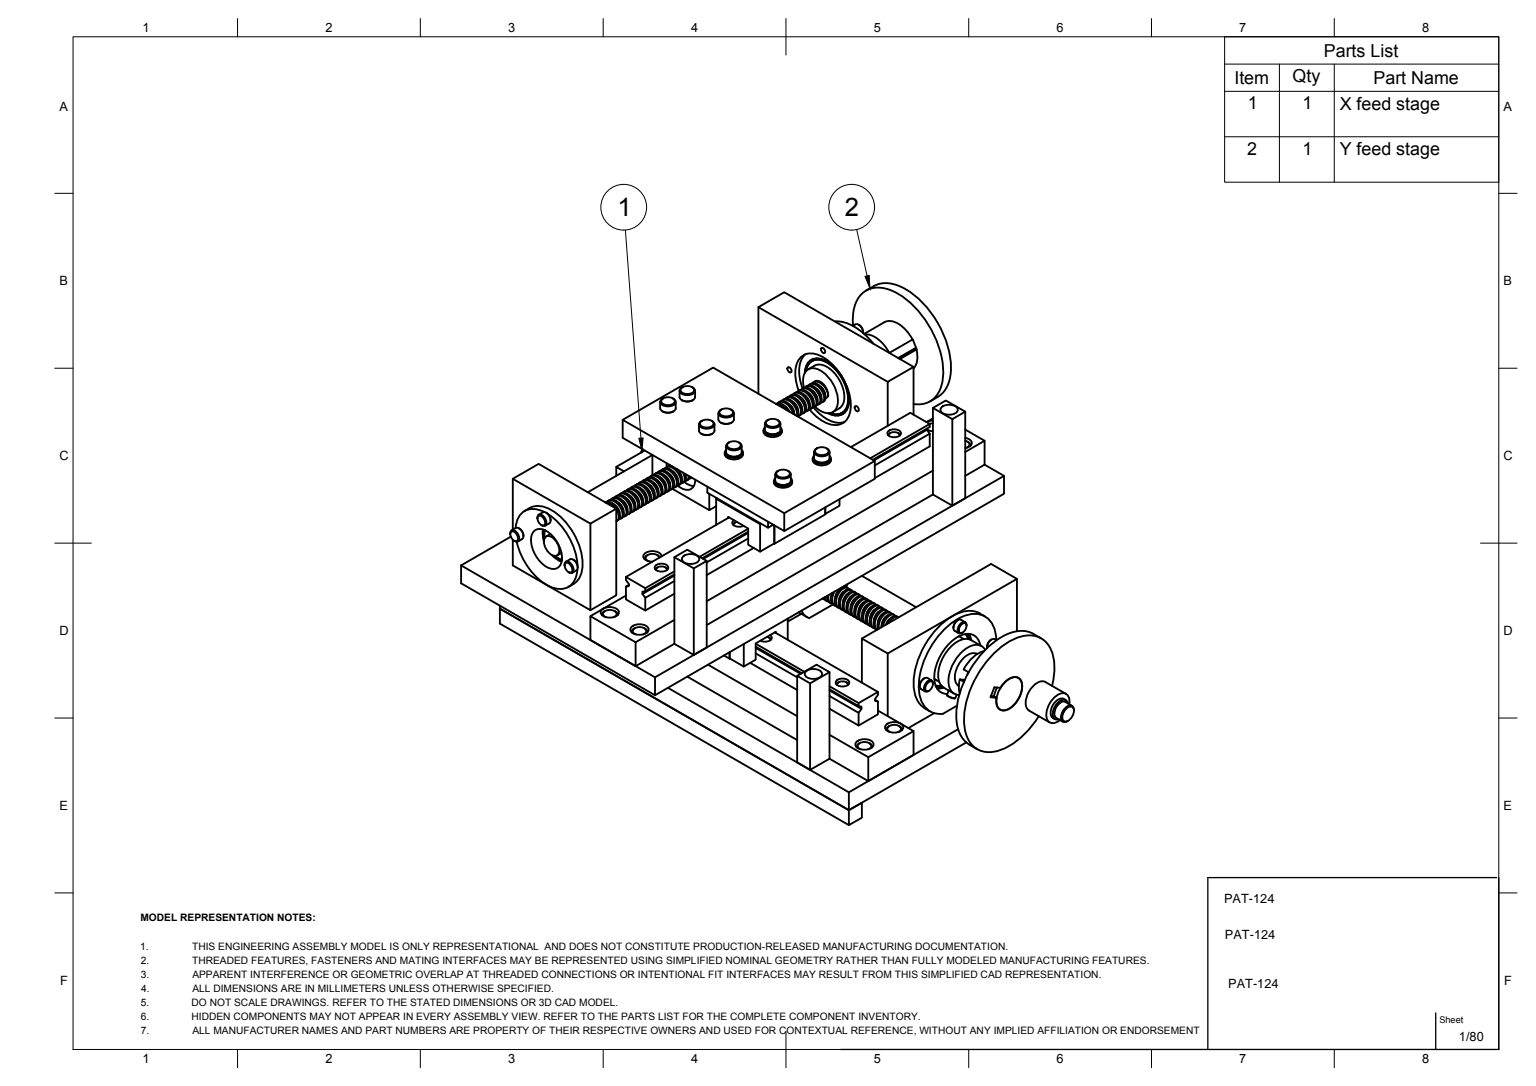
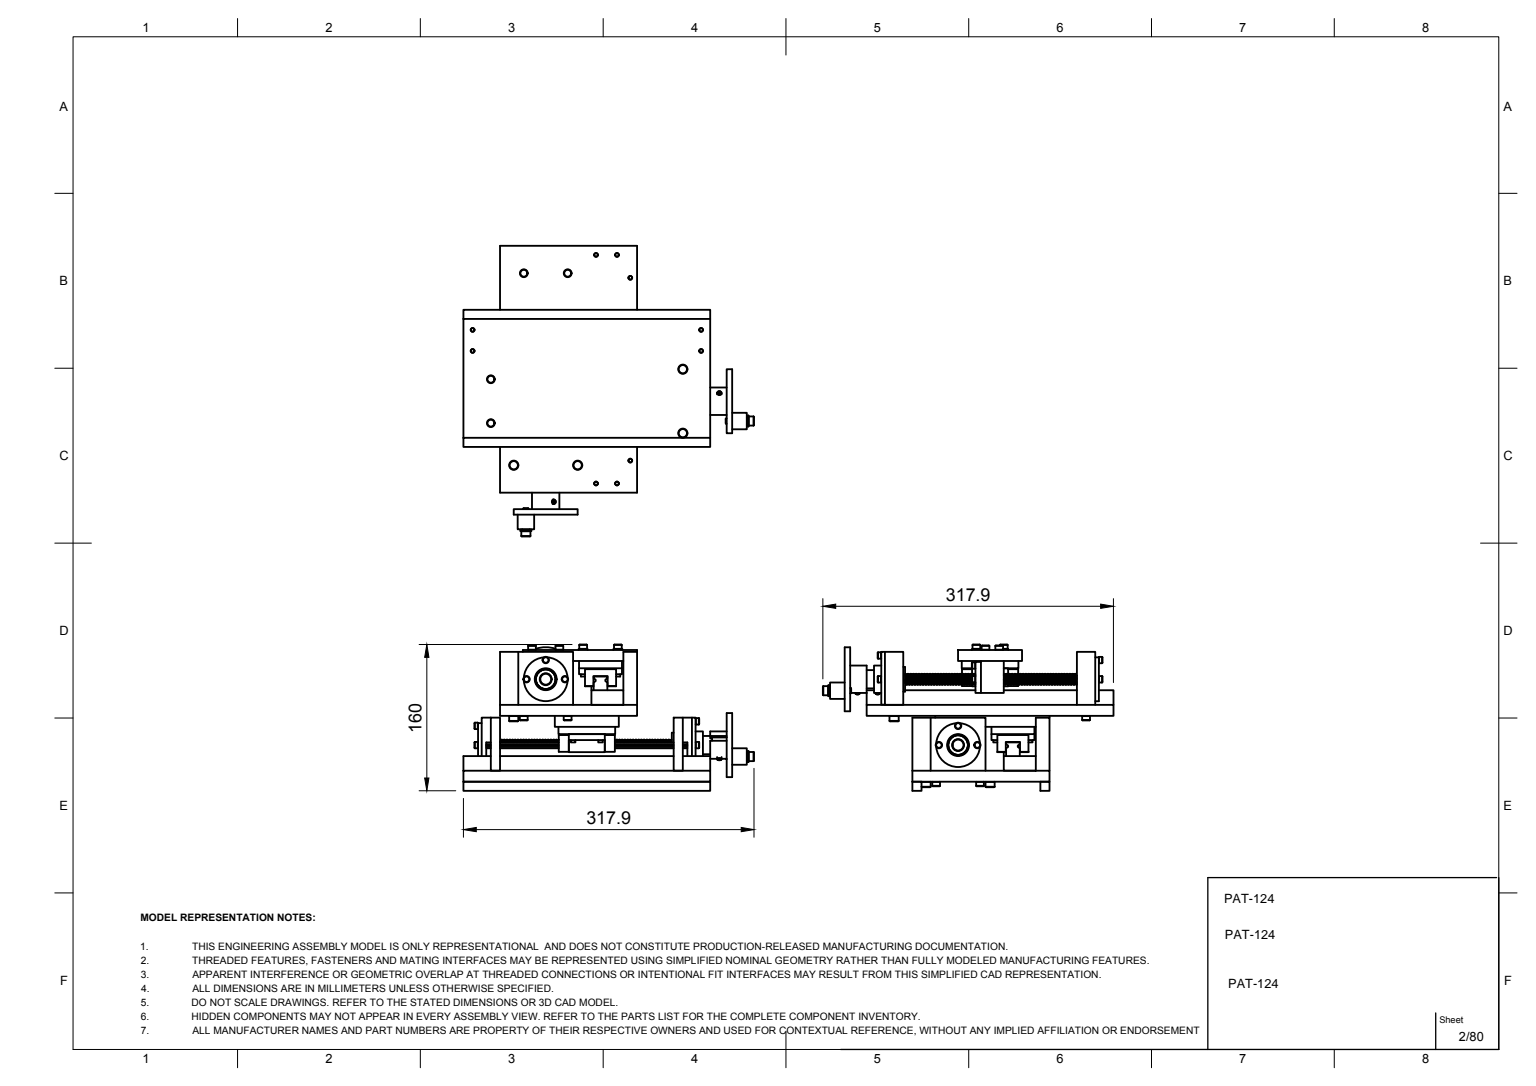
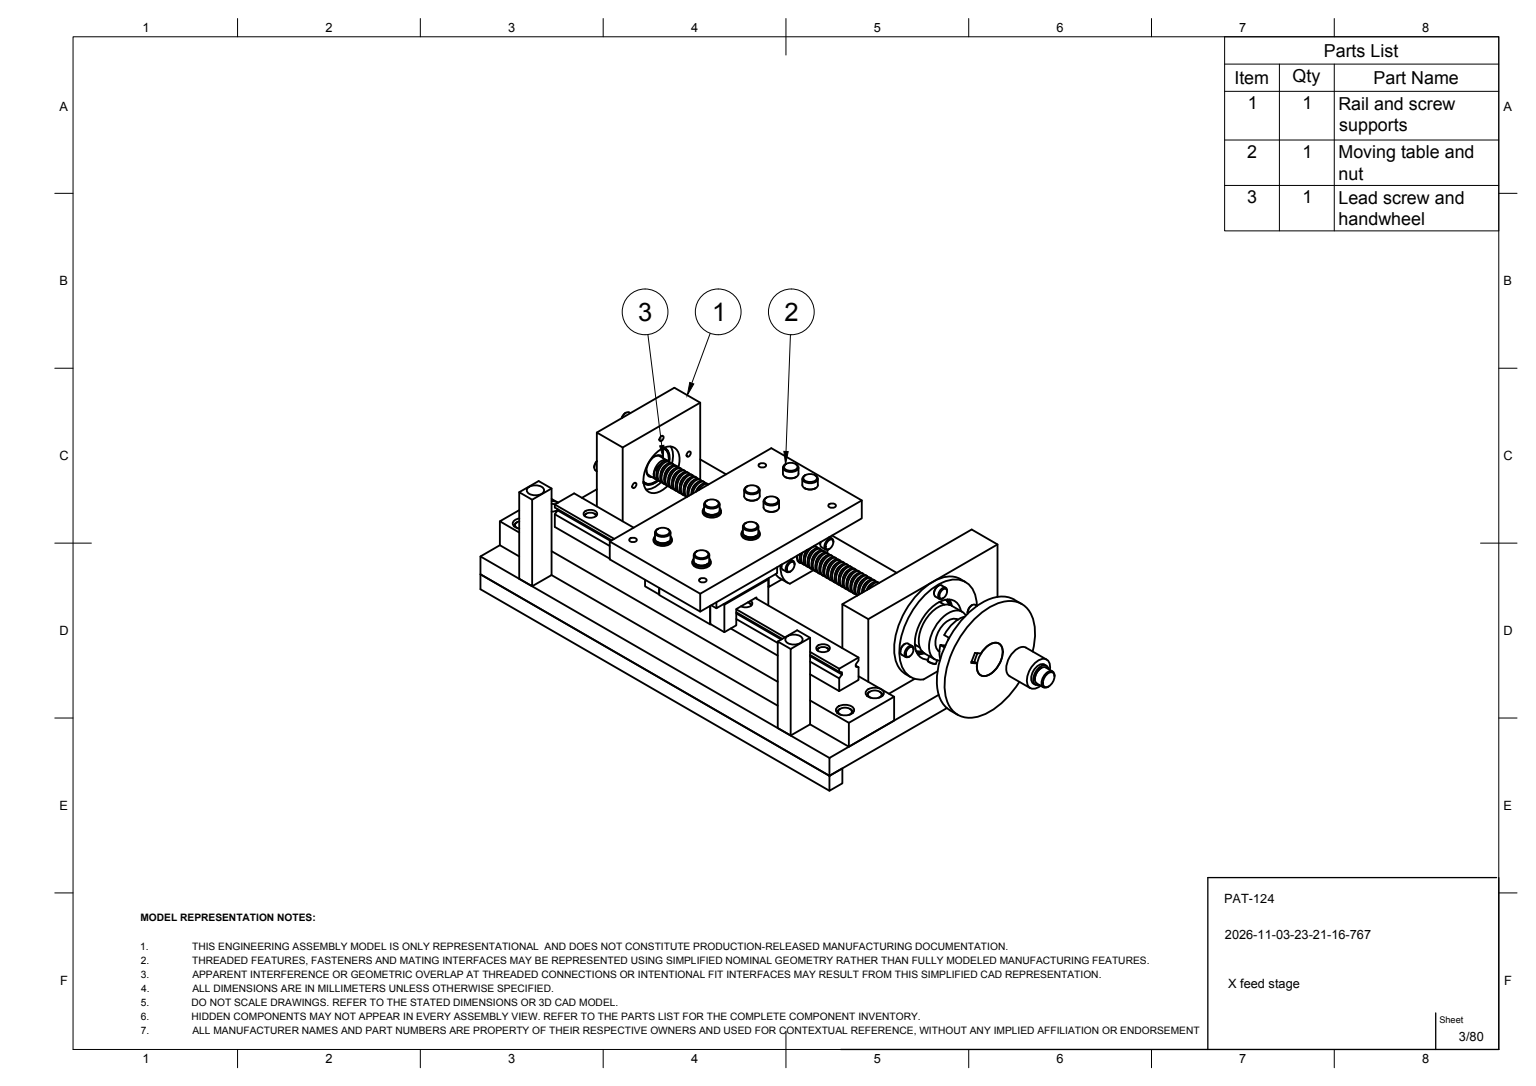
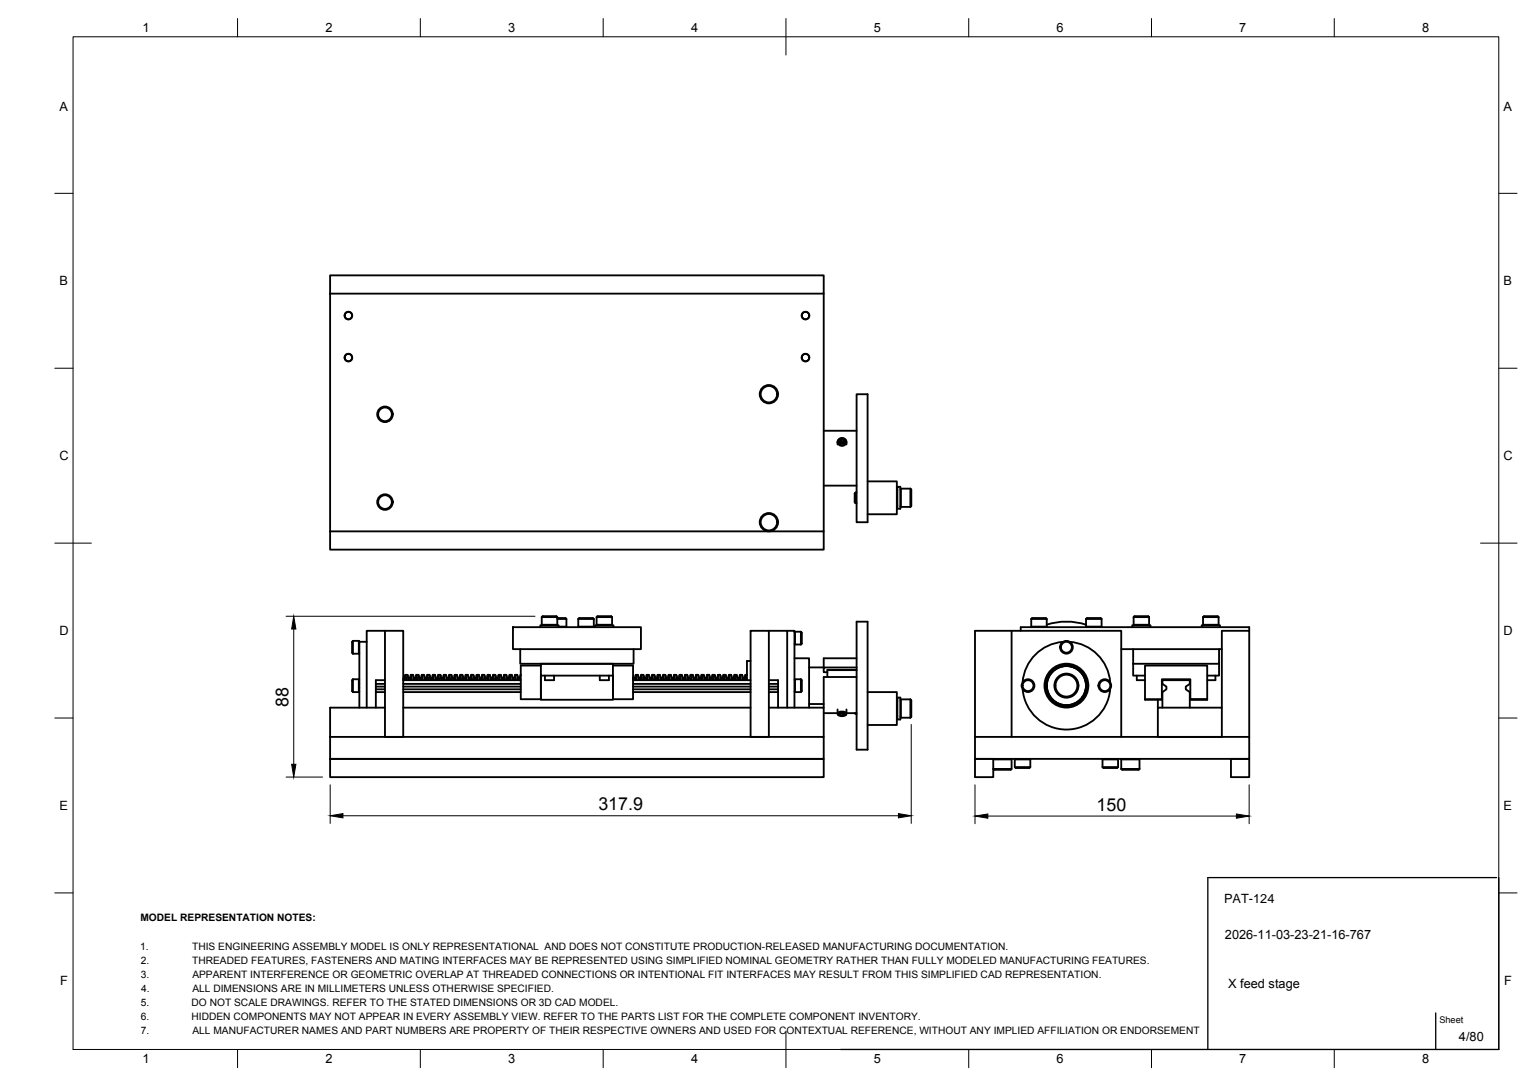
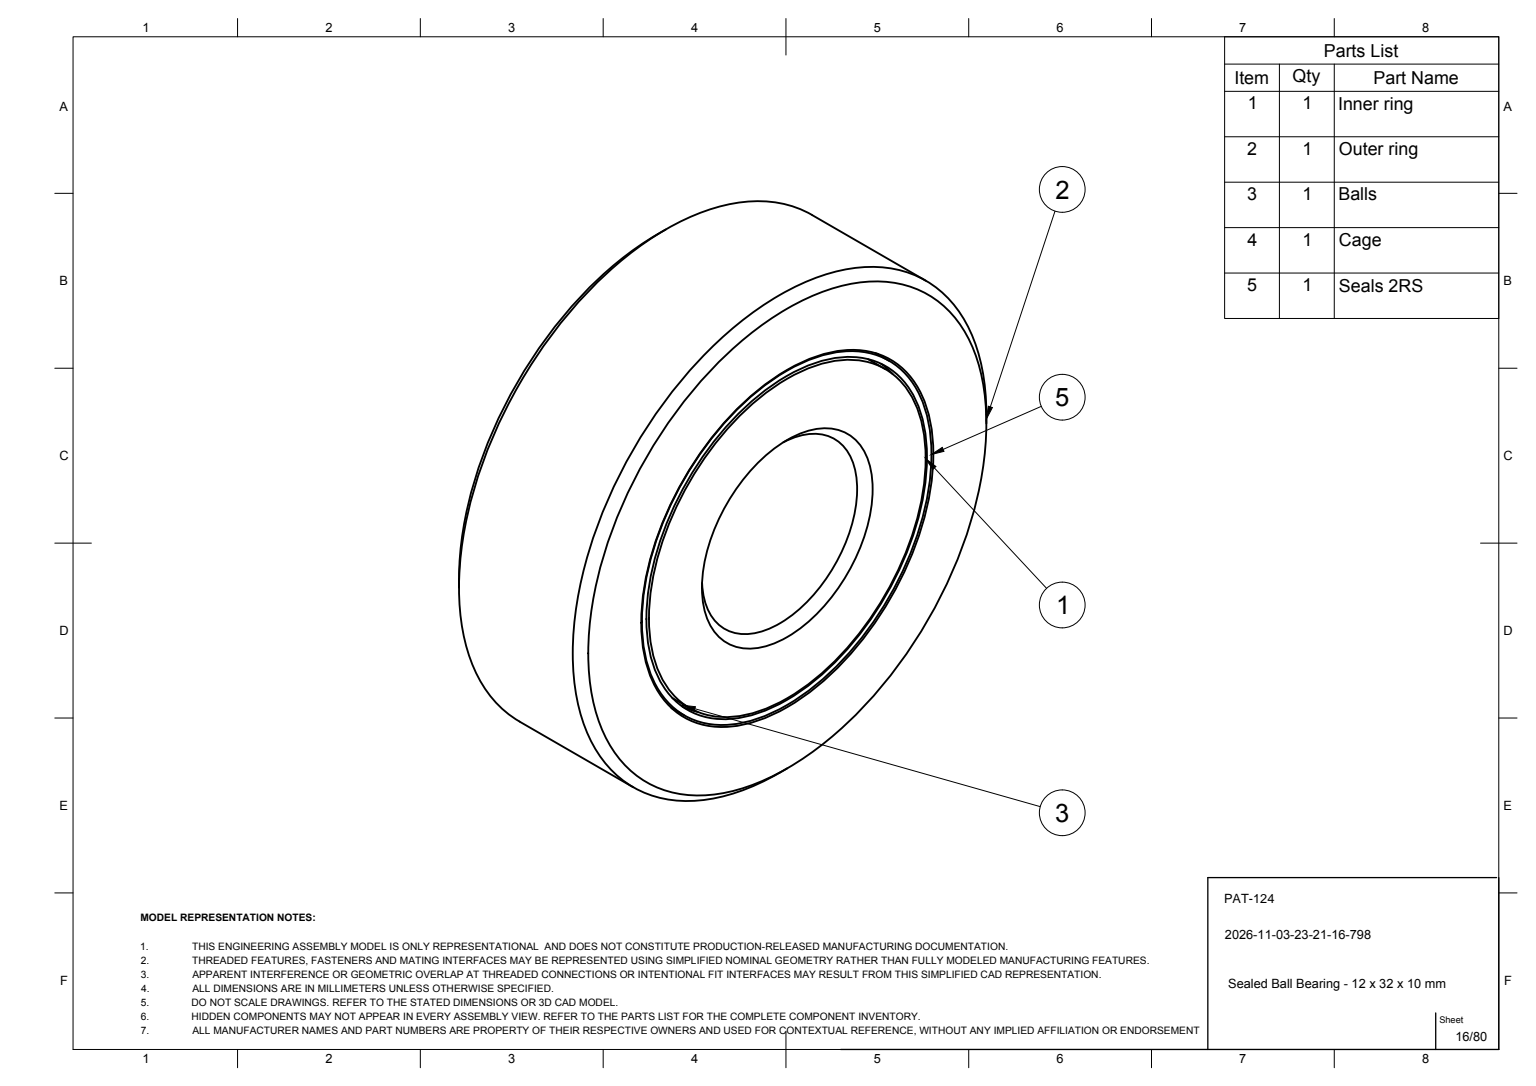
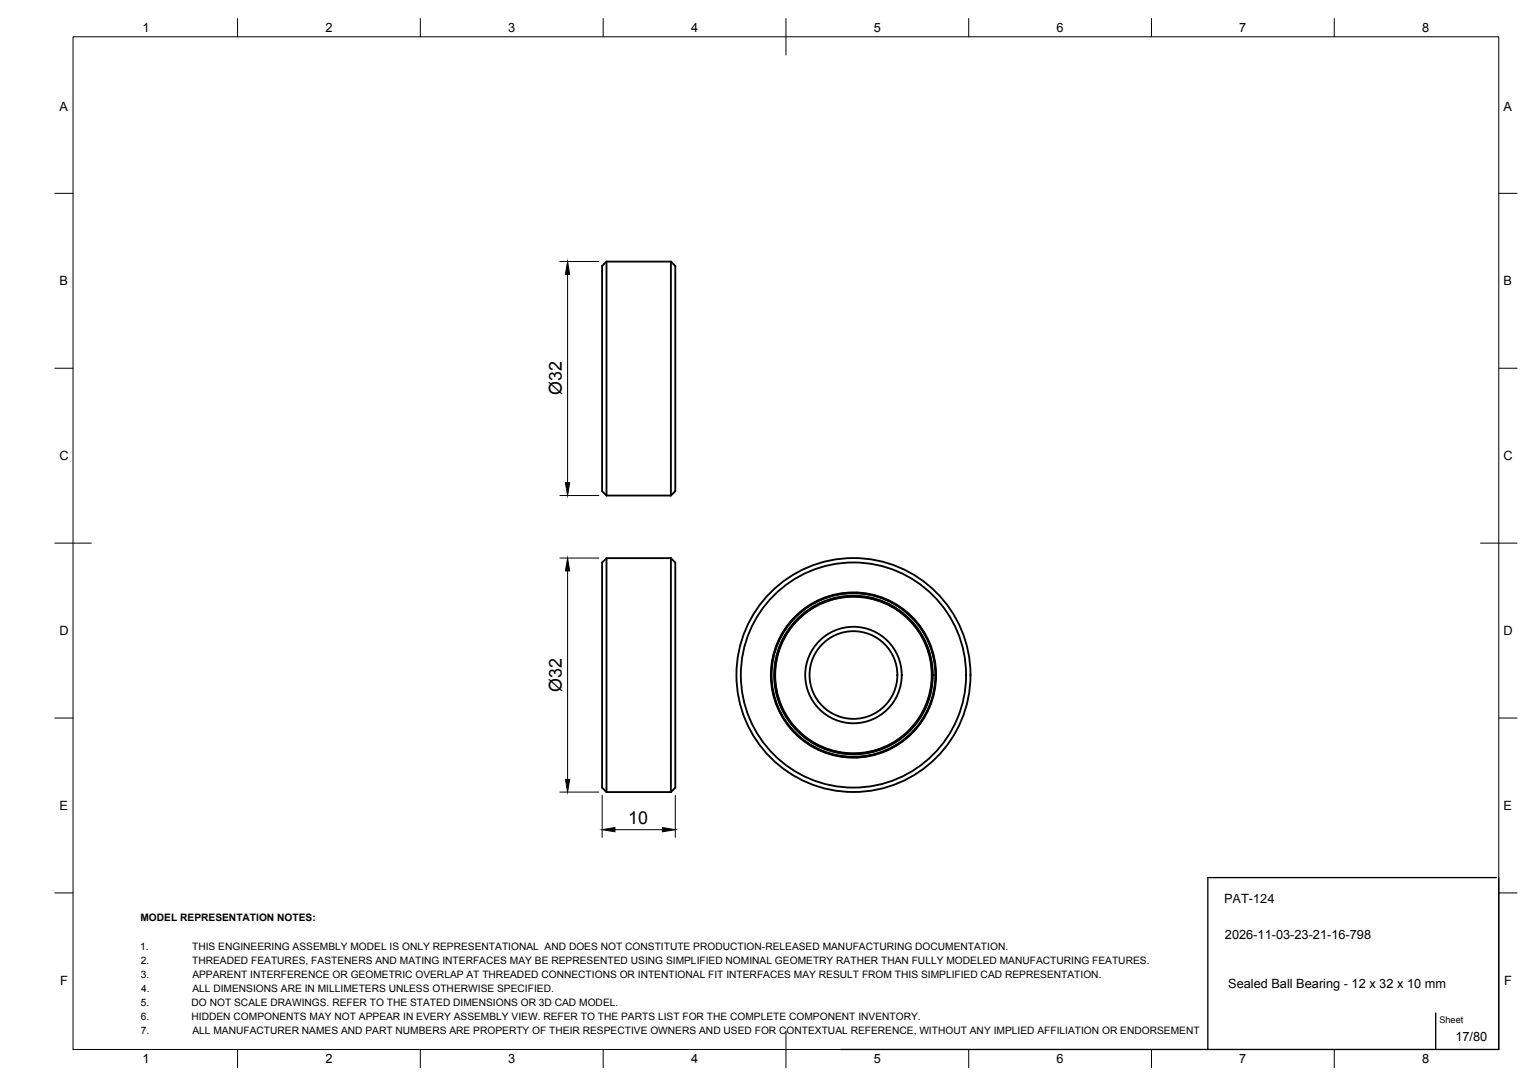
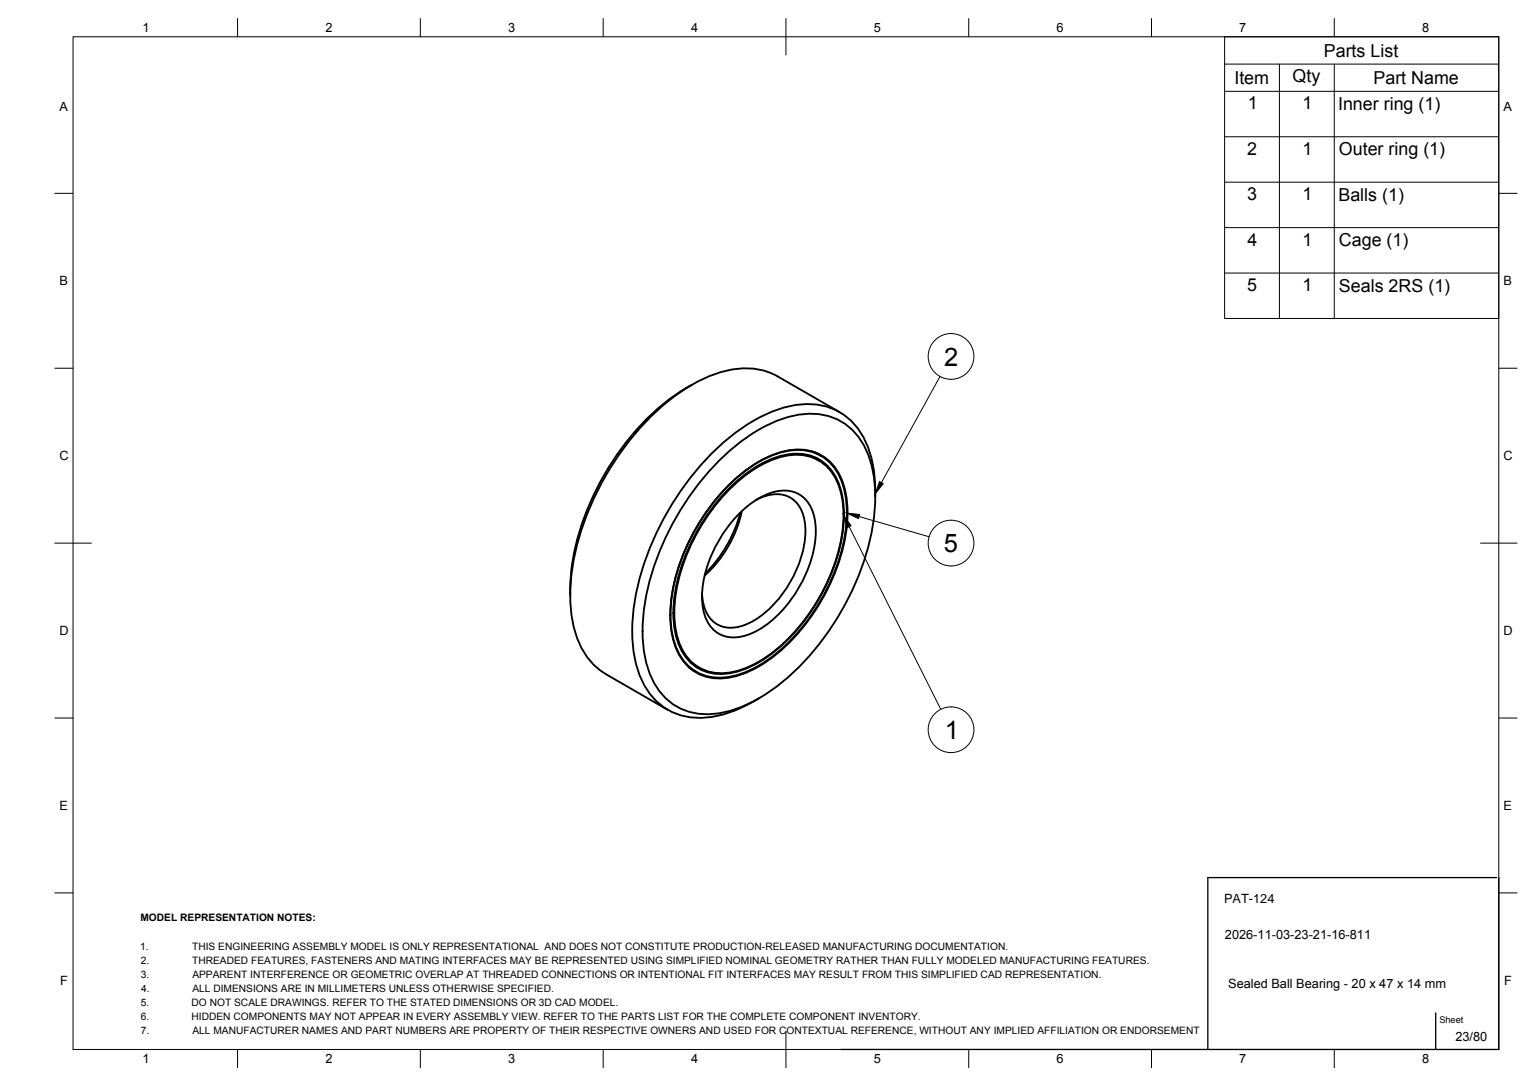
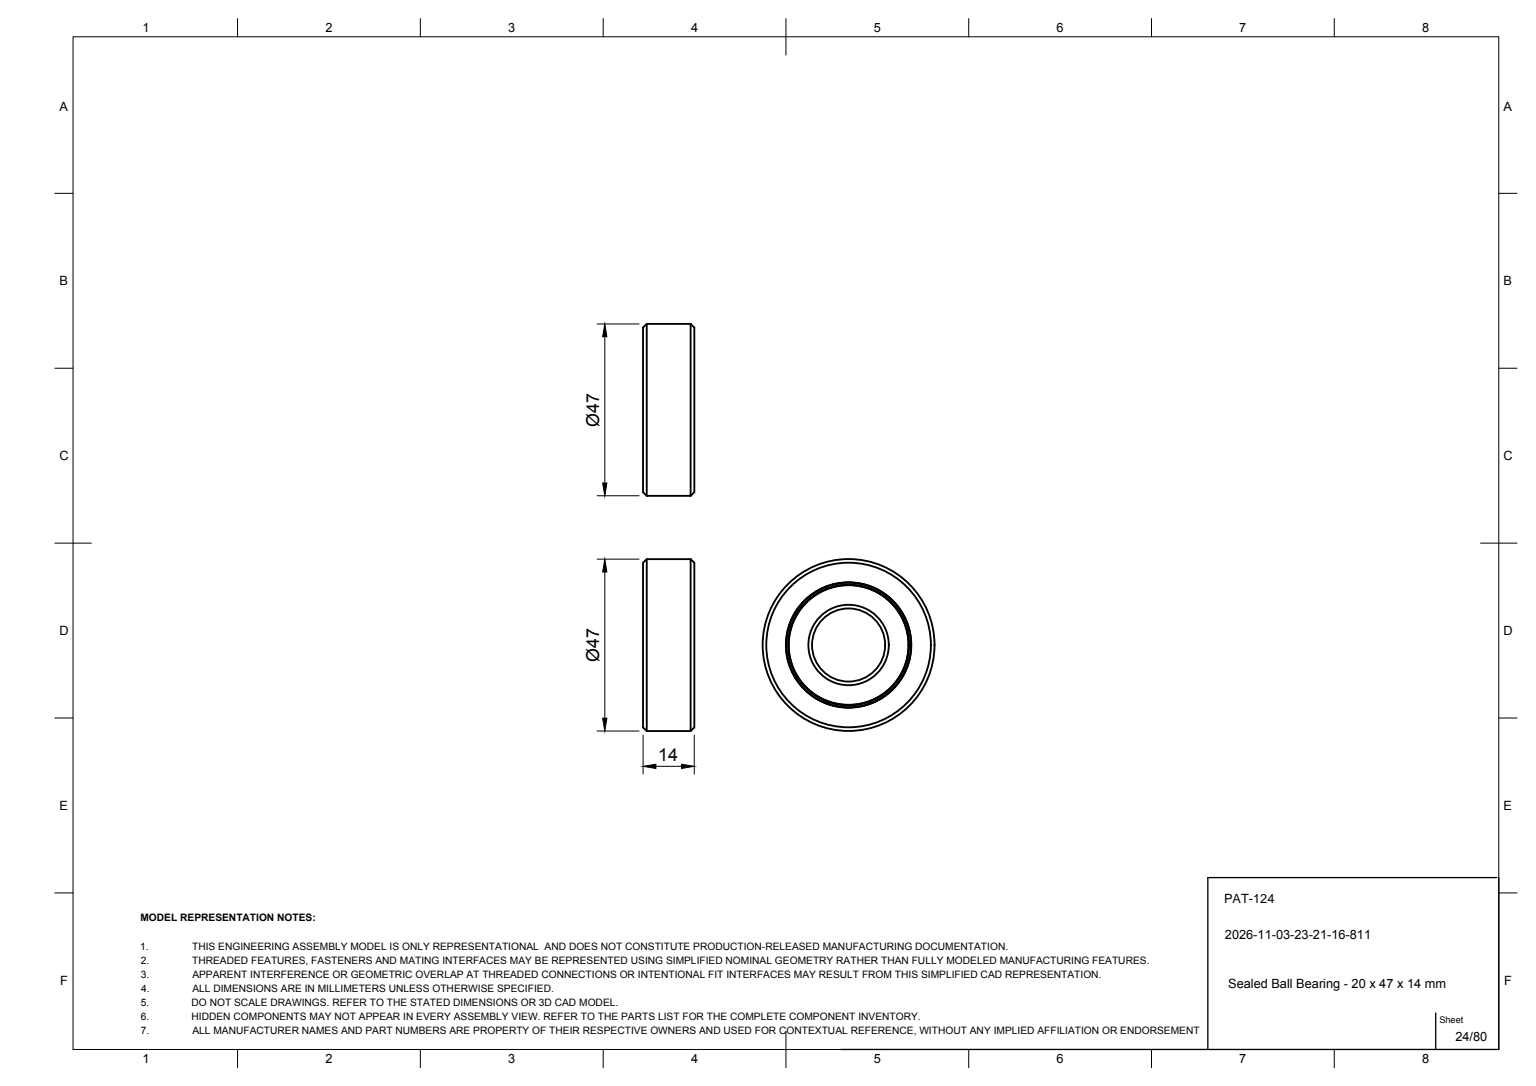
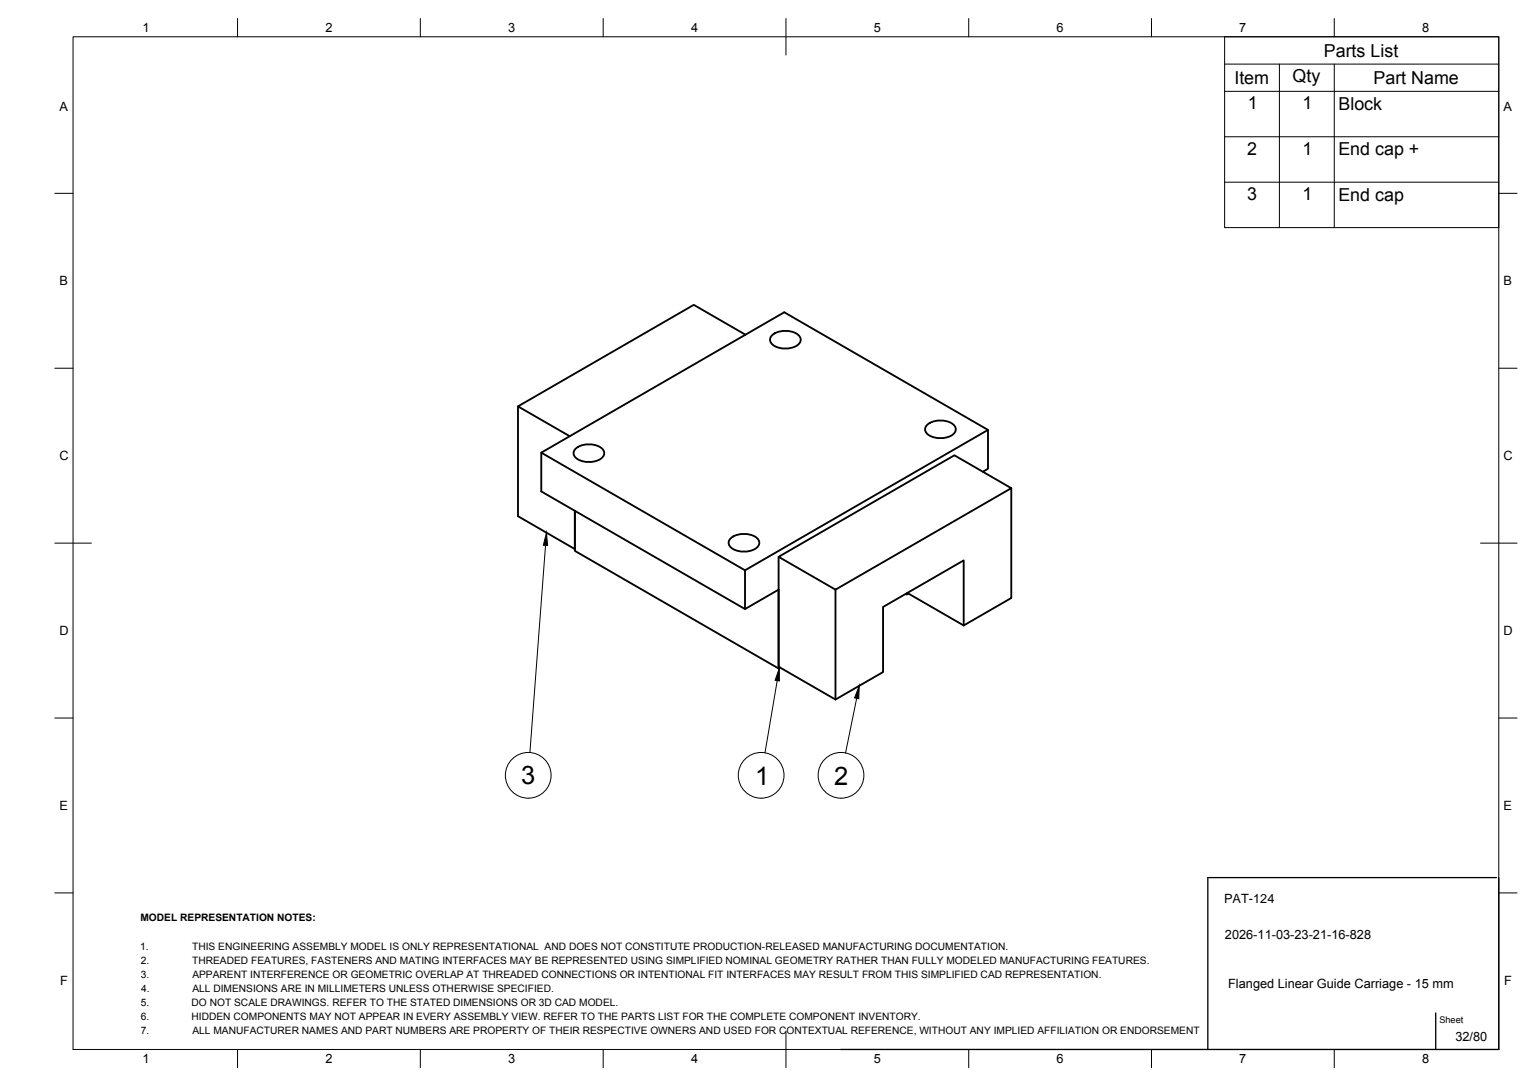
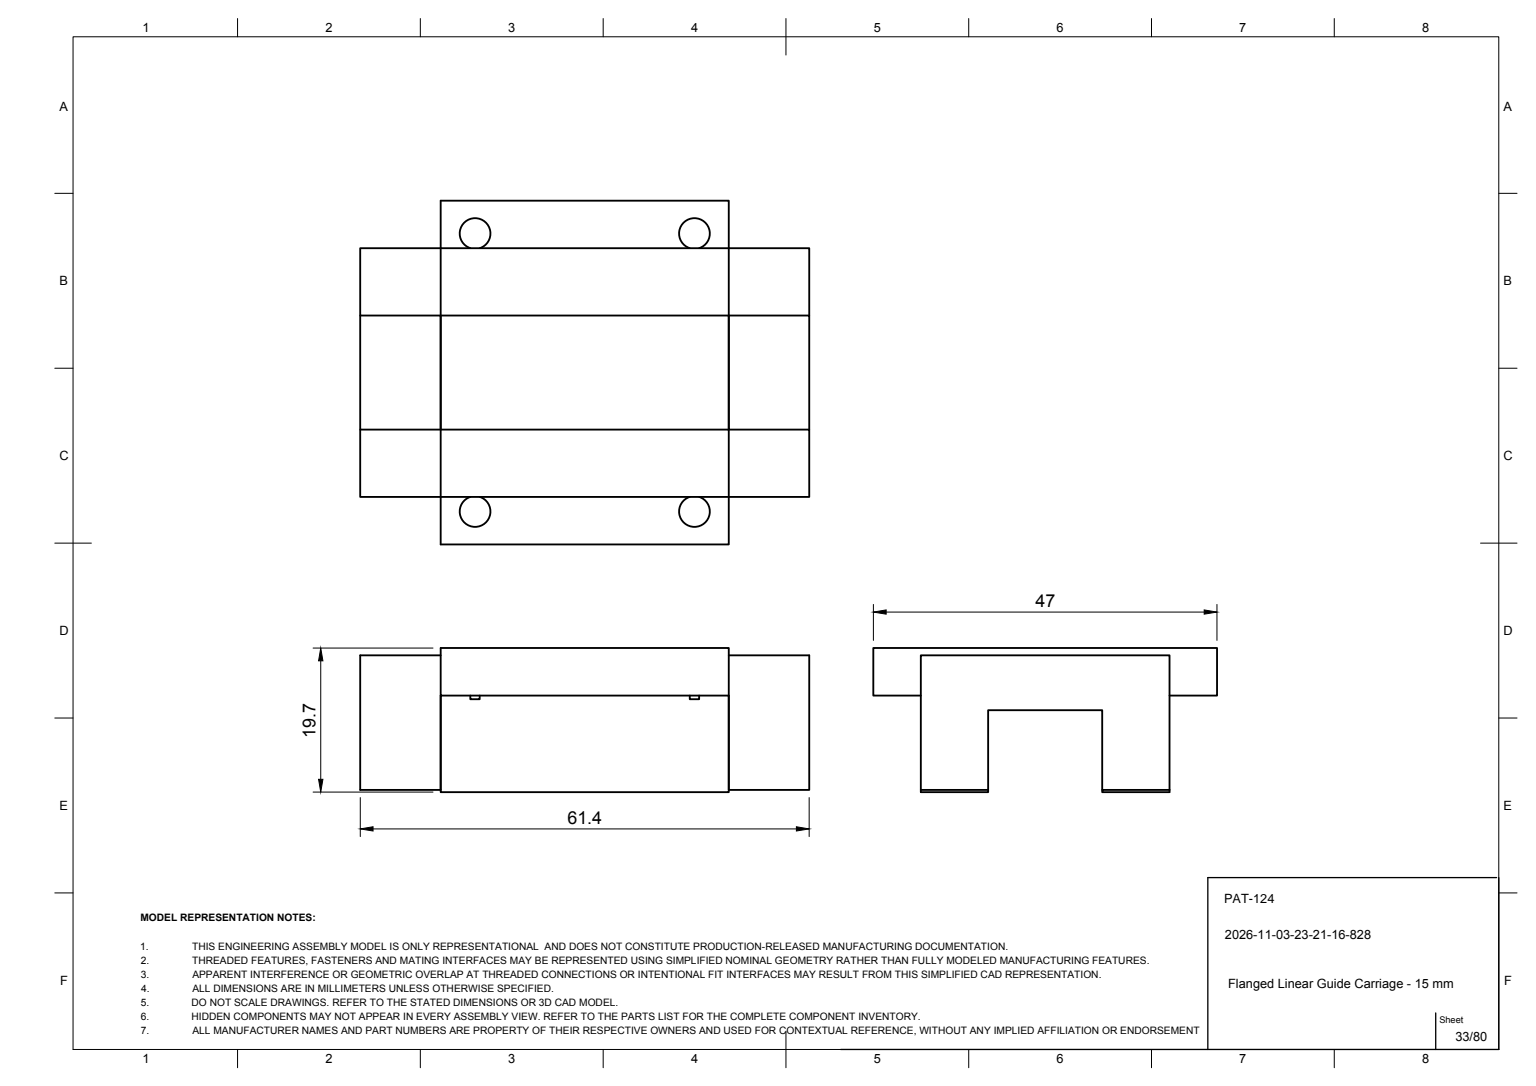
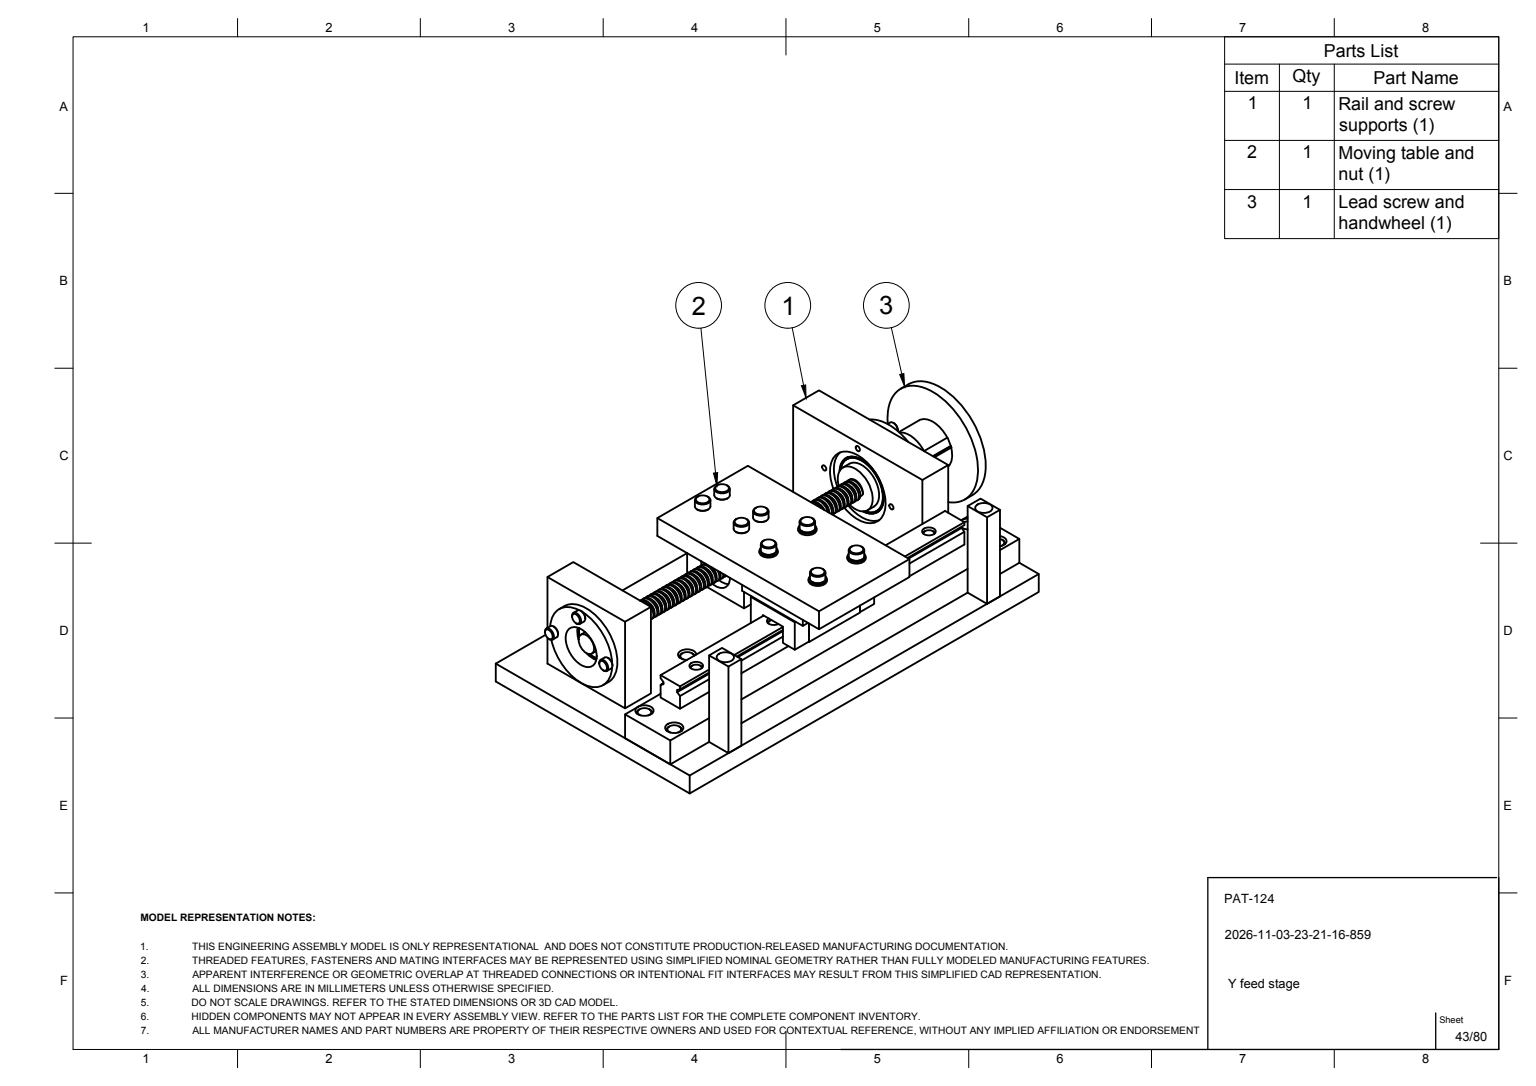
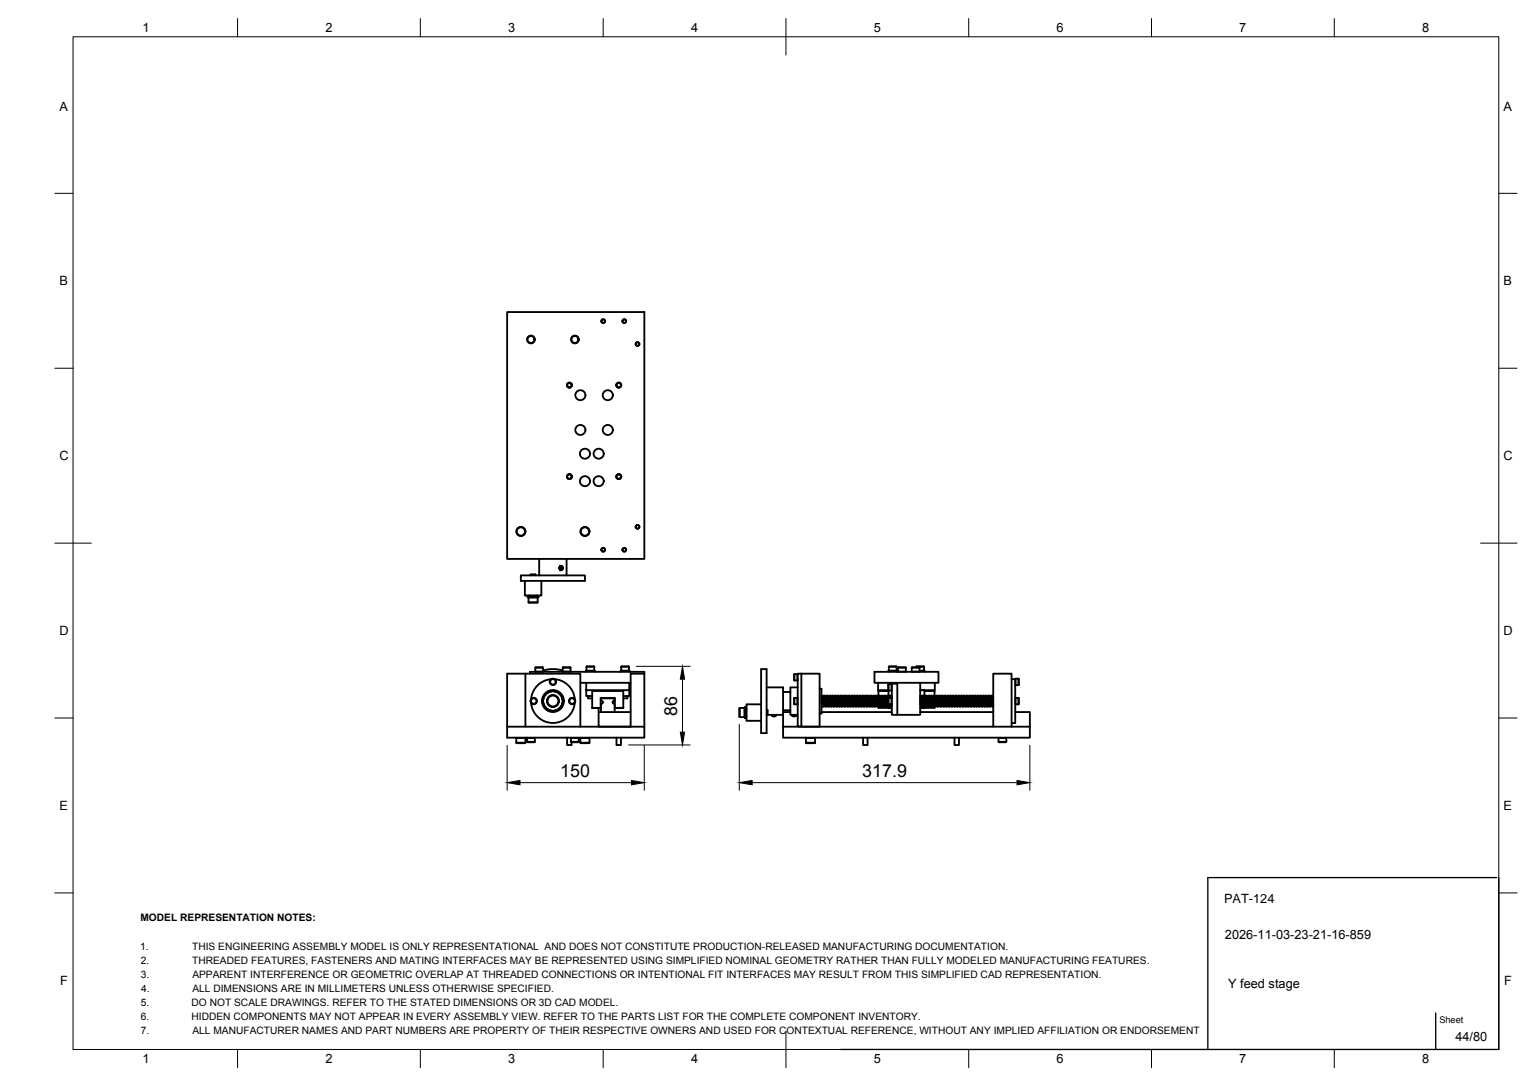
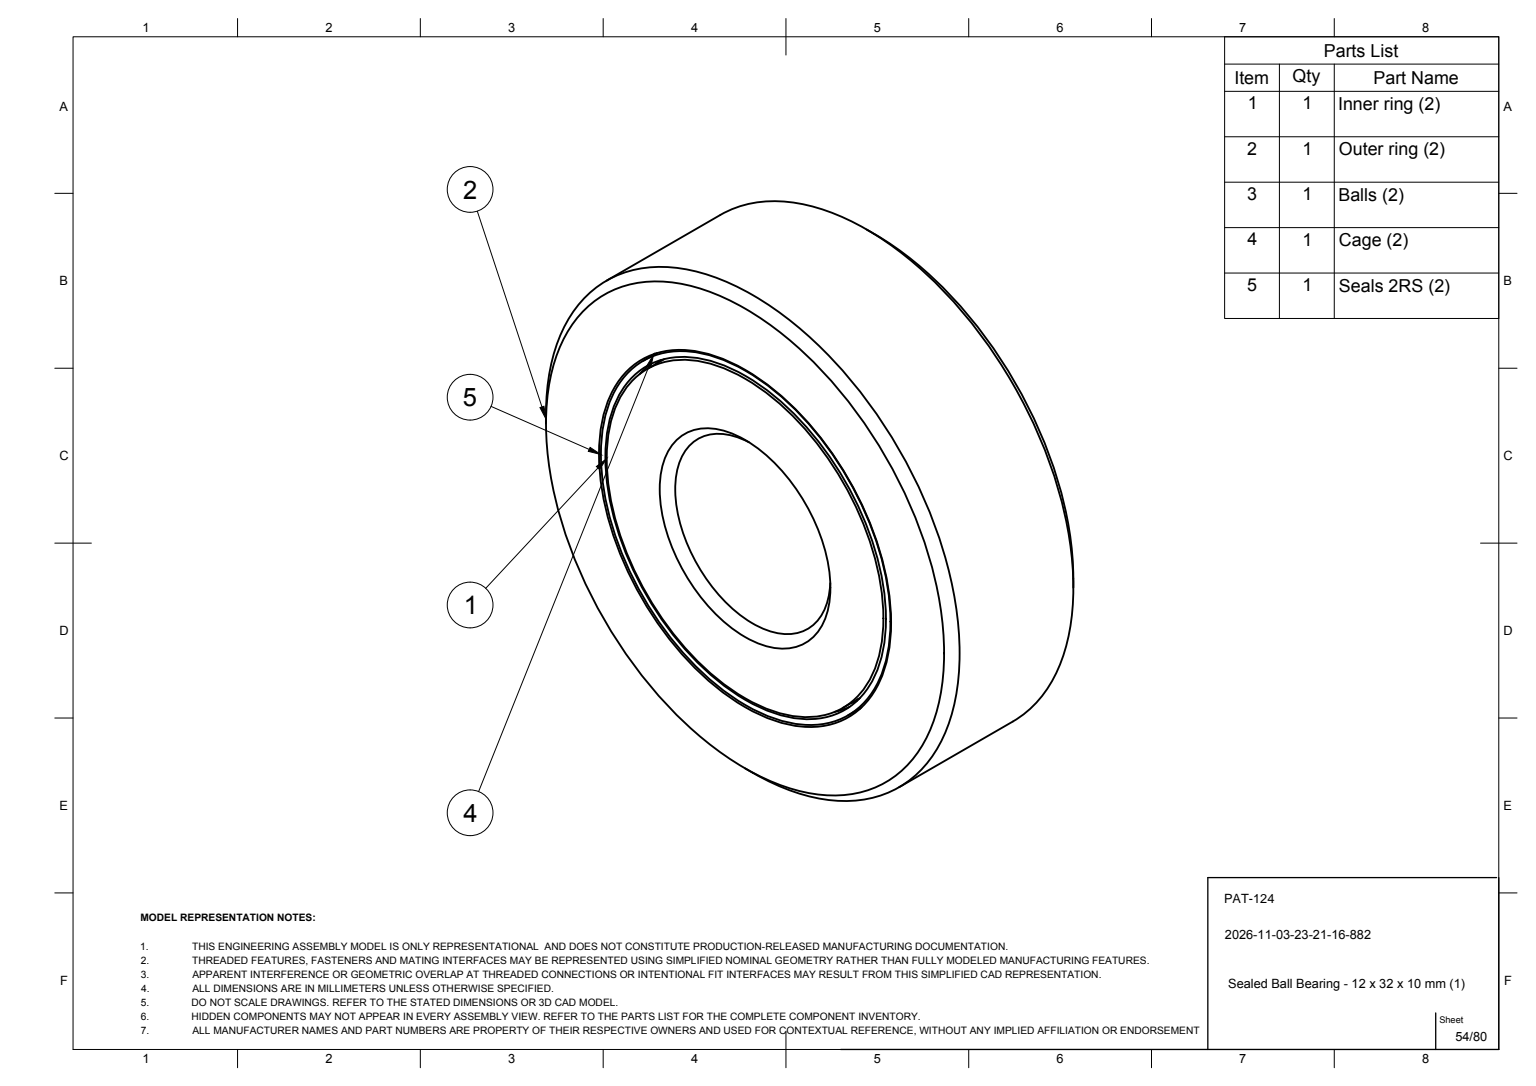
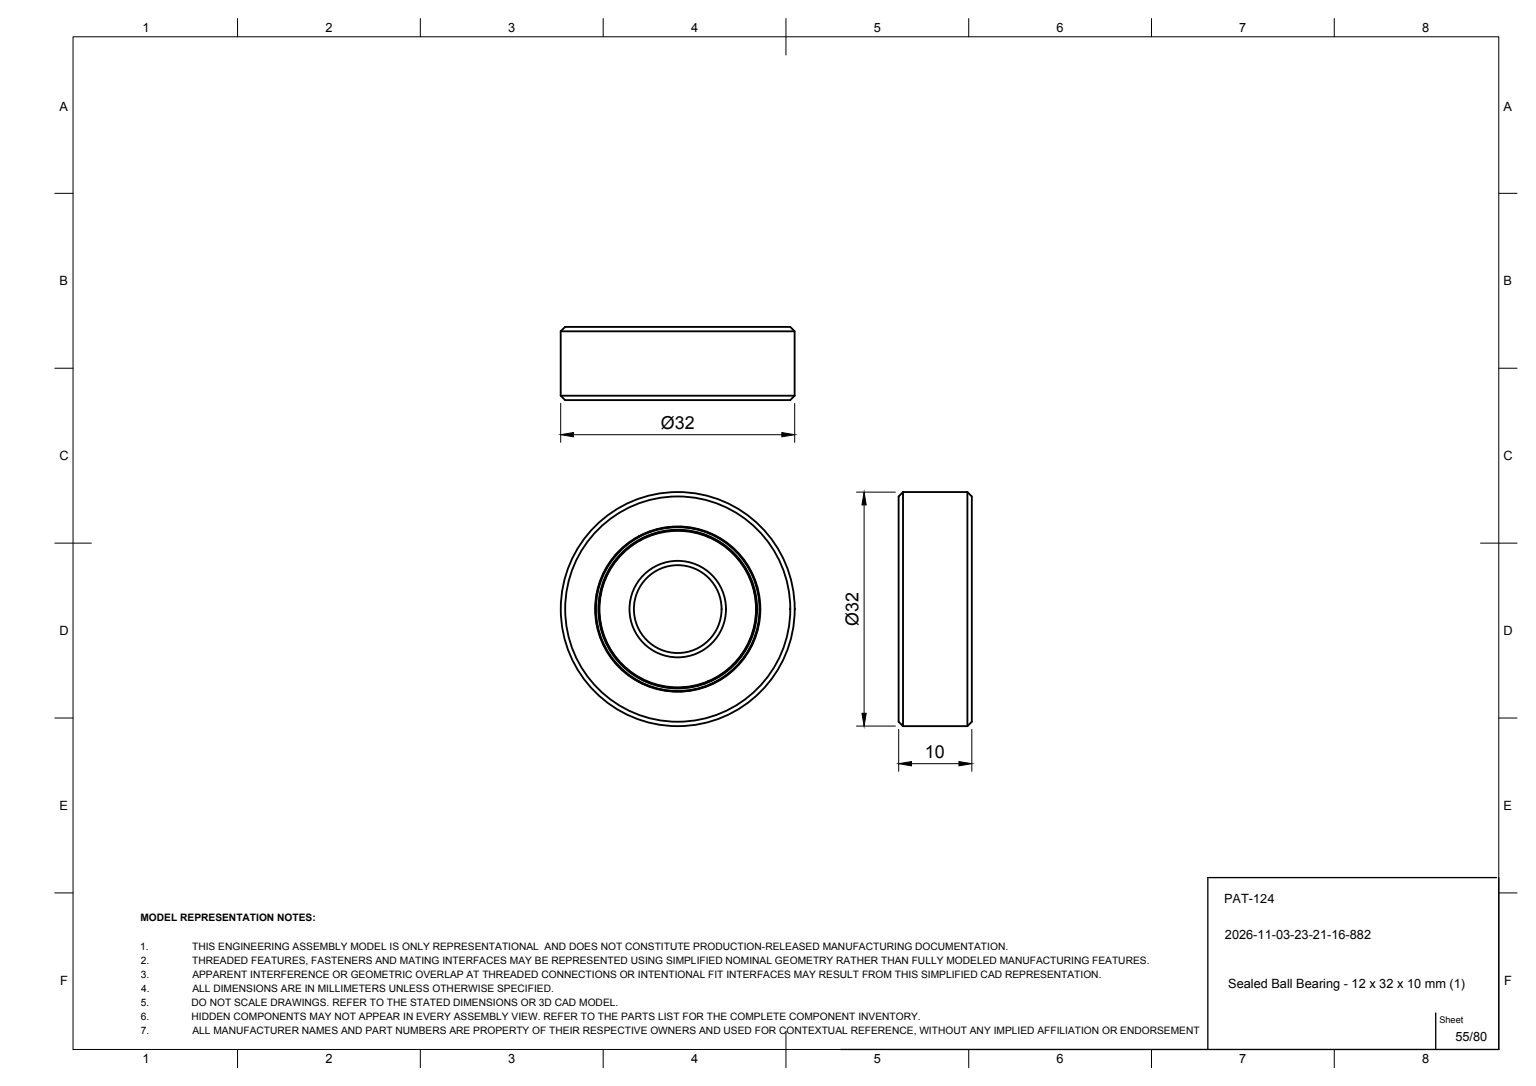
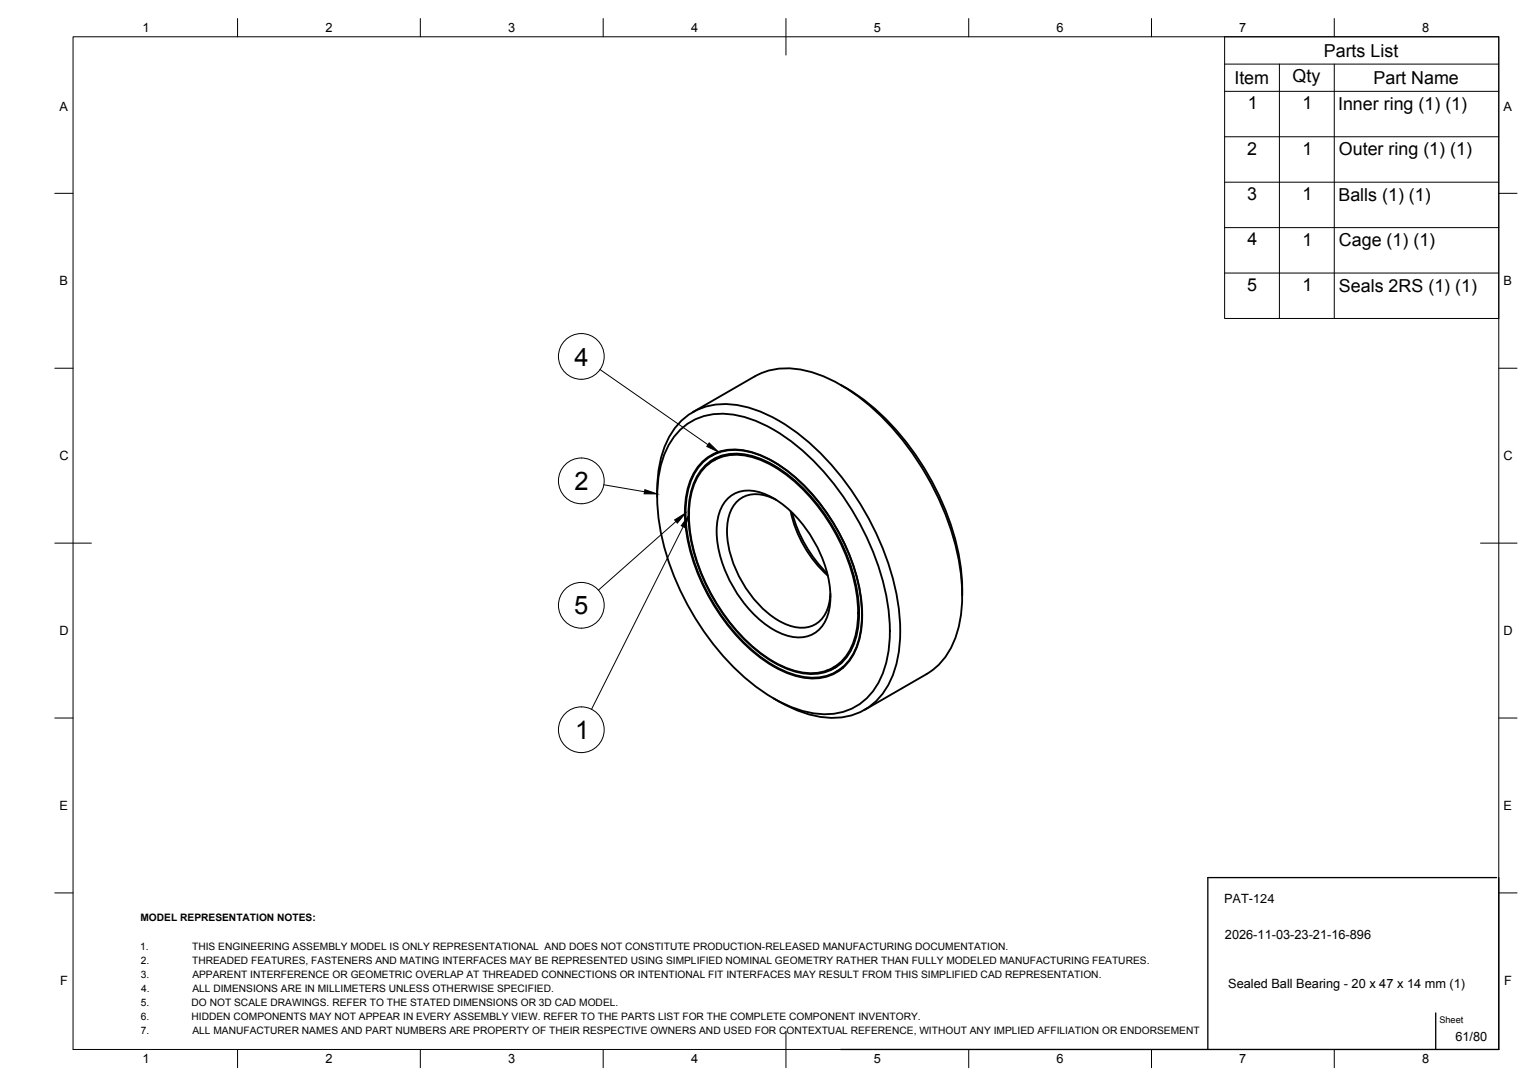
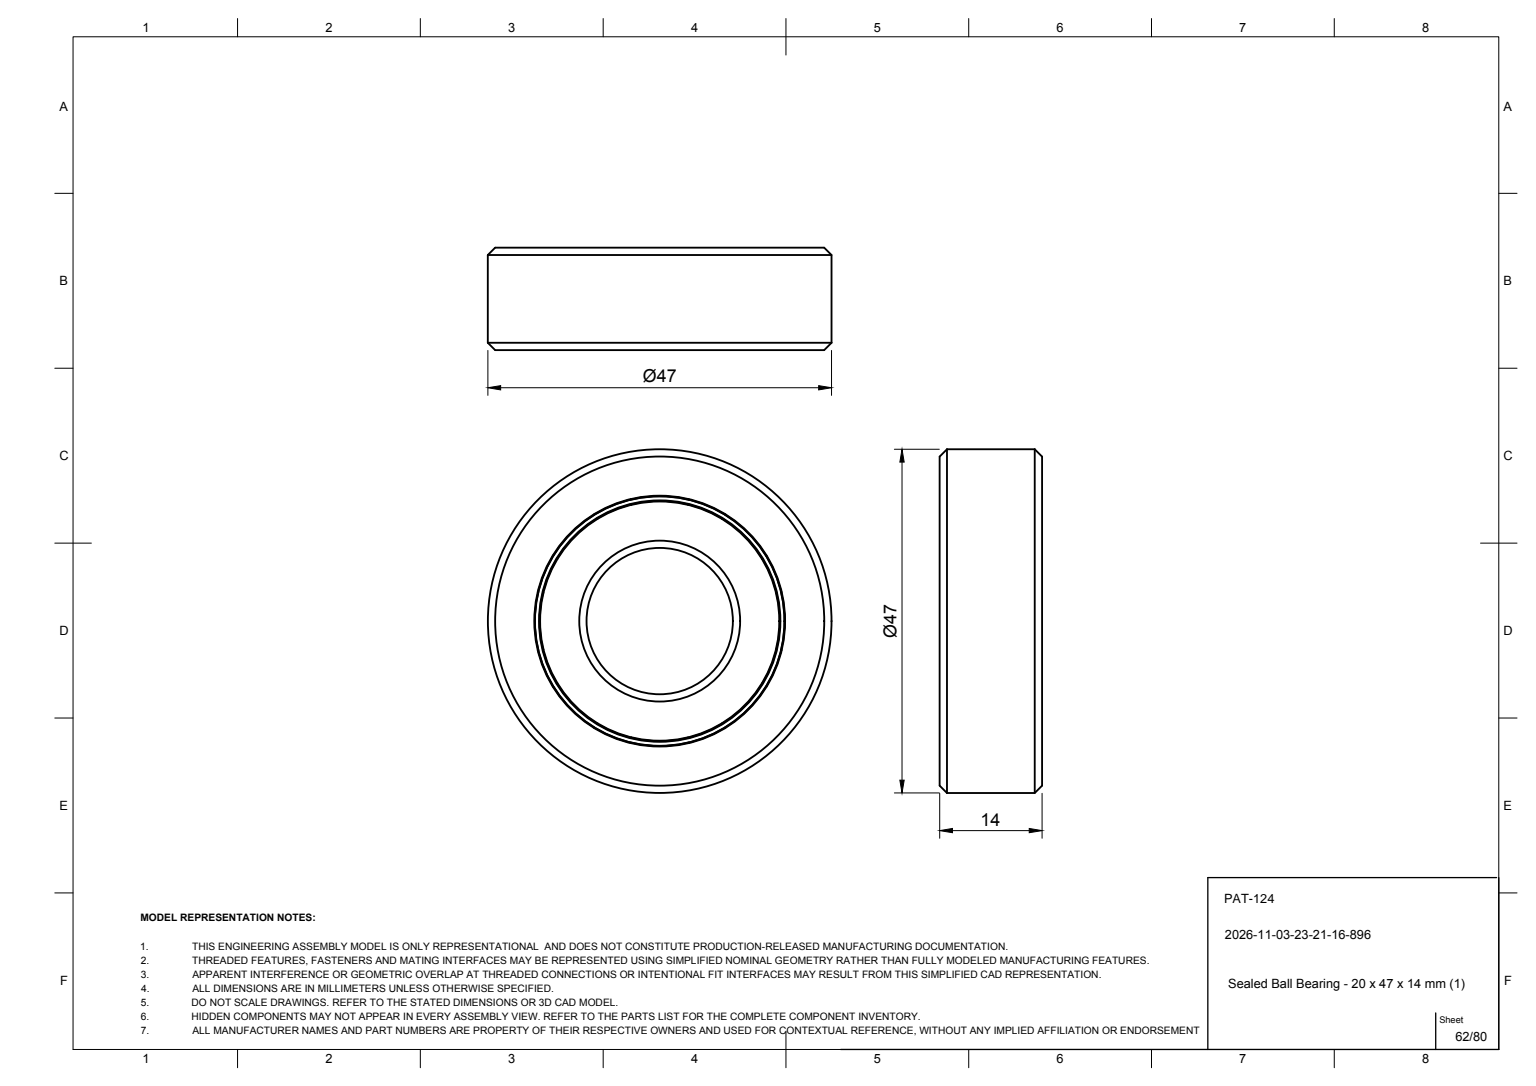
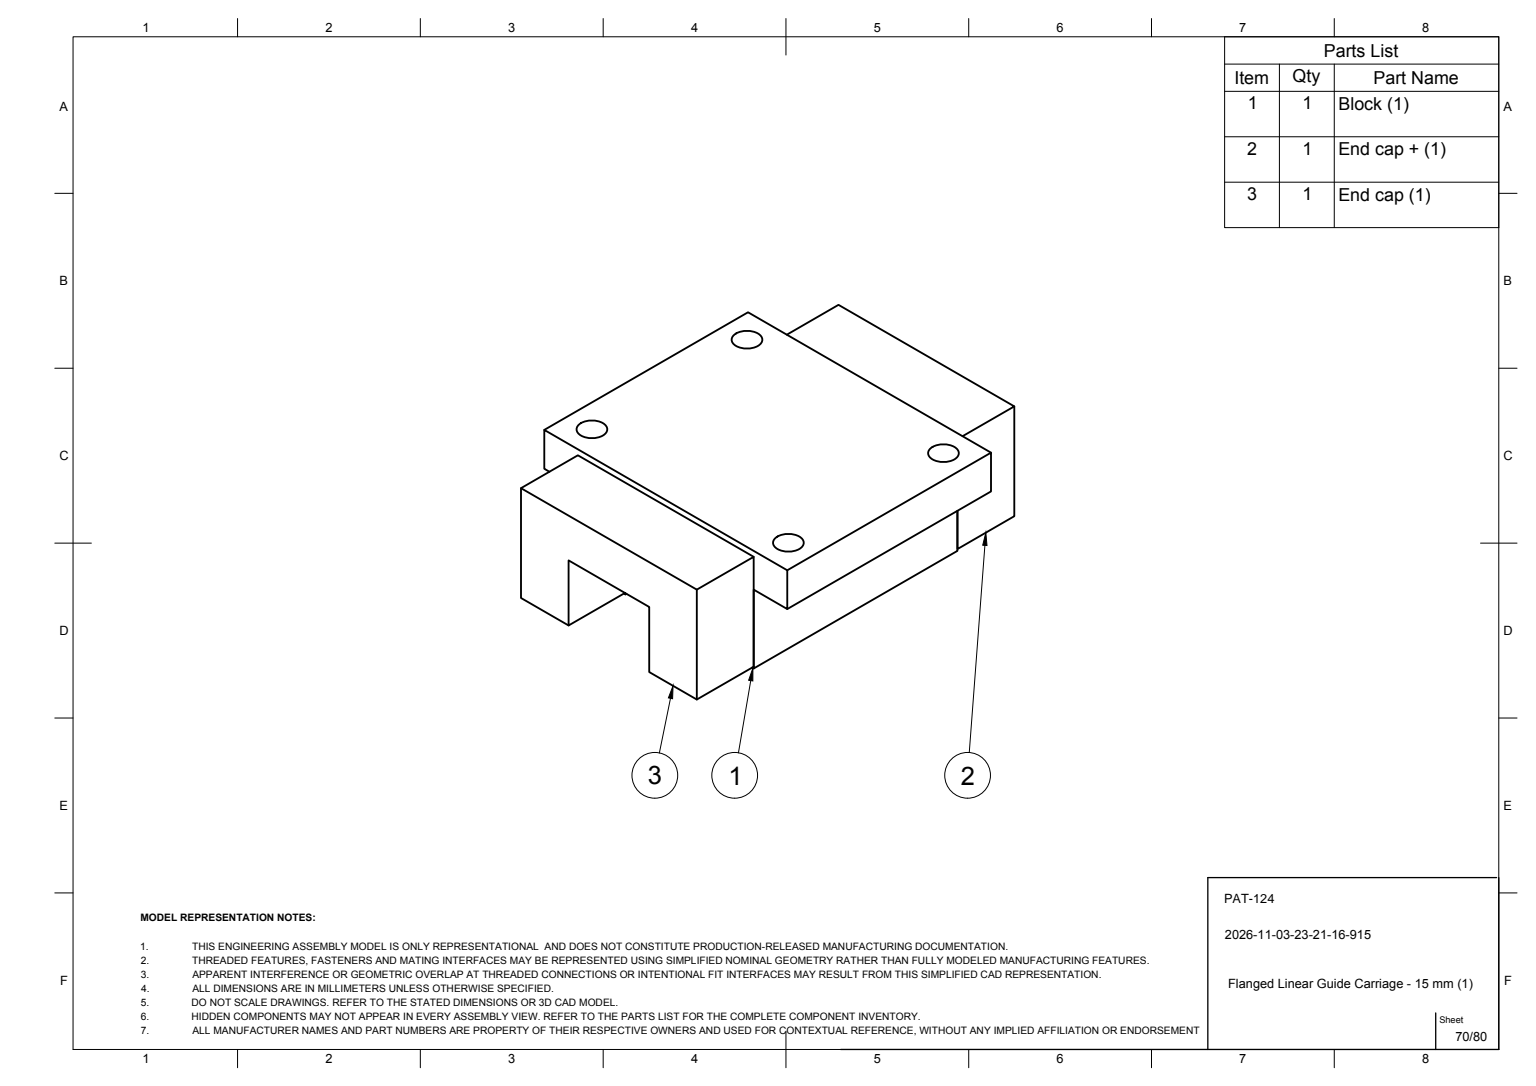
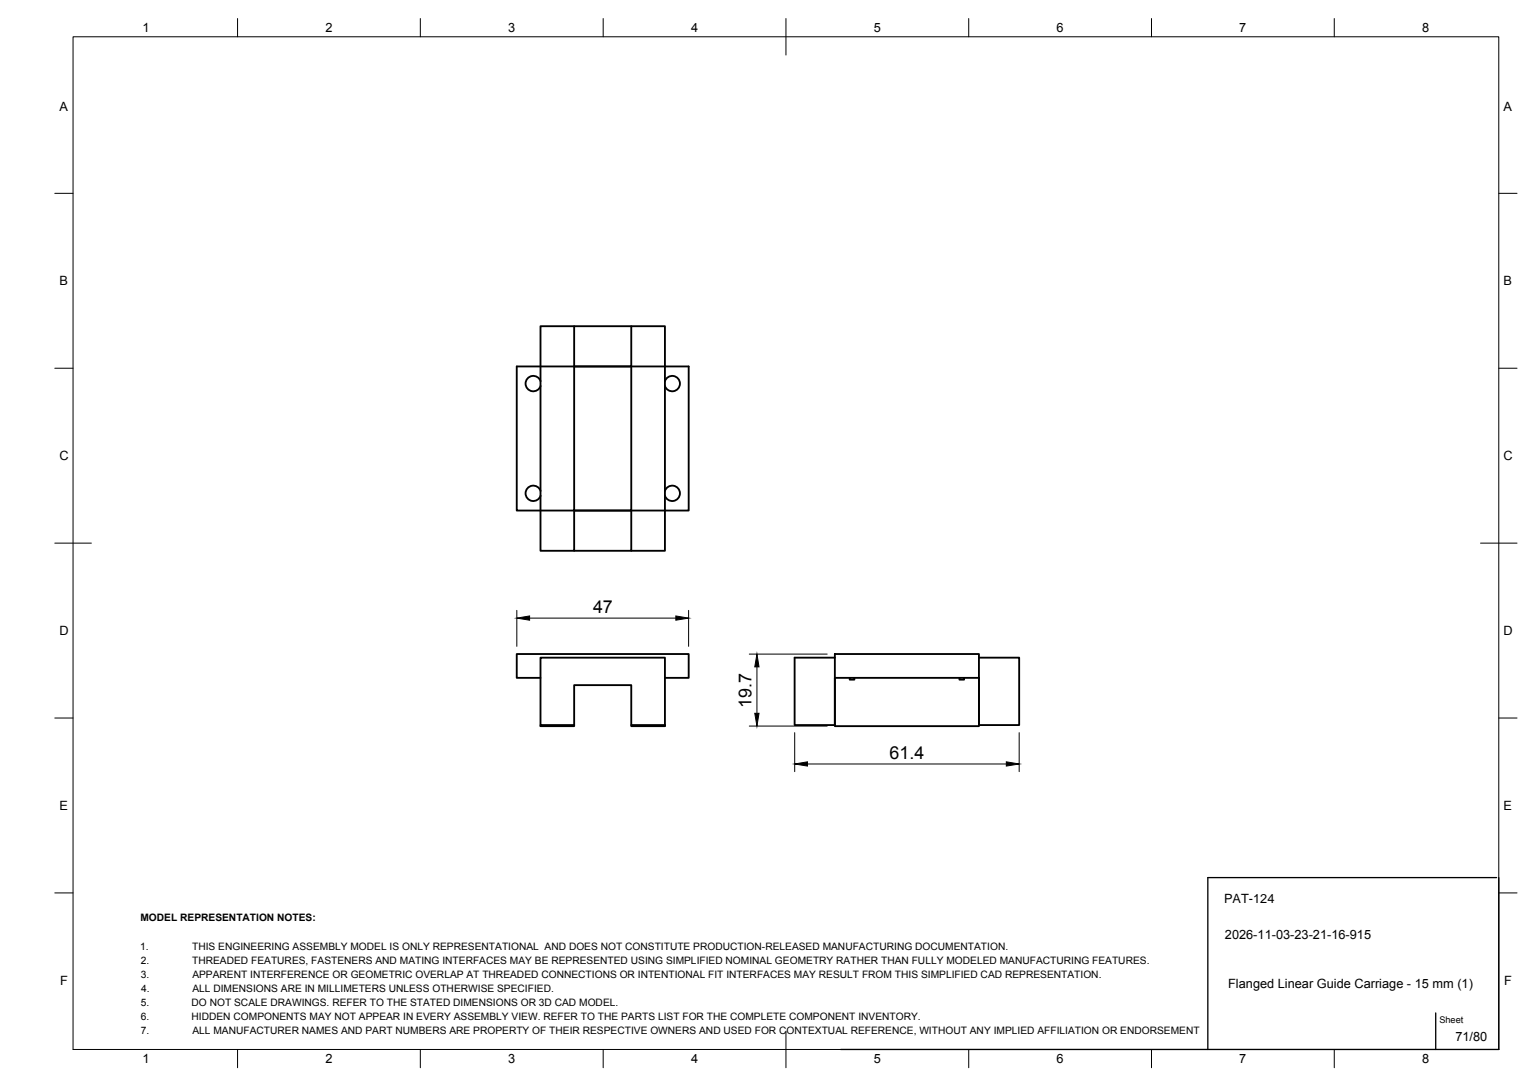
ISO-10303-21;
HEADER;
/* Generated by software containing ST-Developer
 * from STEP Tools, Inc. (www.steptools.com) 
 */

FILE_DESCRIPTION(
/* description */ ('XY cross-slide table'),
/* implementation_level */ '2;1');

FILE_NAME(
/* name */ 'PAT-124',
/* time_stamp */ '2026-10-28T03:22:46-07:00',
/* author */ (''),
/* organization */ (''),
/* preprocessor_version */ 'ST-DEVELOPER v20.2',
/* originating_system */ 'Autodesk Translation Framework v15.17.0.0',
/* authorisation */ '');

FILE_SCHEMA (('AUTOMOTIVE_DESIGN { 1 0 10303 214 3 1 1 }'));
ENDSEC;

DATA;
#10=MECHANICAL_DESIGN_GEOMETRIC_PRESENTATION_REPRESENTATION('',(#1670,#1671,
#1672,#1673,#1674,#1675,#1676,#1677,#1678,#1679,#1680,#1681,#1682,#1683,
#1684,#1685,#1686,#1687,#1688,#1689,#1690,#1691,#1692,#1693,#1694,#1695,
#1696,#1697,#1698,#1699,#1700,#1701,#1702,#1703,#1704,#1705,#1706,#1707,
#1708,#1709,#1710,#1711,#1712,#1713,#1714,#1715,#1716,#1717,#1718,#1719,
#1720,#1721,#1722,#1723,#1724,#1725,#1726,#1727,#1728,#1729,#1730,#1731,
#1732,#1733,#1734,#1735,#1736,#1737,#1738,#1739,#1740,#1741,#1742,#1743,
#1744,#1745,#1746,#1747,#1748,#1749,#1750,#1751,#1752,#1753,#1754,#1755,
#1756,#1757,#1758,#1759,#1760,#1761,#1762,#1763,#1764,#1765,#1766,#1767,
#1768,#1769,#1770,#1771,#1772,#1773,#1774,#1775,#1776,#1777,#1778,#1779,
#1780,#1781,#1782),#62984);
#11=B_SPLINE_SURFACE_WITH_KNOTS('',3,3,((#36306,#36307,#36308,#36309,#36310,
#36311,#36312,#36313,#36314,#36315,#36316,#36317,#36318,#36319,#36320,#36321,
#36322,#36323,#36324,#36325,#36326,#36327,#36328,#36329,#36330,#36331,#36332,
#36333,#36334,#36335,#36336,#36337,#36338,#36339,#36340,#36341,#36342,#36343,
#36344,#36345,#36346,#36347,#36348,#36349,#36350,#36351,#36352,#36353,#36354,
#36355,#36356,#36357,#36358,#36359,#36360,#36361,#36362,#36363,#36364,#36365,
#36366,#36367,#36368,#36369,#36370,#36371,#36372,#36373,#36374,#36375,#36376,
#36377,#36378,#36379,#36380,#36381,#36382,#36383,#36384,#36385,#36386,#36387,
#36388,#36389,#36390,#36391,#36392,#36393,#36394,#36395,#36396,#36397,#36398,
#36399,#36400,#36401,#36402,#36403,#36404,#36405,#36406,#36407,#36408,#36409,
#36410,#36411,#36412,#36413,#36414,#36415,#36416,#36417,#36418,#36419,#36420),
(#36421,#36422,#36423,#36424,#36425,#36426,#36427,#36428,#36429,#36430,
#36431,#36432,#36433,#36434,#36435,#36436,#36437,#36438,#36439,#36440,#36441,
#36442,#36443,#36444,#36445,#36446,#36447,#36448,#36449,#36450,#36451,#36452,
#36453,#36454,#36455,#36456,#36457,#36458,#36459,#36460,#36461,#36462,#36463,
#36464,#36465,#36466,#36467,#36468,#36469,#36470,#36471,#36472,#36473,#36474,
#36475,#36476,#36477,#36478,#36479,#36480,#36481,#36482,#36483,#36484,#36485,
#36486,#36487,#36488,#36489,#36490,#36491,#36492,#36493,#36494,#36495,#36496,
#36497,#36498,#36499,#36500,#36501,#36502,#36503,#36504,#36505,#36506,#36507,
#36508,#36509,#36510,#36511,#36512,#36513,#36514,#36515,#36516,#36517,#36518,
#36519,#36520,#36521,#36522,#36523,#36524,#36525,#36526,#36527,#36528,#36529,
#36530,#36531,#36532,#36533,#36534,#36535),(#36536,#36537,#36538,#36539,
#36540,#36541,#36542,#36543,#36544,#36545,#36546,#36547,#36548,#36549,#36550,
#36551,#36552,#36553,#36554,#36555,#36556,#36557,#36558,#36559,#36560,#36561,
#36562,#36563,#36564,#36565,#36566,#36567,#36568,#36569,#36570,#36571,#36572,
#36573,#36574,#36575,#36576,#36577,#36578,#36579,#36580,#36581,#36582,#36583,
#36584,#36585,#36586,#36587,#36588,#36589,#36590,#36591,#36592,#36593,#36594,
#36595,#36596,#36597,#36598,#36599,#36600,#36601,#36602,#36603,#36604,#36605,
#36606,#36607,#36608,#36609,#36610,#36611,#36612,#36613,#36614,#36615,#36616,
#36617,#36618,#36619,#36620,#36621,#36622,#36623,#36624,#36625,#36626,#36627,
#36628,#36629,#36630,#36631,#36632,#36633,#36634,#36635,#36636,#36637,#36638,
#36639,#36640,#36641,#36642,#36643,#36644,#36645,#36646,#36647,#36648,#36649,
#36650),(#36651,#36652,#36653,#36654,#36655,#36656,#36657,#36658,#36659,
#36660,#36661,#36662,#36663,#36664,#36665,#36666,#36667,#36668,#36669,#36670,
#36671,#36672,#36673,#36674,#36675,#36676,#36677,#36678,#36679,#36680,#36681,
#36682,#36683,#36684,#36685,#36686,#36687,#36688,#36689,#36690,#36691,#36692,
#36693,#36694,#36695,#36696,#36697,#36698,#36699,#36700,#36701,#36702,#36703,
#36704,#36705,#36706,#36707,#36708,#36709,#36710,#36711,#36712,#36713,#36714,
#36715,#36716,#36717,#36718,#36719,#36720,#36721,#36722,#36723,#36724,#36725,
#36726,#36727,#36728,#36729,#36730,#36731,#36732,#36733,#36734,#36735,#36736,
#36737,#36738,#36739,#36740,#36741,#36742,#36743,#36744,#36745,#36746,#36747,
#36748,#36749,#36750,#36751,#36752,#36753,#36754,#36755,#36756,#36757,#36758,
#36759,#36760,#36761,#36762,#36763,#36764,#36765)),.UNSPECIFIED.,.F.,.F.,
 .F.,(4,4),(4,1,1,1,1,1,1,1,1,1,1,1,1,1,1,1,1,1,1,1,1,1,1,1,1,1,1,1,1,1,
1,1,1,1,1,1,1,1,1,1,1,1,1,1,1,1,1,1,1,1,1,1,1,1,1,1,1,1,1,1,1,1,1,1,1,1,
1,1,1,1,1,1,1,1,1,1,1,1,1,1,1,1,1,1,1,1,1,1,1,1,1,1,1,1,1,1,1,1,1,1,1,1,
1,1,1,1,1,1,1,1,1,1,4),(0.,0.173020531651036),(12.1475814751569,12.6421543672732,
13.1367272593894,13.6313001515056,14.1258730436219,14.6204459357381,15.1150188278544,
15.6095917199706,16.1041646120869,16.5987375042031,17.0933103963194,17.5878832884356,
18.0824561805519,18.5770290726681,19.0716019647843,19.5661748569006,20.0607477490168,
20.5553206411331,21.0498935332493,21.5444664253656,22.0390393174818,22.5336122095981,
23.0281851017143,23.5227579938306,24.0173308859468,24.511903778063,25.0064766701793,
25.5010495622955,25.9956224544118,26.490195346528,26.9847682386443,27.4793411307605,
27.9739140228768,28.468486914993,28.9630598071093,29.4576326992255,29.9522055913417,
30.446778483458,30.9413513755742,31.4359242676905,31.9304971598067,32.425070051923,
32.9196429440392,33.4142158361555,33.9087887282717,34.403361620388,34.8979345125042,
35.3925074046204,35.8870802967367,36.3816531888529,36.8762260809692,37.3707989730854,
37.8653718652017,38.3599447573179,38.8545176494342,39.3490905415504,39.8436634336667,
40.3382363257829,40.8328092178991,41.3273821100154,41.8219550021316,42.3165278942479,
42.8111007863641,43.3056736784804,43.8002465705966,44.2948194627129,44.7893923548291,
45.2839652469454,45.7785381390616,46.2731110311778,46.7676839232941,47.2622568154103,
47.7568297075266,48.2514025996428,48.7459754917591,49.2405483838753,49.7351212759916,
50.2296941681078,50.7242670602241,51.2188399523403,51.7134128444565,52.2079857365728,
52.702558628689,53.1971315208053,53.6917044129215,54.1862773050378,54.680850197154,
55.1754230892703,55.6699959813865,56.1645688735028,56.659141765619,57.1537146577353,
57.6482875498515,58.1428604419677,58.637433334084,59.1320062262002,59.6265791183165,
60.1211520104327,60.615724902549,61.1102977946652,61.6048706867815,62.0994435788977,
62.5940164710139,63.0885893631302,63.5831622552464,64.0777351473627,64.5723080394789,
65.0668809315952,65.5614538237114,66.0560267158277,66.5505996079439,67.0451725000601,
67.5397453921764),.UNSPECIFIED.);
#12=B_SPLINE_SURFACE_WITH_KNOTS('',3,3,((#36865,#36866,#36867,#36868,#36869,
#36870,#36871,#36872,#36873,#36874,#36875,#36876,#36877,#36878,#36879,#36880,
#36881,#36882,#36883,#36884,#36885,#36886,#36887,#36888,#36889,#36890,#36891,
#36892,#36893,#36894,#36895,#36896,#36897,#36898,#36899,#36900,#36901,#36902,
#36903,#36904,#36905,#36906,#36907,#36908,#36909,#36910,#36911,#36912,#36913,
#36914,#36915,#36916,#36917,#36918,#36919,#36920,#36921,#36922,#36923,#36924,
#36925,#36926,#36927,#36928,#36929,#36930,#36931,#36932,#36933,#36934,#36935,
#36936,#36937,#36938,#36939,#36940,#36941,#36942,#36943,#36944,#36945,#36946,
#36947,#36948,#36949,#36950,#36951,#36952,#36953,#36954,#36955,#36956,#36957,
#36958,#36959,#36960,#36961,#36962,#36963,#36964,#36965,#36966,#36967,#36968,
#36969,#36970,#36971,#36972,#36973,#36974,#36975,#36976,#36977,#36978,#36979),
(#36980,#36981,#36982,#36983,#36984,#36985,#36986,#36987,#36988,#36989,
#36990,#36991,#36992,#36993,#36994,#36995,#36996,#36997,#36998,#36999,#37000,
#37001,#37002,#37003,#37004,#37005,#37006,#37007,#37008,#37009,#37010,#37011,
#37012,#37013,#37014,#37015,#37016,#37017,#37018,#37019,#37020,#37021,#37022,
#37023,#37024,#37025,#37026,#37027,#37028,#37029,#37030,#37031,#37032,#37033,
#37034,#37035,#37036,#37037,#37038,#37039,#37040,#37041,#37042,#37043,#37044,
#37045,#37046,#37047,#37048,#37049,#37050,#37051,#37052,#37053,#37054,#37055,
#37056,#37057,#37058,#37059,#37060,#37061,#37062,#37063,#37064,#37065,#37066,
#37067,#37068,#37069,#37070,#37071,#37072,#37073,#37074,#37075,#37076,#37077,
#37078,#37079,#37080,#37081,#37082,#37083,#37084,#37085,#37086,#37087,#37088,
#37089,#37090,#37091,#37092,#37093,#37094),(#37095,#37096,#37097,#37098,
#37099,#37100,#37101,#37102,#37103,#37104,#37105,#37106,#37107,#37108,#37109,
#37110,#37111,#37112,#37113,#37114,#37115,#37116,#37117,#37118,#37119,#37120,
#37121,#37122,#37123,#37124,#37125,#37126,#37127,#37128,#37129,#37130,#37131,
#37132,#37133,#37134,#37135,#37136,#37137,#37138,#37139,#37140,#37141,#37142,
#37143,#37144,#37145,#37146,#37147,#37148,#37149,#37150,#37151,#37152,#37153,
#37154,#37155,#37156,#37157,#37158,#37159,#37160,#37161,#37162,#37163,#37164,
#37165,#37166,#37167,#37168,#37169,#37170,#37171,#37172,#37173,#37174,#37175,
#37176,#37177,#37178,#37179,#37180,#37181,#37182,#37183,#37184,#37185,#37186,
#37187,#37188,#37189,#37190,#37191,#37192,#37193,#37194,#37195,#37196,#37197,
#37198,#37199,#37200,#37201,#37202,#37203,#37204,#37205,#37206,#37207,#37208,
#37209),(#37210,#37211,#37212,#37213,#37214,#37215,#37216,#37217,#37218,
#37219,#37220,#37221,#37222,#37223,#37224,#37225,#37226,#37227,#37228,#37229,
#37230,#37231,#37232,#37233,#37234,#37235,#37236,#37237,#37238,#37239,#37240,
#37241,#37242,#37243,#37244,#37245,#37246,#37247,#37248,#37249,#37250,#37251,
#37252,#37253,#37254,#37255,#37256,#37257,#37258,#37259,#37260,#37261,#37262,
#37263,#37264,#37265,#37266,#37267,#37268,#37269,#37270,#37271,#37272,#37273,
#37274,#37275,#37276,#37277,#37278,#37279,#37280,#37281,#37282,#37283,#37284,
#37285,#37286,#37287,#37288,#37289,#37290,#37291,#37292,#37293,#37294,#37295,
#37296,#37297,#37298,#37299,#37300,#37301,#37302,#37303,#37304,#37305,#37306,
#37307,#37308,#37309,#37310,#37311,#37312,#37313,#37314,#37315,#37316,#37317,
#37318,#37319,#37320,#37321,#37322,#37323,#37324)),.UNSPECIFIED.,.F.,.F.,
 .F.,(4,4),(4,1,1,1,1,1,1,1,1,1,1,1,1,1,1,1,1,1,1,1,1,1,1,1,1,1,1,1,1,1,
1,1,1,1,1,1,1,1,1,1,1,1,1,1,1,1,1,1,1,1,1,1,1,1,1,1,1,1,1,1,1,1,1,1,1,1,
1,1,1,1,1,1,1,1,1,1,1,1,1,1,1,1,1,1,1,1,1,1,1,1,1,1,1,1,1,1,1,1,1,1,1,1,
1,1,1,1,1,1,1,1,1,1,4),(0.,0.173020531651036),(15.1888611523549,15.6834340444711,
16.1780069365874,16.6725798287036,17.1671527208199,17.6617256129361,18.1562985050523,
18.6508713971686,19.1454442892848,19.6400171814011,20.1345900735173,20.6291629656336,
21.1237358577498,21.6183087498661,22.1128816419823,22.6074545340986,23.1020274262148,
23.596600318331,24.0911732104473,24.5857461025635,25.0803189946798,25.574891886796,
26.0694647789123,26.5640376710285,27.0586105631448,27.553183455261,28.0477563473773,
28.5423292394935,29.0369021316097,29.531475023726,30.0260479158422,30.5206208079585,
31.0151937000747,31.509766592191,32.0043394843072,32.4989123764235,32.9934852685397,
33.488058160656,33.9826310527722,34.4772039448884,34.9717768370047,35.4663497291209,
35.9609226212372,36.4554955133534,36.9500684054697,37.4446412975859,37.9392141897022,
38.4337870818184,38.9283599739347,39.4229328660509,39.9175057581671,40.4120786502834,
40.9066515423996,41.4012244345159,41.8957973266321,42.3903702187484,42.8849431108646,
43.3795160029809,43.8740888950971,44.3686617872134,44.8632346793296,45.3578075714458,
45.8523804635621,46.3469533556783,46.8415262477946,47.3360991399108,47.8306720320271,
48.3252449241433,48.8198178162596,49.3143907083758,49.8089636004921,50.3035364926083,
50.7981093847245,51.2926822768408,51.787255168957,52.2818280610733,52.7764009531895,
53.2709738453058,53.765546737422,54.2601196295383,54.7546925216545,55.2492654137708,
55.743838305887,56.2384111980032,56.7329840901195,57.2275569822357,57.722129874352,
58.2167027664682,58.7112756585845,59.2058485507007,59.700421442817,60.1949943349332,
60.6895672270495,61.1841401191657,61.6787130112819,62.1732859033982,62.6678587955144,
63.1624316876307,63.6570045797469,64.1515774718632,64.6461503639794,65.1407232560957,
65.6352961482119,66.1298690403281,66.6244419324444,67.1190148245607,67.6135877166769,
68.1081606087931,68.6027335009094,69.0973063930256,69.5918792851419,70.0864521772581,
70.5810250693744),.UNSPECIFIED.);
#13=B_SPLINE_SURFACE_WITH_KNOTS('',3,3,((#43107,#43108,#43109,#43110,#43111,
#43112,#43113,#43114,#43115,#43116,#43117,#43118,#43119,#43120,#43121,#43122,
#43123,#43124,#43125,#43126,#43127,#43128,#43129,#43130,#43131,#43132,#43133,
#43134,#43135,#43136,#43137,#43138,#43139,#43140,#43141,#43142,#43143,#43144,
#43145,#43146,#43147,#43148,#43149,#43150,#43151,#43152,#43153,#43154,#43155,
#43156,#43157,#43158,#43159,#43160,#43161,#43162,#43163,#43164,#43165,#43166,
#43167,#43168,#43169,#43170,#43171,#43172,#43173,#43174,#43175,#43176,#43177,
#43178,#43179,#43180,#43181,#43182,#43183,#43184,#43185,#43186,#43187,#43188,
#43189,#43190,#43191,#43192,#43193,#43194,#43195,#43196,#43197,#43198,#43199,
#43200,#43201,#43202,#43203,#43204,#43205,#43206,#43207,#43208,#43209,#43210,
#43211,#43212,#43213,#43214,#43215,#43216,#43217,#43218,#43219,#43220,#43221,
#43222,#43223,#43224,#43225,#43226,#43227,#43228,#43229,#43230,#43231,#43232,
#43233,#43234,#43235,#43236,#43237,#43238,#43239,#43240,#43241,#43242,#43243,
#43244,#43245,#43246,#43247,#43248,#43249,#43250,#43251,#43252,#43253,#43254,
#43255,#43256,#43257,#43258,#43259,#43260,#43261,#43262,#43263,#43264,#43265,
#43266,#43267,#43268,#43269,#43270,#43271,#43272,#43273,#43274,#43275,#43276,
#43277,#43278,#43279,#43280,#43281,#43282,#43283,#43284,#43285,#43286,#43287,
#43288,#43289,#43290,#43291,#43292,#43293,#43294,#43295,#43296,#43297,#43298,
#43299,#43300,#43301,#43302,#43303,#43304,#43305,#43306,#43307,#43308,#43309,
#43310,#43311,#43312,#43313,#43314,#43315,#43316,#43317,#43318,#43319,#43320,
#43321,#43322,#43323,#43324,#43325,#43326,#43327,#43328,#43329,#43330,#43331,
#43332,#43333,#43334,#43335,#43336,#43337,#43338,#43339,#43340,#43341,#43342,
#43343,#43344,#43345,#43346,#43347,#43348,#43349,#43350,#43351,#43352,#43353,
#43354,#43355,#43356,#43357,#43358,#43359,#43360,#43361,#43362,#43363,#43364,
#43365,#43366,#43367,#43368,#43369,#43370,#43371,#43372,#43373,#43374,#43375,
#43376,#43377,#43378,#43379,#43380,#43381,#43382,#43383,#43384,#43385,#43386,
#43387,#43388,#43389,#43390,#43391,#43392,#43393,#43394,#43395,#43396,#43397,
#43398,#43399,#43400,#43401,#43402,#43403,#43404,#43405,#43406,#43407,#43408,
#43409,#43410,#43411,#43412,#43413,#43414,#43415,#43416,#43417,#43418,#43419,
#43420,#43421,#43422,#43423,#43424,#43425,#43426,#43427,#43428,#43429,#43430,
#43431,#43432,#43433,#43434,#43435,#43436,#43437,#43438,#43439,#43440,#43441,
#43442,#43443,#43444,#43445,#43446,#43447,#43448,#43449,#43450,#43451,#43452,
#43453,#43454,#43455,#43456,#43457,#43458,#43459,#43460,#43461,#43462,#43463,
#43464,#43465,#43466,#43467,#43468,#43469,#43470,#43471,#43472,#43473,#43474,
#43475,#43476,#43477,#43478,#43479,#43480,#43481,#43482,#43483,#43484,#43485,
#43486,#43487,#43488,#43489,#43490,#43491,#43492,#43493,#43494,#43495,#43496,
#43497,#43498,#43499,#43500,#43501,#43502,#43503,#43504,#43505,#43506,#43507,
#43508,#43509,#43510,#43511,#43512,#43513,#43514,#43515,#43516,#43517,#43518,
#43519,#43520,#43521,#43522,#43523,#43524,#43525,#43526,#43527,#43528,#43529,
#43530,#43531,#43532,#43533,#43534,#43535,#43536,#43537,#43538,#43539,#43540,
#43541,#43542,#43543,#43544,#43545,#43546,#43547,#43548,#43549,#43550,#43551,
#43552,#43553,#43554,#43555,#43556,#43557,#43558,#43559,#43560,#43561,#43562,
#43563,#43564,#43565,#43566,#43567,#43568,#43569,#43570,#43571,#43572,#43573,
#43574,#43575,#43576,#43577,#43578,#43579,#43580,#43581,#43582,#43583,#43584,
#43585,#43586,#43587,#43588,#43589,#43590,#43591,#43592,#43593,#43594,#43595,
#43596,#43597,#43598,#43599,#43600,#43601,#43602,#43603,#43604),(#43605,
#43606,#43607,#43608,#43609,#43610,#43611,#43612,#43613,#43614,#43615,#43616,
#43617,#43618,#43619,#43620,#43621,#43622,#43623,#43624,#43625,#43626,#43627,
#43628,#43629,#43630,#43631,#43632,#43633,#43634,#43635,#43636,#43637,#43638,
#43639,#43640,#43641,#43642,#43643,#43644,#43645,#43646,#43647,#43648,#43649,
#43650,#43651,#43652,#43653,#43654,#43655,#43656,#43657,#43658,#43659,#43660,
#43661,#43662,#43663,#43664,#43665,#43666,#43667,#43668,#43669,#43670,#43671,
#43672,#43673,#43674,#43675,#43676,#43677,#43678,#43679,#43680,#43681,#43682,
#43683,#43684,#43685,#43686,#43687,#43688,#43689,#43690,#43691,#43692,#43693,
#43694,#43695,#43696,#43697,#43698,#43699,#43700,#43701,#43702,#43703,#43704,
#43705,#43706,#43707,#43708,#43709,#43710,#43711,#43712,#43713,#43714,#43715,
#43716,#43717,#43718,#43719,#43720,#43721,#43722,#43723,#43724,#43725,#43726,
#43727,#43728,#43729,#43730,#43731,#43732,#43733,#43734,#43735,#43736,#43737,
#43738,#43739,#43740,#43741,#43742,#43743,#43744,#43745,#43746,#43747,#43748,
#43749,#43750,#43751,#43752,#43753,#43754,#43755,#43756,#43757,#43758,#43759,
#43760,#43761,#43762,#43763,#43764,#43765,#43766,#43767,#43768,#43769,#43770,
#43771,#43772,#43773,#43774,#43775,#43776,#43777,#43778,#43779,#43780,#43781,
#43782,#43783,#43784,#43785,#43786,#43787,#43788,#43789,#43790,#43791,#43792,
#43793,#43794,#43795,#43796,#43797,#43798,#43799,#43800,#43801,#43802,#43803,
#43804,#43805,#43806,#43807,#43808,#43809,#43810,#43811,#43812,#43813,#43814,
#43815,#43816,#43817,#43818,#43819,#43820,#43821,#43822,#43823,#43824,#43825,
#43826,#43827,#43828,#43829,#43830,#43831,#43832,#43833,#43834,#43835,#43836,
#43837,#43838,#43839,#43840,#43841,#43842,#43843,#43844,#43845,#43846,#43847,
#43848,#43849,#43850,#43851,#43852,#43853,#43854,#43855,#43856,#43857,#43858,
#43859,#43860,#43861,#43862,#43863,#43864,#43865,#43866,#43867,#43868,#43869,
#43870,#43871,#43872,#43873,#43874,#43875,#43876,#43877,#43878,#43879,#43880,
#43881,#43882,#43883,#43884,#43885,#43886,#43887,#43888,#43889,#43890,#43891,
#43892,#43893,#43894,#43895,#43896,#43897,#43898,#43899,#43900,#43901,#43902,
#43903,#43904,#43905,#43906,#43907,#43908,#43909,#43910,#43911,#43912,#43913,
#43914,#43915,#43916,#43917,#43918,#43919,#43920,#43921,#43922,#43923,#43924,
#43925,#43926,#43927,#43928,#43929,#43930,#43931,#43932,#43933,#43934,#43935,
#43936,#43937,#43938,#43939,#43940,#43941,#43942,#43943,#43944,#43945,#43946,
#43947,#43948,#43949,#43950,#43951,#43952,#43953,#43954,#43955,#43956,#43957,
#43958,#43959,#43960,#43961,#43962,#43963,#43964,#43965,#43966,#43967,#43968,
#43969,#43970,#43971,#43972,#43973,#43974,#43975,#43976,#43977,#43978,#43979,
#43980,#43981,#43982,#43983,#43984,#43985,#43986,#43987,#43988,#43989,#43990,
#43991,#43992,#43993,#43994,#43995,#43996,#43997,#43998,#43999,#44000,#44001,
#44002,#44003,#44004,#44005,#44006,#44007,#44008,#44009,#44010,#44011,#44012,
#44013,#44014,#44015,#44016,#44017,#44018,#44019,#44020,#44021,#44022,#44023,
#44024,#44025,#44026,#44027,#44028,#44029,#44030,#44031,#44032,#44033,#44034,
#44035,#44036,#44037,#44038,#44039,#44040,#44041,#44042,#44043,#44044,#44045,
#44046,#44047,#44048,#44049,#44050,#44051,#44052,#44053,#44054,#44055,#44056,
#44057,#44058,#44059,#44060,#44061,#44062,#44063,#44064,#44065,#44066,#44067,
#44068,#44069,#44070,#44071,#44072,#44073,#44074,#44075,#44076,#44077,#44078,
#44079,#44080,#44081,#44082,#44083,#44084,#44085,#44086,#44087,#44088,#44089,
#44090,#44091,#44092,#44093,#44094,#44095,#44096,#44097,#44098,#44099,#44100,
#44101,#44102),(#44103,#44104,#44105,#44106,#44107,#44108,#44109,#44110,
#44111,#44112,#44113,#44114,#44115,#44116,#44117,#44118,#44119,#44120,#44121,
#44122,#44123,#44124,#44125,#44126,#44127,#44128,#44129,#44130,#44131,#44132,
#44133,#44134,#44135,#44136,#44137,#44138,#44139,#44140,#44141,#44142,#44143,
#44144,#44145,#44146,#44147,#44148,#44149,#44150,#44151,#44152,#44153,#44154,
#44155,#44156,#44157,#44158,#44159,#44160,#44161,#44162,#44163,#44164,#44165,
#44166,#44167,#44168,#44169,#44170,#44171,#44172,#44173,#44174,#44175,#44176,
#44177,#44178,#44179,#44180,#44181,#44182,#44183,#44184,#44185,#44186,#44187,
#44188,#44189,#44190,#44191,#44192,#44193,#44194,#44195,#44196,#44197,#44198,
#44199,#44200,#44201,#44202,#44203,#44204,#44205,#44206,#44207,#44208,#44209,
#44210,#44211,#44212,#44213,#44214,#44215,#44216,#44217,#44218,#44219,#44220,
#44221,#44222,#44223,#44224,#44225,#44226,#44227,#44228,#44229,#44230,#44231,
#44232,#44233,#44234,#44235,#44236,#44237,#44238,#44239,#44240,#44241,#44242,
#44243,#44244,#44245,#44246,#44247,#44248,#44249,#44250,#44251,#44252,#44253,
#44254,#44255,#44256,#44257,#44258,#44259,#44260,#44261,#44262,#44263,#44264,
#44265,#44266,#44267,#44268,#44269,#44270,#44271,#44272,#44273,#44274,#44275,
#44276,#44277,#44278,#44279,#44280,#44281,#44282,#44283,#44284,#44285,#44286,
#44287,#44288,#44289,#44290,#44291,#44292,#44293,#44294,#44295,#44296,#44297,
#44298,#44299,#44300,#44301,#44302,#44303,#44304,#44305,#44306,#44307,#44308,
#44309,#44310,#44311,#44312,#44313,#44314,#44315,#44316,#44317,#44318,#44319,
#44320,#44321,#44322,#44323,#44324,#44325,#44326,#44327,#44328,#44329,#44330,
#44331,#44332,#44333,#44334,#44335,#44336,#44337,#44338,#44339,#44340,#44341,
#44342,#44343,#44344,#44345,#44346,#44347,#44348,#44349,#44350,#44351,#44352,
#44353,#44354,#44355,#44356,#44357,#44358,#44359,#44360,#44361,#44362,#44363,
#44364,#44365,#44366,#44367,#44368,#44369,#44370,#44371,#44372,#44373,#44374,
#44375,#44376,#44377,#44378,#44379,#44380,#44381,#44382,#44383,#44384,#44385,
#44386,#44387,#44388,#44389,#44390,#44391,#44392,#44393,#44394,#44395,#44396,
#44397,#44398,#44399,#44400,#44401,#44402,#44403,#44404,#44405,#44406,#44407,
#44408,#44409,#44410,#44411,#44412,#44413,#44414,#44415,#44416,#44417,#44418,
#44419,#44420,#44421,#44422,#44423,#44424,#44425,#44426,#44427,#44428,#44429,
#44430,#44431,#44432,#44433,#44434,#44435,#44436,#44437,#44438,#44439,#44440,
#44441,#44442,#44443,#44444,#44445,#44446,#44447,#44448,#44449,#44450,#44451,
#44452,#44453,#44454,#44455,#44456,#44457,#44458,#44459,#44460,#44461,#44462,
#44463,#44464,#44465,#44466,#44467,#44468,#44469,#44470,#44471,#44472,#44473,
#44474,#44475,#44476,#44477,#44478,#44479,#44480,#44481,#44482,#44483,#44484,
#44485,#44486,#44487,#44488,#44489,#44490,#44491,#44492,#44493,#44494,#44495,
#44496,#44497,#44498,#44499,#44500,#44501,#44502,#44503,#44504,#44505,#44506,
#44507,#44508,#44509,#44510,#44511,#44512,#44513,#44514,#44515,#44516,#44517,
#44518,#44519,#44520,#44521,#44522,#44523,#44524,#44525,#44526,#44527,#44528,
#44529,#44530,#44531,#44532,#44533,#44534,#44535,#44536,#44537,#44538,#44539,
#44540,#44541,#44542,#44543,#44544,#44545,#44546,#44547,#44548,#44549,#44550,
#44551,#44552,#44553,#44554,#44555,#44556,#44557,#44558,#44559,#44560,#44561,
#44562,#44563,#44564,#44565,#44566,#44567,#44568,#44569,#44570,#44571,#44572,
#44573,#44574,#44575,#44576,#44577,#44578,#44579,#44580,#44581,#44582,#44583,
#44584,#44585,#44586,#44587,#44588,#44589,#44590,#44591,#44592,#44593,#44594,
#44595,#44596,#44597,#44598,#44599,#44600),(#44601,#44602,#44603,#44604,
#44605,#44606,#44607,#44608,#44609,#44610,#44611,#44612,#44613,#44614,#44615,
#44616,#44617,#44618,#44619,#44620,#44621,#44622,#44623,#44624,#44625,#44626,
#44627,#44628,#44629,#44630,#44631,#44632,#44633,#44634,#44635,#44636,#44637,
#44638,#44639,#44640,#44641,#44642,#44643,#44644,#44645,#44646,#44647,#44648,
#44649,#44650,#44651,#44652,#44653,#44654,#44655,#44656,#44657,#44658,#44659,
#44660,#44661,#44662,#44663,#44664,#44665,#44666,#44667,#44668,#44669,#44670,
#44671,#44672,#44673,#44674,#44675,#44676,#44677,#44678,#44679,#44680,#44681,
#44682,#44683,#44684,#44685,#44686,#44687,#44688,#44689,#44690,#44691,#44692,
#44693,#44694,#44695,#44696,#44697,#44698,#44699,#44700,#44701,#44702,#44703,
#44704,#44705,#44706,#44707,#44708,#44709,#44710,#44711,#44712,#44713,#44714,
#44715,#44716,#44717,#44718,#44719,#44720,#44721,#44722,#44723,#44724,#44725,
#44726,#44727,#44728,#44729,#44730,#44731,#44732,#44733,#44734,#44735,#44736,
#44737,#44738,#44739,#44740,#44741,#44742,#44743,#44744,#44745,#44746,#44747,
#44748,#44749,#44750,#44751,#44752,#44753,#44754,#44755,#44756,#44757,#44758,
#44759,#44760,#44761,#44762,#44763,#44764,#44765,#44766,#44767,#44768,#44769,
#44770,#44771,#44772,#44773,#44774,#44775,#44776,#44777,#44778,#44779,#44780,
#44781,#44782,#44783,#44784,#44785,#44786,#44787,#44788,#44789,#44790,#44791,
#44792,#44793,#44794,#44795,#44796,#44797,#44798,#44799,#44800,#44801,#44802,
#44803,#44804,#44805,#44806,#44807,#44808,#44809,#44810,#44811,#44812,#44813,
#44814,#44815,#44816,#44817,#44818,#44819,#44820,#44821,#44822,#44823,#44824,
#44825,#44826,#44827,#44828,#44829,#44830,#44831,#44832,#44833,#44834,#44835,
#44836,#44837,#44838,#44839,#44840,#44841,#44842,#44843,#44844,#44845,#44846,
#44847,#44848,#44849,#44850,#44851,#44852,#44853,#44854,#44855,#44856,#44857,
#44858,#44859,#44860,#44861,#44862,#44863,#44864,#44865,#44866,#44867,#44868,
#44869,#44870,#44871,#44872,#44873,#44874,#44875,#44876,#44877,#44878,#44879,
#44880,#44881,#44882,#44883,#44884,#44885,#44886,#44887,#44888,#44889,#44890,
#44891,#44892,#44893,#44894,#44895,#44896,#44897,#44898,#44899,#44900,#44901,
#44902,#44903,#44904,#44905,#44906,#44907,#44908,#44909,#44910,#44911,#44912,
#44913,#44914,#44915,#44916,#44917,#44918,#44919,#44920,#44921,#44922,#44923,
#44924,#44925,#44926,#44927,#44928,#44929,#44930,#44931,#44932,#44933,#44934,
#44935,#44936,#44937,#44938,#44939,#44940,#44941,#44942,#44943,#44944,#44945,
#44946,#44947,#44948,#44949,#44950,#44951,#44952,#44953,#44954,#44955,#44956,
#44957,#44958,#44959,#44960,#44961,#44962,#44963,#44964,#44965,#44966,#44967,
#44968,#44969,#44970,#44971,#44972,#44973,#44974,#44975,#44976,#44977,#44978,
#44979,#44980,#44981,#44982,#44983,#44984,#44985,#44986,#44987,#44988,#44989,
#44990,#44991,#44992,#44993,#44994,#44995,#44996,#44997,#44998,#44999,#45000,
#45001,#45002,#45003,#45004,#45005,#45006,#45007,#45008,#45009,#45010,#45011,
#45012,#45013,#45014,#45015,#45016,#45017,#45018,#45019,#45020,#45021,#45022,
#45023,#45024,#45025,#45026,#45027,#45028,#45029,#45030,#45031,#45032,#45033,
#45034,#45035,#45036,#45037,#45038,#45039,#45040,#45041,#45042,#45043,#45044,
#45045,#45046,#45047,#45048,#45049,#45050,#45051,#45052,#45053,#45054,#45055,
#45056,#45057,#45058,#45059,#45060,#45061,#45062,#45063,#45064,#45065,#45066,
#45067,#45068,#45069,#45070,#45071,#45072,#45073,#45074,#45075,#45076,#45077,
#45078,#45079,#45080,#45081,#45082,#45083,#45084,#45085,#45086,#45087,#45088,
#45089,#45090,#45091,#45092,#45093,#45094,#45095,#45096,#45097,#45098)),
 .UNSPECIFIED.,.F.,.F.,.F.,(4,4),(4,1,1,1,1,1,1,1,1,1,1,1,1,1,1,1,1,1,1,
1,1,1,1,1,1,1,1,1,1,1,1,1,1,1,1,1,1,1,1,1,1,1,1,1,1,1,1,1,1,1,1,1,1,1,1,
1,1,1,1,1,1,1,1,1,1,1,1,1,1,1,1,1,1,1,1,1,1,1,1,1,1,1,1,1,1,1,1,1,1,1,1,
1,1,1,1,1,1,1,1,1,1,1,1,1,1,1,1,1,1,1,1,1,1,1,1,1,1,1,1,1,1,1,1,1,1,1,1,
1,1,1,1,1,1,1,1,1,1,1,1,1,1,1,1,1,1,1,1,1,1,1,1,1,1,1,1,1,1,1,1,1,1,1,1,
1,1,1,1,1,1,1,1,1,1,1,1,1,1,1,1,1,1,1,1,1,1,1,1,1,1,1,1,1,1,1,1,1,1,1,1,
1,1,1,1,1,1,1,1,1,1,1,1,1,1,1,1,1,1,1,1,1,1,1,1,1,1,1,1,1,1,1,1,1,1,1,1,
1,1,1,1,1,1,1,1,1,1,1,1,1,1,1,1,1,1,1,1,1,1,1,1,1,1,1,1,1,1,1,1,1,1,1,1,
1,1,1,1,1,1,1,1,1,1,1,1,1,1,1,1,1,1,1,1,1,1,1,1,1,1,1,1,1,1,1,1,1,1,1,1,
1,1,1,1,1,1,1,1,1,1,1,1,1,1,1,1,1,1,1,1,1,1,1,1,1,1,1,1,1,1,1,1,1,1,1,1,
1,1,1,1,1,1,1,1,1,1,1,1,1,1,1,1,1,1,1,1,1,1,1,1,1,1,1,1,1,1,1,1,1,1,1,1,
1,1,1,1,1,1,1,1,1,1,1,1,1,1,1,1,1,1,1,1,1,1,1,1,1,1,1,1,1,1,1,1,1,1,1,1,
1,1,1,1,1,1,1,1,1,1,1,1,1,1,1,1,1,1,1,1,1,1,1,1,1,1,1,1,1,1,1,1,1,1,1,1,
1,1,1,1,1,1,1,1,1,1,1,1,1,1,1,1,1,1,1,1,1,1,1,1,1,1,1,1,1,1,1,1,1,1,1,1,
1,1,1,1,1,1,1,1,4),(0.,0.184512097253587),(8.98171729021681,9.48139635699984,
9.98107542378286,10.4807544905659,10.9804335573489,11.4801126241319,11.979791690915,
12.479470757698,12.979149824481,13.478828891264,13.9785079580471,14.4781870248301,
14.9778660916131,15.4775451583961,15.9772242251791,16.4769032919622,16.9765823587452,
17.4762614255282,17.9759404923112,18.4756195590943,18.9752986258773,19.4749776926603,
19.9746567594433,20.4743358262264,20.9740148930094,21.4736939597924,21.9733730265754,
22.4730520933585,22.9727311601415,23.4724102269245,23.9720892937075,24.4717683604905,
24.9714474272736,25.4711264940566,25.9708055608396,26.4704846276226,26.9701636944057,
27.4698427611887,27.9695218279717,28.4692008947547,28.9688799615378,29.4685590283208,
29.9682380951038,30.4679171618868,30.9675962286699,31.4672752954529,31.9669543622359,
32.4666334290189,32.966312495802,33.465991562585,33.965670629368,34.465349696151,
34.965028762934,35.4647078297171,35.9643868965001,36.4640659632831,36.9637450300661,
37.4634240968492,37.9631031636322,38.4627822304152,38.9624612971982,39.4621403639813,
39.9618194307643,40.4614984975473,40.9611775643303,41.4608566311134,41.9605356978964,
42.4602147646794,42.9598938314624,43.4595728982454,43.9592519650285,44.4589310318115,
44.9586100985945,45.4582891653775,45.9579682321606,46.4576472989436,46.9573263657266,
47.4570054325096,47.9566844992927,48.4563635660757,48.9560426328587,49.4557216996417,
49.9554007664248,50.4550798332078,50.9547588999908,51.4544379667738,51.9541170335568,
52.4537961003399,52.9534751671229,53.4531542339059,53.9528333006889,54.452512367472,
54.952191434255,55.451870501038,55.951549567821,56.4512286346041,56.9509077013871,
57.4505867681701,57.9502658349531,58.4499449017362,58.9496239685192,59.9489821020852,
60.9483402356513,61.9476983692173,62.9470565027834,63.9464146363494,64.9457727699155,
65.9451309034815,66.9444890370476,67.9438471706136,68.9432053041797,69.9425634377457,
70.9419215713118,71.9412797048778,72.9406378384438,73.9399959720099,74.9393541055759,
75.938712239142,76.938070372708,77.9374285062741,78.9367866398401,79.9361447734062,
80.9355029069722,81.9348610405383,82.9342191741043,83.9335773076704,84.9329354412364,
85.9322935748025,86.9316517083685,87.9310098419346,88.9303679755006,89.9297261090666,
90.9290842426327,91.9284423761987,92.9278005097648,93.9271586433308,94.9265167768969,
95.9258749104629,96.925233044029,97.924591177595,98.9239493111611,99.9233074447271,
100.922665578293,101.922023711859,102.921381845425,103.920739978991,104.920098112557,
105.919456246123,106.918814379689,107.918172513255,108.917530646822,109.916888780388,
110.916246913954,111.91560504752,112.914963181086,113.914321314652,114.913679448218,
115.913037581784,116.91239571535,117.911753848916,118.911111982482,119.910470116048,
120.909828249614,121.90918638318,122.908544516746,123.907902650312,124.907260783878,
125.906618917444,126.90597705101,127.905335184576,128.904693318142,129.904051451709,
130.903409585275,131.902767718841,132.902125852407,133.901483985973,134.900842119539,
135.900200253105,136.899558386671,137.898916520237,138.898274653803,139.897632787369,
140.896990920935,141.896349054501,142.895707188067,143.895065321633,144.894423455199,
145.893781588765,146.893139722331,147.892497855897,148.891855989463,149.891214123029,
150.890572256596,151.889930390162,152.889288523728,153.888646657294,154.88800479086,
155.887362924426,156.886721057992,157.886079191558,158.885437325124,159.88479545869,
160.884153592256,161.883511725822,162.882869859388,163.882227992954,164.88158612652,
165.880944260086,166.880302393652,167.879660527218,168.879018660784,169.87837679435,
170.877734927916,171.877093061483,172.876451195049,173.875809328615,174.875167462181,
175.874525595747,176.873883729313,177.873241862879,178.872599996445,179.871958130011,
180.871316263577,181.870674397143,182.870032530709,183.869390664275,184.868748797841,
185.868106931407,186.867465064973,187.866823198539,188.866181332105,189.865539465671,
190.864897599237,191.864255732803,192.86361386637,193.862971999936,194.862330133502,
195.861688267068,196.861046400634,197.8604045342,198.859762667766,199.859120801332,
200.858478934898,201.857837068464,202.85719520203,203.856553335596,204.855911469162,
205.855269602728,206.854627736294,207.85398586986,208.853344003426,209.852702136992,
210.852060270558,211.851418404124,212.85077653769,213.850134671257,214.849492804823,
215.848850938389,216.848209071955,217.847567205521,218.846925339087,219.846283472653,
220.845641606219,221.844999739785,222.844357873351,223.843716006917,224.843074140483,
225.842432274049,226.841790407615,227.841148541181,228.840506674747,229.839864808313,
230.839222941879,231.838581075445,232.837939209011,233.837297342577,234.836655476144,
235.83601360971,236.835371743276,237.834729876842,238.834088010408,239.833446143974,
240.83280427754,241.832162411106,242.831520544672,243.830878678238,244.830236811804,
245.82959494537,246.828953078936,247.828311212502,248.827669346068,249.827027479634,
250.8263856132,251.825743746766,252.825101880332,253.824460013898,254.823818147464,
255.82317628103,256.822534414597,257.821892548163,258.821250681729,259.820608815295,
260.819966948861,261.819325082427,262.818683215993,263.818041349559,264.817399483125,
265.816757616691,266.816115750257,267.815473883823,268.814832017389,269.814190150955,
270.813548284521,271.812906418087,272.812264551653,273.811622685219,274.810980818785,
275.810338952351,276.809697085917,277.809055219484,278.80841335305,279.807771486616,
280.807129620182,281.806487753748,282.805845887314,283.80520402088,284.804562154446,
285.803920288012,286.803278421578,287.802636555144,288.80199468871,289.801352822276,
290.800710955842,291.800069089408,292.799427222974,293.79878535654,294.798143490106,
295.797501623672,296.796859757238,297.796217890804,298.795576024371,299.794934157937,
300.794292291503,301.793650425069,302.793008558635,303.792366692201,304.791724825767,
305.791082959333,306.790441092899,307.789799226465,308.789157360031,309.788515493597,
310.787873627163,311.787231760729,312.786589894295,313.785948027861,314.785306161427,
315.784664294993,316.784022428559,317.783380562125,318.782738695691,319.782096829258,
320.781454962824,321.78081309639,322.780171229956,323.779529363522,324.778887497088,
325.778245630654,326.77760376422,327.776961897786,328.776320031352,329.775678164918,
330.775036298484,331.77439443205,332.773752565616,333.773110699182,334.772468832748,
335.771826966314,336.77118509988,337.770543233446,338.769901367012,339.769259500578,
340.768617634145,341.767975767711,342.767333901277,343.766692034843,344.766050168409,
345.765408301975,346.764766435541,347.764124569107,348.763482702673,349.762840836239,
350.762198969805,351.761557103371,352.760915236937,353.760273370503,354.259952437286,
354.759631504069,355.259310570852,355.758989637635,356.258668704418,356.758347771201,
357.258026837984,357.757705904767,358.25738497155,358.757064038333,359.256743105116,
359.756422171899,360.256101238682,360.755780305465,361.255459372248,361.755138439031,
362.254817505815,362.754496572598,363.254175639381,363.753854706164,364.253533772947,
364.75321283973,365.252891906513,365.752570973296,366.252250040079,366.751929106862,
367.251608173645,367.751287240428,368.250966307211,368.750645373994,369.250324440777,
369.75000350756,370.249682574343,370.749361641126,371.249040707909,371.748719774692,
372.248398841475,372.748077908258,373.247756975041,373.747436041824,374.247115108607,
374.74679417539,375.246473242173,375.746152308956,376.245831375739,376.745510442522,
377.245189509305,377.744868576088,378.244547642871,378.744226709654,379.243905776437,
379.74358484322,380.243263910003,380.742942976786,381.242622043569,381.742301110352,
382.241980177135,382.741659243918,383.241338310702,383.741017377485,384.240696444268,
384.740375511051,385.240054577834,385.739733644617,386.2394127114,386.739091778183,
387.238770844966,387.738449911749,388.238128978532,388.737808045315,389.237487112098,
389.737166178881,390.236845245664,390.736524312447,391.23620337923,391.735882446013,
392.235561512796,392.735240579579,393.234919646362,393.734598713145,394.234277779928,
394.733956846711,395.233635913494,395.733314980277,396.23299404706,396.732673113843,
397.232352180626,397.732031247409,398.231710314192,398.731389380975,399.231068447758,
399.730747514541,400.230426581324,400.730105648107,401.22978471489,401.729463781673,
402.229142848456,402.728821915239,403.228500982022,403.728180048805),
 .UNSPECIFIED.);
#14=B_SPLINE_SURFACE_WITH_KNOTS('',3,3,((#45192,#45193,#45194,#45195,#45196,
#45197,#45198,#45199,#45200,#45201,#45202,#45203,#45204,#45205,#45206,#45207,
#45208,#45209,#45210,#45211,#45212,#45213,#45214,#45215,#45216,#45217,#45218,
#45219,#45220,#45221,#45222,#45223,#45224,#45225,#45226,#45227,#45228,#45229,
#45230,#45231,#45232,#45233,#45234,#45235,#45236,#45237,#45238,#45239,#45240,
#45241,#45242,#45243,#45244,#45245,#45246,#45247,#45248,#45249,#45250,#45251,
#45252,#45253,#45254,#45255,#45256,#45257,#45258,#45259,#45260,#45261,#45262,
#45263,#45264,#45265,#45266,#45267,#45268,#45269,#45270,#45271,#45272,#45273,
#45274,#45275,#45276,#45277,#45278,#45279,#45280,#45281,#45282,#45283,#45284,
#45285,#45286,#45287,#45288,#45289,#45290,#45291,#45292,#45293,#45294,#45295,
#45296,#45297,#45298,#45299,#45300,#45301,#45302,#45303,#45304,#45305,#45306,
#45307,#45308,#45309,#45310,#45311,#45312,#45313,#45314,#45315,#45316,#45317,
#45318,#45319,#45320,#45321,#45322,#45323,#45324,#45325,#45326,#45327,#45328,
#45329,#45330,#45331,#45332,#45333,#45334,#45335,#45336,#45337,#45338,#45339,
#45340,#45341,#45342,#45343,#45344,#45345,#45346,#45347,#45348,#45349,#45350,
#45351,#45352,#45353,#45354,#45355,#45356,#45357,#45358,#45359,#45360,#45361,
#45362,#45363,#45364,#45365,#45366,#45367,#45368,#45369,#45370,#45371,#45372,
#45373,#45374,#45375,#45376,#45377,#45378,#45379,#45380,#45381,#45382,#45383,
#45384,#45385,#45386,#45387,#45388,#45389,#45390,#45391,#45392,#45393,#45394,
#45395,#45396,#45397,#45398,#45399,#45400,#45401,#45402,#45403,#45404,#45405,
#45406,#45407,#45408,#45409,#45410,#45411,#45412,#45413,#45414,#45415,#45416,
#45417,#45418,#45419,#45420,#45421,#45422,#45423,#45424,#45425,#45426,#45427,
#45428,#45429,#45430,#45431,#45432,#45433,#45434,#45435,#45436,#45437,#45438,
#45439,#45440,#45441,#45442,#45443,#45444,#45445,#45446,#45447,#45448,#45449,
#45450,#45451,#45452,#45453,#45454,#45455,#45456,#45457,#45458,#45459,#45460,
#45461,#45462,#45463,#45464,#45465,#45466,#45467,#45468,#45469,#45470,#45471,
#45472,#45473,#45474,#45475,#45476,#45477,#45478,#45479,#45480,#45481,#45482,
#45483,#45484,#45485,#45486,#45487,#45488,#45489,#45490,#45491,#45492,#45493,
#45494,#45495,#45496,#45497,#45498,#45499,#45500,#45501,#45502,#45503,#45504,
#45505,#45506,#45507,#45508,#45509,#45510,#45511,#45512,#45513,#45514,#45515,
#45516,#45517,#45518,#45519,#45520,#45521,#45522,#45523,#45524,#45525,#45526,
#45527,#45528,#45529,#45530,#45531,#45532,#45533,#45534,#45535,#45536,#45537,
#45538,#45539,#45540,#45541,#45542,#45543,#45544,#45545,#45546,#45547,#45548,
#45549,#45550,#45551,#45552,#45553,#45554,#45555,#45556,#45557,#45558,#45559,
#45560,#45561,#45562,#45563,#45564,#45565,#45566,#45567,#45568,#45569,#45570,
#45571,#45572,#45573,#45574,#45575,#45576,#45577,#45578,#45579,#45580,#45581,
#45582,#45583,#45584,#45585,#45586,#45587,#45588,#45589,#45590,#45591,#45592,
#45593,#45594,#45595,#45596,#45597,#45598,#45599,#45600,#45601,#45602,#45603,
#45604,#45605,#45606,#45607,#45608,#45609,#45610,#45611,#45612,#45613,#45614,
#45615,#45616,#45617,#45618,#45619,#45620,#45621,#45622,#45623,#45624,#45625,
#45626,#45627,#45628,#45629,#45630,#45631,#45632,#45633,#45634,#45635,#45636,
#45637,#45638,#45639,#45640,#45641,#45642,#45643,#45644,#45645,#45646,#45647,
#45648,#45649,#45650,#45651,#45652,#45653,#45654,#45655,#45656,#45657,#45658,
#45659,#45660,#45661,#45662,#45663,#45664,#45665,#45666,#45667,#45668,#45669,
#45670,#45671,#45672,#45673,#45674,#45675,#45676,#45677,#45678,#45679,#45680,
#45681,#45682,#45683,#45684,#45685,#45686,#45687,#45688,#45689),(#45690,
#45691,#45692,#45693,#45694,#45695,#45696,#45697,#45698,#45699,#45700,#45701,
#45702,#45703,#45704,#45705,#45706,#45707,#45708,#45709,#45710,#45711,#45712,
#45713,#45714,#45715,#45716,#45717,#45718,#45719,#45720,#45721,#45722,#45723,
#45724,#45725,#45726,#45727,#45728,#45729,#45730,#45731,#45732,#45733,#45734,
#45735,#45736,#45737,#45738,#45739,#45740,#45741,#45742,#45743,#45744,#45745,
#45746,#45747,#45748,#45749,#45750,#45751,#45752,#45753,#45754,#45755,#45756,
#45757,#45758,#45759,#45760,#45761,#45762,#45763,#45764,#45765,#45766,#45767,
#45768,#45769,#45770,#45771,#45772,#45773,#45774,#45775,#45776,#45777,#45778,
#45779,#45780,#45781,#45782,#45783,#45784,#45785,#45786,#45787,#45788,#45789,
#45790,#45791,#45792,#45793,#45794,#45795,#45796,#45797,#45798,#45799,#45800,
#45801,#45802,#45803,#45804,#45805,#45806,#45807,#45808,#45809,#45810,#45811,
#45812,#45813,#45814,#45815,#45816,#45817,#45818,#45819,#45820,#45821,#45822,
#45823,#45824,#45825,#45826,#45827,#45828,#45829,#45830,#45831,#45832,#45833,
#45834,#45835,#45836,#45837,#45838,#45839,#45840,#45841,#45842,#45843,#45844,
#45845,#45846,#45847,#45848,#45849,#45850,#45851,#45852,#45853,#45854,#45855,
#45856,#45857,#45858,#45859,#45860,#45861,#45862,#45863,#45864,#45865,#45866,
#45867,#45868,#45869,#45870,#45871,#45872,#45873,#45874,#45875,#45876,#45877,
#45878,#45879,#45880,#45881,#45882,#45883,#45884,#45885,#45886,#45887,#45888,
#45889,#45890,#45891,#45892,#45893,#45894,#45895,#45896,#45897,#45898,#45899,
#45900,#45901,#45902,#45903,#45904,#45905,#45906,#45907,#45908,#45909,#45910,
#45911,#45912,#45913,#45914,#45915,#45916,#45917,#45918,#45919,#45920,#45921,
#45922,#45923,#45924,#45925,#45926,#45927,#45928,#45929,#45930,#45931,#45932,
#45933,#45934,#45935,#45936,#45937,#45938,#45939,#45940,#45941,#45942,#45943,
#45944,#45945,#45946,#45947,#45948,#45949,#45950,#45951,#45952,#45953,#45954,
#45955,#45956,#45957,#45958,#45959,#45960,#45961,#45962,#45963,#45964,#45965,
#45966,#45967,#45968,#45969,#45970,#45971,#45972,#45973,#45974,#45975,#45976,
#45977,#45978,#45979,#45980,#45981,#45982,#45983,#45984,#45985,#45986,#45987,
#45988,#45989,#45990,#45991,#45992,#45993,#45994,#45995,#45996,#45997,#45998,
#45999,#46000,#46001,#46002,#46003,#46004,#46005,#46006,#46007,#46008,#46009,
#46010,#46011,#46012,#46013,#46014,#46015,#46016,#46017,#46018,#46019,#46020,
#46021,#46022,#46023,#46024,#46025,#46026,#46027,#46028,#46029,#46030,#46031,
#46032,#46033,#46034,#46035,#46036,#46037,#46038,#46039,#46040,#46041,#46042,
#46043,#46044,#46045,#46046,#46047,#46048,#46049,#46050,#46051,#46052,#46053,
#46054,#46055,#46056,#46057,#46058,#46059,#46060,#46061,#46062,#46063,#46064,
#46065,#46066,#46067,#46068,#46069,#46070,#46071,#46072,#46073,#46074,#46075,
#46076,#46077,#46078,#46079,#46080,#46081,#46082,#46083,#46084,#46085,#46086,
#46087,#46088,#46089,#46090,#46091,#46092,#46093,#46094,#46095,#46096,#46097,
#46098,#46099,#46100,#46101,#46102,#46103,#46104,#46105,#46106,#46107,#46108,
#46109,#46110,#46111,#46112,#46113,#46114,#46115,#46116,#46117,#46118,#46119,
#46120,#46121,#46122,#46123,#46124,#46125,#46126,#46127,#46128,#46129,#46130,
#46131,#46132,#46133,#46134,#46135,#46136,#46137,#46138,#46139,#46140,#46141,
#46142,#46143,#46144,#46145,#46146,#46147,#46148,#46149,#46150,#46151,#46152,
#46153,#46154,#46155,#46156,#46157,#46158,#46159,#46160,#46161,#46162,#46163,
#46164,#46165,#46166,#46167,#46168,#46169,#46170,#46171,#46172,#46173,#46174,
#46175,#46176,#46177,#46178,#46179,#46180,#46181,#46182,#46183,#46184,#46185,
#46186,#46187),(#46188,#46189,#46190,#46191,#46192,#46193,#46194,#46195,
#46196,#46197,#46198,#46199,#46200,#46201,#46202,#46203,#46204,#46205,#46206,
#46207,#46208,#46209,#46210,#46211,#46212,#46213,#46214,#46215,#46216,#46217,
#46218,#46219,#46220,#46221,#46222,#46223,#46224,#46225,#46226,#46227,#46228,
#46229,#46230,#46231,#46232,#46233,#46234,#46235,#46236,#46237,#46238,#46239,
#46240,#46241,#46242,#46243,#46244,#46245,#46246,#46247,#46248,#46249,#46250,
#46251,#46252,#46253,#46254,#46255,#46256,#46257,#46258,#46259,#46260,#46261,
#46262,#46263,#46264,#46265,#46266,#46267,#46268,#46269,#46270,#46271,#46272,
#46273,#46274,#46275,#46276,#46277,#46278,#46279,#46280,#46281,#46282,#46283,
#46284,#46285,#46286,#46287,#46288,#46289,#46290,#46291,#46292,#46293,#46294,
#46295,#46296,#46297,#46298,#46299,#46300,#46301,#46302,#46303,#46304,#46305,
#46306,#46307,#46308,#46309,#46310,#46311,#46312,#46313,#46314,#46315,#46316,
#46317,#46318,#46319,#46320,#46321,#46322,#46323,#46324,#46325,#46326,#46327,
#46328,#46329,#46330,#46331,#46332,#46333,#46334,#46335,#46336,#46337,#46338,
#46339,#46340,#46341,#46342,#46343,#46344,#46345,#46346,#46347,#46348,#46349,
#46350,#46351,#46352,#46353,#46354,#46355,#46356,#46357,#46358,#46359,#46360,
#46361,#46362,#46363,#46364,#46365,#46366,#46367,#46368,#46369,#46370,#46371,
#46372,#46373,#46374,#46375,#46376,#46377,#46378,#46379,#46380,#46381,#46382,
#46383,#46384,#46385,#46386,#46387,#46388,#46389,#46390,#46391,#46392,#46393,
#46394,#46395,#46396,#46397,#46398,#46399,#46400,#46401,#46402,#46403,#46404,
#46405,#46406,#46407,#46408,#46409,#46410,#46411,#46412,#46413,#46414,#46415,
#46416,#46417,#46418,#46419,#46420,#46421,#46422,#46423,#46424,#46425,#46426,
#46427,#46428,#46429,#46430,#46431,#46432,#46433,#46434,#46435,#46436,#46437,
#46438,#46439,#46440,#46441,#46442,#46443,#46444,#46445,#46446,#46447,#46448,
#46449,#46450,#46451,#46452,#46453,#46454,#46455,#46456,#46457,#46458,#46459,
#46460,#46461,#46462,#46463,#46464,#46465,#46466,#46467,#46468,#46469,#46470,
#46471,#46472,#46473,#46474,#46475,#46476,#46477,#46478,#46479,#46480,#46481,
#46482,#46483,#46484,#46485,#46486,#46487,#46488,#46489,#46490,#46491,#46492,
#46493,#46494,#46495,#46496,#46497,#46498,#46499,#46500,#46501,#46502,#46503,
#46504,#46505,#46506,#46507,#46508,#46509,#46510,#46511,#46512,#46513,#46514,
#46515,#46516,#46517,#46518,#46519,#46520,#46521,#46522,#46523,#46524,#46525,
#46526,#46527,#46528,#46529,#46530,#46531,#46532,#46533,#46534,#46535,#46536,
#46537,#46538,#46539,#46540,#46541,#46542,#46543,#46544,#46545,#46546,#46547,
#46548,#46549,#46550,#46551,#46552,#46553,#46554,#46555,#46556,#46557,#46558,
#46559,#46560,#46561,#46562,#46563,#46564,#46565,#46566,#46567,#46568,#46569,
#46570,#46571,#46572,#46573,#46574,#46575,#46576,#46577,#46578,#46579,#46580,
#46581,#46582,#46583,#46584,#46585,#46586,#46587,#46588,#46589,#46590,#46591,
#46592,#46593,#46594,#46595,#46596,#46597,#46598,#46599,#46600,#46601,#46602,
#46603,#46604,#46605,#46606,#46607,#46608,#46609,#46610,#46611,#46612,#46613,
#46614,#46615,#46616,#46617,#46618,#46619,#46620,#46621,#46622,#46623,#46624,
#46625,#46626,#46627,#46628,#46629,#46630,#46631,#46632,#46633,#46634,#46635,
#46636,#46637,#46638,#46639,#46640,#46641,#46642,#46643,#46644,#46645,#46646,
#46647,#46648,#46649,#46650,#46651,#46652,#46653,#46654,#46655,#46656,#46657,
#46658,#46659,#46660,#46661,#46662,#46663,#46664,#46665,#46666,#46667,#46668,
#46669,#46670,#46671,#46672,#46673,#46674,#46675,#46676,#46677,#46678,#46679,
#46680,#46681,#46682,#46683,#46684,#46685),(#46686,#46687,#46688,#46689,
#46690,#46691,#46692,#46693,#46694,#46695,#46696,#46697,#46698,#46699,#46700,
#46701,#46702,#46703,#46704,#46705,#46706,#46707,#46708,#46709,#46710,#46711,
#46712,#46713,#46714,#46715,#46716,#46717,#46718,#46719,#46720,#46721,#46722,
#46723,#46724,#46725,#46726,#46727,#46728,#46729,#46730,#46731,#46732,#46733,
#46734,#46735,#46736,#46737,#46738,#46739,#46740,#46741,#46742,#46743,#46744,
#46745,#46746,#46747,#46748,#46749,#46750,#46751,#46752,#46753,#46754,#46755,
#46756,#46757,#46758,#46759,#46760,#46761,#46762,#46763,#46764,#46765,#46766,
#46767,#46768,#46769,#46770,#46771,#46772,#46773,#46774,#46775,#46776,#46777,
#46778,#46779,#46780,#46781,#46782,#46783,#46784,#46785,#46786,#46787,#46788,
#46789,#46790,#46791,#46792,#46793,#46794,#46795,#46796,#46797,#46798,#46799,
#46800,#46801,#46802,#46803,#46804,#46805,#46806,#46807,#46808,#46809,#46810,
#46811,#46812,#46813,#46814,#46815,#46816,#46817,#46818,#46819,#46820,#46821,
#46822,#46823,#46824,#46825,#46826,#46827,#46828,#46829,#46830,#46831,#46832,
#46833,#46834,#46835,#46836,#46837,#46838,#46839,#46840,#46841,#46842,#46843,
#46844,#46845,#46846,#46847,#46848,#46849,#46850,#46851,#46852,#46853,#46854,
#46855,#46856,#46857,#46858,#46859,#46860,#46861,#46862,#46863,#46864,#46865,
#46866,#46867,#46868,#46869,#46870,#46871,#46872,#46873,#46874,#46875,#46876,
#46877,#46878,#46879,#46880,#46881,#46882,#46883,#46884,#46885,#46886,#46887,
#46888,#46889,#46890,#46891,#46892,#46893,#46894,#46895,#46896,#46897,#46898,
#46899,#46900,#46901,#46902,#46903,#46904,#46905,#46906,#46907,#46908,#46909,
#46910,#46911,#46912,#46913,#46914,#46915,#46916,#46917,#46918,#46919,#46920,
#46921,#46922,#46923,#46924,#46925,#46926,#46927,#46928,#46929,#46930,#46931,
#46932,#46933,#46934,#46935,#46936,#46937,#46938,#46939,#46940,#46941,#46942,
#46943,#46944,#46945,#46946,#46947,#46948,#46949,#46950,#46951,#46952,#46953,
#46954,#46955,#46956,#46957,#46958,#46959,#46960,#46961,#46962,#46963,#46964,
#46965,#46966,#46967,#46968,#46969,#46970,#46971,#46972,#46973,#46974,#46975,
#46976,#46977,#46978,#46979,#46980,#46981,#46982,#46983,#46984,#46985,#46986,
#46987,#46988,#46989,#46990,#46991,#46992,#46993,#46994,#46995,#46996,#46997,
#46998,#46999,#47000,#47001,#47002,#47003,#47004,#47005,#47006,#47007,#47008,
#47009,#47010,#47011,#47012,#47013,#47014,#47015,#47016,#47017,#47018,#47019,
#47020,#47021,#47022,#47023,#47024,#47025,#47026,#47027,#47028,#47029,#47030,
#47031,#47032,#47033,#47034,#47035,#47036,#47037,#47038,#47039,#47040,#47041,
#47042,#47043,#47044,#47045,#47046,#47047,#47048,#47049,#47050,#47051,#47052,
#47053,#47054,#47055,#47056,#47057,#47058,#47059,#47060,#47061,#47062,#47063,
#47064,#47065,#47066,#47067,#47068,#47069,#47070,#47071,#47072,#47073,#47074,
#47075,#47076,#47077,#47078,#47079,#47080,#47081,#47082,#47083,#47084,#47085,
#47086,#47087,#47088,#47089,#47090,#47091,#47092,#47093,#47094,#47095,#47096,
#47097,#47098,#47099,#47100,#47101,#47102,#47103,#47104,#47105,#47106,#47107,
#47108,#47109,#47110,#47111,#47112,#47113,#47114,#47115,#47116,#47117,#47118,
#47119,#47120,#47121,#47122,#47123,#47124,#47125,#47126,#47127,#47128,#47129,
#47130,#47131,#47132,#47133,#47134,#47135,#47136,#47137,#47138,#47139,#47140,
#47141,#47142,#47143,#47144,#47145,#47146,#47147,#47148,#47149,#47150,#47151,
#47152,#47153,#47154,#47155,#47156,#47157,#47158,#47159,#47160,#47161,#47162,
#47163,#47164,#47165,#47166,#47167,#47168,#47169,#47170,#47171,#47172,#47173,
#47174,#47175,#47176,#47177,#47178,#47179,#47180,#47181,#47182,#47183)),
 .UNSPECIFIED.,.F.,.F.,.F.,(4,4),(4,1,1,1,1,1,1,1,1,1,1,1,1,1,1,1,1,1,1,
1,1,1,1,1,1,1,1,1,1,1,1,1,1,1,1,1,1,1,1,1,1,1,1,1,1,1,1,1,1,1,1,1,1,1,1,
1,1,1,1,1,1,1,1,1,1,1,1,1,1,1,1,1,1,1,1,1,1,1,1,1,1,1,1,1,1,1,1,1,1,1,1,
1,1,1,1,1,1,1,1,1,1,1,1,1,1,1,1,1,1,1,1,1,1,1,1,1,1,1,1,1,1,1,1,1,1,1,1,
1,1,1,1,1,1,1,1,1,1,1,1,1,1,1,1,1,1,1,1,1,1,1,1,1,1,1,1,1,1,1,1,1,1,1,1,
1,1,1,1,1,1,1,1,1,1,1,1,1,1,1,1,1,1,1,1,1,1,1,1,1,1,1,1,1,1,1,1,1,1,1,1,
1,1,1,1,1,1,1,1,1,1,1,1,1,1,1,1,1,1,1,1,1,1,1,1,1,1,1,1,1,1,1,1,1,1,1,1,
1,1,1,1,1,1,1,1,1,1,1,1,1,1,1,1,1,1,1,1,1,1,1,1,1,1,1,1,1,1,1,1,1,1,1,1,
1,1,1,1,1,1,1,1,1,1,1,1,1,1,1,1,1,1,1,1,1,1,1,1,1,1,1,1,1,1,1,1,1,1,1,1,
1,1,1,1,1,1,1,1,1,1,1,1,1,1,1,1,1,1,1,1,1,1,1,1,1,1,1,1,1,1,1,1,1,1,1,1,
1,1,1,1,1,1,1,1,1,1,1,1,1,1,1,1,1,1,1,1,1,1,1,1,1,1,1,1,1,1,1,1,1,1,1,1,
1,1,1,1,1,1,1,1,1,1,1,1,1,1,1,1,1,1,1,1,1,1,1,1,1,1,1,1,1,1,1,1,1,1,1,1,
1,1,1,1,1,1,1,1,1,1,1,1,1,1,1,1,1,1,1,1,1,1,1,1,1,1,1,1,1,1,1,1,1,1,1,1,
1,1,1,1,1,1,1,1,1,1,1,1,1,1,1,1,1,1,1,1,1,1,1,1,1,1,1,1,1,1,1,1,1,1,1,1,
1,1,1,1,1,1,1,1,4),(0.,0.184512097253587),(12.0092477762453,12.5089268430284,
13.0086059098114,13.5082849765944,14.0079640433774,14.5076431101605,15.0073221769435,
15.5070012437265,16.0066803105095,16.5063593772925,17.0060384440756,17.5057175108586,
18.0053965776416,18.5050756444246,19.0047547112077,19.5044337779907,20.0041128447737,
20.5037919115567,21.0034709783398,21.5031500451228,22.0028291119058,22.5025081786888,
23.0021872454719,23.5018663122549,24.0015453790379,24.5012244458209,25.0009035126039,
25.500582579387,26.00026164617,26.499940712953,26.999619779736,27.4992988465191,
27.9989779133021,28.4986569800851,28.9983360468681,29.4980151136512,29.9976941804342,
30.4973732472172,30.9970523140002,31.4967313807832,31.9964104475663,32.4960895143493,
32.9957685811323,33.4954476479153,33.9951267146984,34.4948057814814,34.9944848482644,
35.4941639150474,35.9938429818305,36.4935220486135,36.9932011153965,37.4928801821795,
37.9925592489626,38.4922383157456,38.9919173825286,39.4915964493116,39.9912755160946,
40.4909545828777,40.9906336496607,41.4903127164437,41.9899917832267,42.4896708500098,
42.9893499167928,43.4890289835758,43.9887080503588,44.4883871171419,44.9880661839249,
45.4877452507079,45.9874243174909,46.4871033842739,46.986782451057,47.48646151784,
47.986140584623,48.485819651406,48.9854987181891,49.4851777849721,49.9848568517551,
50.4845359185381,50.9842149853212,51.4838940521042,51.9835731188872,52.4832521856702,
52.9829312524532,53.4826103192363,53.9822893860193,54.4819684528023,54.9816475195853,
55.4813265863684,55.9810056531514,56.4806847199344,56.9803637867174,57.4800428535005,
57.9797219202835,58.4794009870665,58.9790800538495,59.4787591206325,59.9784381874156,
60.4781172541986,60.9777963209816,61.4774753877646,61.9771544545477,62.9765125881137,
63.9758707216798,64.9752288552458,65.9745869888119,66.9739451223779,67.9733032559439,
68.97266138951,69.972019523076,70.9713776566421,71.9707357902081,72.9700939237742,
73.9694520573402,74.9688101909063,75.9681683244723,76.9675264580384,77.9668845916044,
78.9662427251705,79.9656008587365,80.9649589923026,81.9643171258686,82.9636752594347,
83.9630333930007,84.9623915265667,85.9617496601328,86.9611077936988,87.9604659272649,
88.9598240608309,89.959182194397,90.958540327963,91.9578984615291,92.9572565950951,
93.9566147286612,94.9559728622272,95.9553309957932,96.9546891293593,97.9540472629253,
98.9534053964914,99.9527635300574,100.952121663623,101.95147979719,102.950837930756,
103.950196064322,104.949554197888,105.948912331454,106.94827046502,107.947628598586,
108.946986732152,109.946344865718,110.945702999284,111.94506113285,112.944419266416,
113.943777399982,114.943135533548,115.942493667114,116.94185180068,117.941209934246,
118.940568067812,119.939926201378,120.939284334944,121.93864246851,122.938000602077,
123.937358735643,124.936716869209,125.936075002775,126.935433136341,127.934791269907,
128.934149403473,129.933507537039,130.932865670605,131.932223804171,132.931581937737,
133.930940071303,134.930298204869,135.929656338435,136.929014472001,137.928372605567,
138.927730739133,139.927088872699,140.926447006265,141.925805139831,142.925163273397,
143.924521406963,144.92387954053,145.923237674096,146.922595807662,147.921953941228,
148.921312074794,149.92067020836,150.920028341926,151.919386475492,152.918744609058,
153.918102742624,154.91746087619,155.916819009756,156.916177143322,157.915535276888,
158.914893410454,159.91425154402,160.913609677586,161.912967811152,162.912325944718,
163.911684078284,164.91104221185,165.910400345416,166.909758478983,167.909116612549,
168.908474746115,169.907832879681,170.907191013247,171.906549146813,172.905907280379,
173.905265413945,174.904623547511,175.903981681077,176.903339814643,177.902697948209,
178.902056081775,179.901414215341,180.900772348907,181.900130482473,182.899488616039,
183.898846749605,184.898204883171,185.897563016737,186.896921150303,187.89627928387,
188.895637417436,189.894995551002,190.894353684568,191.893711818134,192.8930699517,
193.892428085266,194.891786218832,195.891144352398,196.890502485964,197.88986061953,
198.889218753096,199.888576886662,200.887935020228,201.887293153794,202.88665128736,
203.886009420926,204.885367554492,205.884725688058,206.884083821624,207.88344195519,
208.882800088756,209.882158222323,210.881516355889,211.880874489455,212.880232623021,
213.879590756587,214.878948890153,215.878307023719,216.877665157285,217.877023290851,
218.876381424417,219.875739557983,220.875097691549,221.874455825115,222.873813958681,
223.873172092247,224.872530225813,225.871888359379,226.871246492945,227.870604626511,
228.869962760077,229.869320893643,230.86867902721,231.868037160776,232.867395294342,
233.866753427908,234.866111561474,235.86546969504,236.864827828606,237.864185962172,
238.863544095738,239.862902229304,240.86226036287,241.861618496436,242.860976630002,
243.860334763568,244.859692897134,245.8590510307,246.858409164266,247.857767297832,
248.857125431398,249.856483564964,250.85584169853,251.855199832097,252.854557965663,
253.853916099229,254.853274232795,255.852632366361,256.851990499927,257.851348633493,
258.850706767059,259.850064900625,260.849423034191,261.848781167757,262.848139301323,
263.847497434889,264.846855568455,265.846213702021,266.845571835587,267.844929969153,
268.844288102719,269.843646236285,270.843004369851,271.842362503417,272.841720636983,
273.84107877055,274.840436904116,275.839795037682,276.839153171248,277.838511304814,
278.83786943838,279.837227571946,280.836585705512,281.835943839078,282.835301972644,
283.83466010621,284.834018239776,285.833376373342,286.832734506908,287.832092640474,
288.83145077404,289.830808907606,290.830167041172,291.829525174738,292.828883308304,
293.82824144187,294.827599575437,295.826957709003,296.826315842569,297.825673976135,
298.825032109701,299.824390243267,300.823748376833,301.823106510399,302.822464643965,
303.821822777531,304.821180911097,305.820539044663,306.819897178229,307.819255311795,
308.818613445361,309.817971578927,310.817329712493,311.816687846059,312.816045979625,
313.815404113191,314.814762246757,315.814120380323,316.81347851389,317.812836647456,
318.812194781022,319.811552914588,320.810911048154,321.81026918172,322.809627315286,
323.808985448852,324.808343582418,325.807701715984,326.80705984955,327.806417983116,
328.805776116682,329.805134250248,330.804492383814,331.80385051738,332.803208650946,
333.802566784512,334.801924918078,335.801283051644,336.80064118521,337.799999318776,
338.799357452343,339.798715585909,340.798073719475,341.797431853041,342.796789986607,
343.796148120173,344.795506253739,345.794864387305,346.794222520871,347.793580654437,
348.792938788003,349.792296921569,350.791655055135,351.791013188701,352.790371322267,
353.789729455833,354.789087589399,355.788445722965,356.787803856531,357.287482923314,
357.787161990097,358.28684105688,358.786520123663,359.286199190446,359.78587825723,
360.285557324013,360.785236390796,361.284915457579,361.784594524362,362.284273591145,
362.783952657928,363.283631724711,363.783310791494,364.282989858277,364.78266892506,
365.282347991843,365.782027058626,366.281706125409,366.781385192192,367.281064258975,
367.780743325758,368.280422392541,368.780101459324,369.279780526107,369.77945959289,
370.279138659673,370.778817726456,371.278496793239,371.778175860022,372.277854926805,
372.777533993588,373.277213060371,373.776892127154,374.276571193937,374.77625026072,
375.275929327503,375.775608394286,376.275287461069,376.774966527852,377.274645594635,
377.774324661418,378.274003728201,378.773682794984,379.273361861767,379.77304092855,
380.272719995333,380.772399062117,381.2720781289,381.771757195683,382.271436262466,
382.771115329249,383.270794396032,383.770473462815,384.270152529598,384.769831596381,
385.269510663164,385.769189729947,386.26886879673,386.768547863513,387.268226930296,
387.767905997079,388.267585063862,388.767264130645,389.266943197428,389.766622264211,
390.266301330994,390.765980397777,391.26565946456,391.765338531343,392.265017598126,
392.764696664909,393.264375731692,393.764054798475,394.263733865258,394.763412932041,
395.263091998824,395.762771065607,396.26245013239,396.762129199173,397.261808265956,
397.761487332739,398.261166399522,398.760845466305,399.260524533088,399.760203599871,
400.259882666654,400.759561733437,401.25924080022,401.758919867003,402.258598933787,
402.75827800057,403.257957067353,403.757636134136,404.257315200919,404.756994267702,
405.256673334485,405.756352401268,406.256031468051,406.755710534834),
 .UNSPECIFIED.);
#15=B_SPLINE_SURFACE_WITH_KNOTS('',3,3,((#51310,#51311,#51312,#51313,#51314,
#51315,#51316,#51317,#51318,#51319,#51320,#51321,#51322,#51323,#51324,#51325,
#51326,#51327,#51328,#51329,#51330,#51331,#51332,#51333,#51334,#51335,#51336,
#51337,#51338,#51339,#51340,#51341,#51342,#51343,#51344,#51345,#51346,#51347,
#51348,#51349,#51350,#51351,#51352,#51353,#51354,#51355,#51356,#51357,#51358,
#51359,#51360,#51361,#51362,#51363,#51364,#51365,#51366,#51367,#51368,#51369,
#51370,#51371,#51372,#51373,#51374,#51375,#51376,#51377,#51378,#51379,#51380,
#51381,#51382,#51383,#51384,#51385,#51386,#51387,#51388,#51389,#51390,#51391,
#51392,#51393,#51394,#51395,#51396,#51397,#51398,#51399,#51400,#51401,#51402,
#51403,#51404,#51405,#51406,#51407,#51408,#51409,#51410,#51411,#51412,#51413,
#51414,#51415,#51416,#51417,#51418,#51419,#51420,#51421,#51422,#51423,#51424),
(#51425,#51426,#51427,#51428,#51429,#51430,#51431,#51432,#51433,#51434,
#51435,#51436,#51437,#51438,#51439,#51440,#51441,#51442,#51443,#51444,#51445,
#51446,#51447,#51448,#51449,#51450,#51451,#51452,#51453,#51454,#51455,#51456,
#51457,#51458,#51459,#51460,#51461,#51462,#51463,#51464,#51465,#51466,#51467,
#51468,#51469,#51470,#51471,#51472,#51473,#51474,#51475,#51476,#51477,#51478,
#51479,#51480,#51481,#51482,#51483,#51484,#51485,#51486,#51487,#51488,#51489,
#51490,#51491,#51492,#51493,#51494,#51495,#51496,#51497,#51498,#51499,#51500,
#51501,#51502,#51503,#51504,#51505,#51506,#51507,#51508,#51509,#51510,#51511,
#51512,#51513,#51514,#51515,#51516,#51517,#51518,#51519,#51520,#51521,#51522,
#51523,#51524,#51525,#51526,#51527,#51528,#51529,#51530,#51531,#51532,#51533,
#51534,#51535,#51536,#51537,#51538,#51539),(#51540,#51541,#51542,#51543,
#51544,#51545,#51546,#51547,#51548,#51549,#51550,#51551,#51552,#51553,#51554,
#51555,#51556,#51557,#51558,#51559,#51560,#51561,#51562,#51563,#51564,#51565,
#51566,#51567,#51568,#51569,#51570,#51571,#51572,#51573,#51574,#51575,#51576,
#51577,#51578,#51579,#51580,#51581,#51582,#51583,#51584,#51585,#51586,#51587,
#51588,#51589,#51590,#51591,#51592,#51593,#51594,#51595,#51596,#51597,#51598,
#51599,#51600,#51601,#51602,#51603,#51604,#51605,#51606,#51607,#51608,#51609,
#51610,#51611,#51612,#51613,#51614,#51615,#51616,#51617,#51618,#51619,#51620,
#51621,#51622,#51623,#51624,#51625,#51626,#51627,#51628,#51629,#51630,#51631,
#51632,#51633,#51634,#51635,#51636,#51637,#51638,#51639,#51640,#51641,#51642,
#51643,#51644,#51645,#51646,#51647,#51648,#51649,#51650,#51651,#51652,#51653,
#51654),(#51655,#51656,#51657,#51658,#51659,#51660,#51661,#51662,#51663,
#51664,#51665,#51666,#51667,#51668,#51669,#51670,#51671,#51672,#51673,#51674,
#51675,#51676,#51677,#51678,#51679,#51680,#51681,#51682,#51683,#51684,#51685,
#51686,#51687,#51688,#51689,#51690,#51691,#51692,#51693,#51694,#51695,#51696,
#51697,#51698,#51699,#51700,#51701,#51702,#51703,#51704,#51705,#51706,#51707,
#51708,#51709,#51710,#51711,#51712,#51713,#51714,#51715,#51716,#51717,#51718,
#51719,#51720,#51721,#51722,#51723,#51724,#51725,#51726,#51727,#51728,#51729,
#51730,#51731,#51732,#51733,#51734,#51735,#51736,#51737,#51738,#51739,#51740,
#51741,#51742,#51743,#51744,#51745,#51746,#51747,#51748,#51749,#51750,#51751,
#51752,#51753,#51754,#51755,#51756,#51757,#51758,#51759,#51760,#51761,#51762,
#51763,#51764,#51765,#51766,#51767,#51768,#51769)),.UNSPECIFIED.,.F.,.F.,
 .F.,(4,4),(4,1,1,1,1,1,1,1,1,1,1,1,1,1,1,1,1,1,1,1,1,1,1,1,1,1,1,1,1,1,
1,1,1,1,1,1,1,1,1,1,1,1,1,1,1,1,1,1,1,1,1,1,1,1,1,1,1,1,1,1,1,1,1,1,1,1,
1,1,1,1,1,1,1,1,1,1,1,1,1,1,1,1,1,1,1,1,1,1,1,1,1,1,1,1,1,1,1,1,1,1,1,1,
1,1,1,1,1,1,1,1,1,1,4),(0.,0.173020531651036),(12.1475814751569,12.6421543672732,
13.1367272593894,13.6313001515056,14.1258730436219,14.6204459357381,15.1150188278544,
15.6095917199706,16.1041646120869,16.5987375042031,17.0933103963194,17.5878832884356,
18.0824561805519,18.5770290726681,19.0716019647843,19.5661748569006,20.0607477490168,
20.5553206411331,21.0498935332493,21.5444664253656,22.0390393174818,22.5336122095981,
23.0281851017143,23.5227579938306,24.0173308859468,24.511903778063,25.0064766701793,
25.5010495622955,25.9956224544118,26.490195346528,26.9847682386443,27.4793411307605,
27.9739140228768,28.468486914993,28.9630598071093,29.4576326992255,29.9522055913417,
30.446778483458,30.9413513755742,31.4359242676905,31.9304971598067,32.425070051923,
32.9196429440392,33.4142158361555,33.9087887282717,34.403361620388,34.8979345125042,
35.3925074046204,35.8870802967367,36.3816531888529,36.8762260809692,37.3707989730854,
37.8653718652017,38.3599447573179,38.8545176494342,39.3490905415504,39.8436634336667,
40.3382363257829,40.8328092178991,41.3273821100154,41.8219550021316,42.3165278942479,
42.8111007863641,43.3056736784804,43.8002465705966,44.2948194627129,44.7893923548291,
45.2839652469454,45.7785381390616,46.2731110311778,46.7676839232941,47.2622568154103,
47.7568297075266,48.2514025996428,48.7459754917591,49.2405483838753,49.7351212759916,
50.2296941681078,50.7242670602241,51.2188399523403,51.7134128444565,52.2079857365728,
52.702558628689,53.1971315208053,53.6917044129215,54.1862773050378,54.680850197154,
55.1754230892703,55.6699959813865,56.1645688735028,56.659141765619,57.1537146577353,
57.6482875498515,58.1428604419677,58.637433334084,59.1320062262002,59.6265791183165,
60.1211520104327,60.615724902549,61.1102977946652,61.6048706867815,62.0994435788977,
62.5940164710139,63.0885893631302,63.5831622552464,64.0777351473627,64.5723080394789,
65.0668809315952,65.5614538237114,66.0560267158277,66.5505996079439,67.0451725000601,
67.5397453921764),.UNSPECIFIED.);
#16=B_SPLINE_SURFACE_WITH_KNOTS('',3,3,((#51869,#51870,#51871,#51872,#51873,
#51874,#51875,#51876,#51877,#51878,#51879,#51880,#51881,#51882,#51883,#51884,
#51885,#51886,#51887,#51888,#51889,#51890,#51891,#51892,#51893,#51894,#51895,
#51896,#51897,#51898,#51899,#51900,#51901,#51902,#51903,#51904,#51905,#51906,
#51907,#51908,#51909,#51910,#51911,#51912,#51913,#51914,#51915,#51916,#51917,
#51918,#51919,#51920,#51921,#51922,#51923,#51924,#51925,#51926,#51927,#51928,
#51929,#51930,#51931,#51932,#51933,#51934,#51935,#51936,#51937,#51938,#51939,
#51940,#51941,#51942,#51943,#51944,#51945,#51946,#51947,#51948,#51949,#51950,
#51951,#51952,#51953,#51954,#51955,#51956,#51957,#51958,#51959,#51960,#51961,
#51962,#51963,#51964,#51965,#51966,#51967,#51968,#51969,#51970,#51971,#51972,
#51973,#51974,#51975,#51976,#51977,#51978,#51979,#51980,#51981,#51982,#51983),
(#51984,#51985,#51986,#51987,#51988,#51989,#51990,#51991,#51992,#51993,
#51994,#51995,#51996,#51997,#51998,#51999,#52000,#52001,#52002,#52003,#52004,
#52005,#52006,#52007,#52008,#52009,#52010,#52011,#52012,#52013,#52014,#52015,
#52016,#52017,#52018,#52019,#52020,#52021,#52022,#52023,#52024,#52025,#52026,
#52027,#52028,#52029,#52030,#52031,#52032,#52033,#52034,#52035,#52036,#52037,
#52038,#52039,#52040,#52041,#52042,#52043,#52044,#52045,#52046,#52047,#52048,
#52049,#52050,#52051,#52052,#52053,#52054,#52055,#52056,#52057,#52058,#52059,
#52060,#52061,#52062,#52063,#52064,#52065,#52066,#52067,#52068,#52069,#52070,
#52071,#52072,#52073,#52074,#52075,#52076,#52077,#52078,#52079,#52080,#52081,
#52082,#52083,#52084,#52085,#52086,#52087,#52088,#52089,#52090,#52091,#52092,
#52093,#52094,#52095,#52096,#52097,#52098),(#52099,#52100,#52101,#52102,
#52103,#52104,#52105,#52106,#52107,#52108,#52109,#52110,#52111,#52112,#52113,
#52114,#52115,#52116,#52117,#52118,#52119,#52120,#52121,#52122,#52123,#52124,
#52125,#52126,#52127,#52128,#52129,#52130,#52131,#52132,#52133,#52134,#52135,
#52136,#52137,#52138,#52139,#52140,#52141,#52142,#52143,#52144,#52145,#52146,
#52147,#52148,#52149,#52150,#52151,#52152,#52153,#52154,#52155,#52156,#52157,
#52158,#52159,#52160,#52161,#52162,#52163,#52164,#52165,#52166,#52167,#52168,
#52169,#52170,#52171,#52172,#52173,#52174,#52175,#52176,#52177,#52178,#52179,
#52180,#52181,#52182,#52183,#52184,#52185,#52186,#52187,#52188,#52189,#52190,
#52191,#52192,#52193,#52194,#52195,#52196,#52197,#52198,#52199,#52200,#52201,
#52202,#52203,#52204,#52205,#52206,#52207,#52208,#52209,#52210,#52211,#52212,
#52213),(#52214,#52215,#52216,#52217,#52218,#52219,#52220,#52221,#52222,
#52223,#52224,#52225,#52226,#52227,#52228,#52229,#52230,#52231,#52232,#52233,
#52234,#52235,#52236,#52237,#52238,#52239,#52240,#52241,#52242,#52243,#52244,
#52245,#52246,#52247,#52248,#52249,#52250,#52251,#52252,#52253,#52254,#52255,
#52256,#52257,#52258,#52259,#52260,#52261,#52262,#52263,#52264,#52265,#52266,
#52267,#52268,#52269,#52270,#52271,#52272,#52273,#52274,#52275,#52276,#52277,
#52278,#52279,#52280,#52281,#52282,#52283,#52284,#52285,#52286,#52287,#52288,
#52289,#52290,#52291,#52292,#52293,#52294,#52295,#52296,#52297,#52298,#52299,
#52300,#52301,#52302,#52303,#52304,#52305,#52306,#52307,#52308,#52309,#52310,
#52311,#52312,#52313,#52314,#52315,#52316,#52317,#52318,#52319,#52320,#52321,
#52322,#52323,#52324,#52325,#52326,#52327,#52328)),.UNSPECIFIED.,.F.,.F.,
 .F.,(4,4),(4,1,1,1,1,1,1,1,1,1,1,1,1,1,1,1,1,1,1,1,1,1,1,1,1,1,1,1,1,1,
1,1,1,1,1,1,1,1,1,1,1,1,1,1,1,1,1,1,1,1,1,1,1,1,1,1,1,1,1,1,1,1,1,1,1,1,
1,1,1,1,1,1,1,1,1,1,1,1,1,1,1,1,1,1,1,1,1,1,1,1,1,1,1,1,1,1,1,1,1,1,1,1,
1,1,1,1,1,1,1,1,1,1,4),(0.,0.173020531651036),(15.1888611523549,15.6834340444711,
16.1780069365874,16.6725798287036,17.1671527208199,17.6617256129361,18.1562985050523,
18.6508713971686,19.1454442892848,19.6400171814011,20.1345900735173,20.6291629656336,
21.1237358577498,21.6183087498661,22.1128816419823,22.6074545340986,23.1020274262148,
23.596600318331,24.0911732104473,24.5857461025635,25.0803189946798,25.574891886796,
26.0694647789123,26.5640376710285,27.0586105631448,27.553183455261,28.0477563473773,
28.5423292394935,29.0369021316097,29.531475023726,30.0260479158422,30.5206208079585,
31.0151937000747,31.509766592191,32.0043394843072,32.4989123764235,32.9934852685397,
33.488058160656,33.9826310527722,34.4772039448884,34.9717768370047,35.4663497291209,
35.9609226212372,36.4554955133534,36.9500684054697,37.4446412975859,37.9392141897022,
38.4337870818184,38.9283599739347,39.4229328660509,39.9175057581671,40.4120786502834,
40.9066515423996,41.4012244345159,41.8957973266321,42.3903702187484,42.8849431108646,
43.3795160029809,43.8740888950971,44.3686617872134,44.8632346793296,45.3578075714458,
45.8523804635621,46.3469533556783,46.8415262477946,47.3360991399108,47.8306720320271,
48.3252449241433,48.8198178162596,49.3143907083758,49.8089636004921,50.3035364926083,
50.7981093847245,51.2926822768408,51.787255168957,52.2818280610733,52.7764009531895,
53.2709738453058,53.765546737422,54.2601196295383,54.7546925216545,55.2492654137708,
55.743838305887,56.2384111980032,56.7329840901195,57.2275569822357,57.722129874352,
58.2167027664682,58.7112756585845,59.2058485507007,59.700421442817,60.1949943349332,
60.6895672270495,61.1841401191657,61.6787130112819,62.1732859033982,62.6678587955144,
63.1624316876307,63.6570045797469,64.1515774718632,64.6461503639794,65.1407232560957,
65.6352961482119,66.1298690403281,66.6244419324444,67.1190148245607,67.6135877166769,
68.1081606087931,68.6027335009094,69.0973063930256,69.5918792851419,70.0864521772581,
70.5810250693744),.UNSPECIFIED.);
#17=B_SPLINE_SURFACE_WITH_KNOTS('',3,3,((#58111,#58112,#58113,#58114,#58115,
#58116,#58117,#58118,#58119,#58120,#58121,#58122,#58123,#58124,#58125,#58126,
#58127,#58128,#58129,#58130,#58131,#58132,#58133,#58134,#58135,#58136,#58137,
#58138,#58139,#58140,#58141,#58142,#58143,#58144,#58145,#58146,#58147,#58148,
#58149,#58150,#58151,#58152,#58153,#58154,#58155,#58156,#58157,#58158,#58159,
#58160,#58161,#58162,#58163,#58164,#58165,#58166,#58167,#58168,#58169,#58170,
#58171,#58172,#58173,#58174,#58175,#58176,#58177,#58178,#58179,#58180,#58181,
#58182,#58183,#58184,#58185,#58186,#58187,#58188,#58189,#58190,#58191,#58192,
#58193,#58194,#58195,#58196,#58197,#58198,#58199,#58200,#58201,#58202,#58203,
#58204,#58205,#58206,#58207,#58208,#58209,#58210,#58211,#58212,#58213,#58214,
#58215,#58216,#58217,#58218,#58219,#58220,#58221,#58222,#58223,#58224,#58225,
#58226,#58227,#58228,#58229,#58230,#58231,#58232,#58233,#58234,#58235,#58236,
#58237,#58238,#58239,#58240,#58241,#58242,#58243,#58244,#58245,#58246,#58247,
#58248,#58249,#58250,#58251,#58252,#58253,#58254,#58255,#58256,#58257,#58258,
#58259,#58260,#58261,#58262,#58263,#58264,#58265,#58266,#58267,#58268,#58269,
#58270,#58271,#58272,#58273,#58274,#58275,#58276,#58277,#58278,#58279,#58280,
#58281,#58282,#58283,#58284,#58285,#58286,#58287,#58288,#58289,#58290,#58291,
#58292,#58293,#58294,#58295,#58296,#58297,#58298,#58299,#58300,#58301,#58302,
#58303,#58304,#58305,#58306,#58307,#58308,#58309,#58310,#58311,#58312,#58313,
#58314,#58315,#58316,#58317,#58318,#58319,#58320,#58321,#58322,#58323,#58324,
#58325,#58326,#58327,#58328,#58329,#58330,#58331,#58332,#58333,#58334,#58335,
#58336,#58337,#58338,#58339,#58340,#58341,#58342,#58343,#58344,#58345,#58346,
#58347,#58348,#58349,#58350,#58351,#58352,#58353,#58354,#58355,#58356,#58357,
#58358,#58359,#58360,#58361,#58362,#58363,#58364,#58365,#58366,#58367,#58368,
#58369,#58370,#58371,#58372,#58373,#58374,#58375,#58376,#58377,#58378,#58379,
#58380,#58381,#58382,#58383,#58384,#58385,#58386,#58387,#58388,#58389,#58390,
#58391,#58392,#58393,#58394,#58395,#58396,#58397,#58398,#58399,#58400,#58401,
#58402,#58403,#58404,#58405,#58406,#58407,#58408,#58409,#58410,#58411,#58412,
#58413,#58414,#58415,#58416,#58417,#58418,#58419,#58420,#58421,#58422,#58423,
#58424,#58425,#58426,#58427,#58428,#58429,#58430,#58431,#58432,#58433,#58434,
#58435,#58436,#58437,#58438,#58439,#58440,#58441,#58442,#58443,#58444,#58445,
#58446,#58447,#58448,#58449,#58450,#58451,#58452,#58453,#58454,#58455,#58456,
#58457,#58458,#58459,#58460,#58461,#58462,#58463,#58464,#58465,#58466,#58467,
#58468,#58469,#58470,#58471,#58472,#58473,#58474,#58475,#58476,#58477,#58478,
#58479,#58480,#58481,#58482,#58483,#58484,#58485,#58486,#58487,#58488,#58489,
#58490,#58491,#58492,#58493,#58494,#58495,#58496,#58497,#58498,#58499,#58500,
#58501,#58502,#58503,#58504,#58505,#58506,#58507,#58508,#58509,#58510,#58511,
#58512,#58513,#58514,#58515,#58516,#58517,#58518,#58519,#58520,#58521,#58522,
#58523,#58524,#58525,#58526,#58527,#58528,#58529,#58530,#58531,#58532,#58533,
#58534,#58535,#58536,#58537,#58538,#58539,#58540,#58541,#58542,#58543,#58544,
#58545,#58546,#58547,#58548,#58549,#58550,#58551,#58552,#58553,#58554,#58555,
#58556,#58557,#58558,#58559,#58560,#58561,#58562,#58563,#58564,#58565,#58566,
#58567,#58568,#58569,#58570,#58571,#58572,#58573,#58574,#58575,#58576,#58577,
#58578,#58579,#58580,#58581,#58582,#58583,#58584,#58585,#58586,#58587,#58588,
#58589,#58590,#58591,#58592,#58593,#58594,#58595,#58596,#58597,#58598,#58599,
#58600,#58601,#58602,#58603,#58604,#58605,#58606,#58607,#58608),(#58609,
#58610,#58611,#58612,#58613,#58614,#58615,#58616,#58617,#58618,#58619,#58620,
#58621,#58622,#58623,#58624,#58625,#58626,#58627,#58628,#58629,#58630,#58631,
#58632,#58633,#58634,#58635,#58636,#58637,#58638,#58639,#58640,#58641,#58642,
#58643,#58644,#58645,#58646,#58647,#58648,#58649,#58650,#58651,#58652,#58653,
#58654,#58655,#58656,#58657,#58658,#58659,#58660,#58661,#58662,#58663,#58664,
#58665,#58666,#58667,#58668,#58669,#58670,#58671,#58672,#58673,#58674,#58675,
#58676,#58677,#58678,#58679,#58680,#58681,#58682,#58683,#58684,#58685,#58686,
#58687,#58688,#58689,#58690,#58691,#58692,#58693,#58694,#58695,#58696,#58697,
#58698,#58699,#58700,#58701,#58702,#58703,#58704,#58705,#58706,#58707,#58708,
#58709,#58710,#58711,#58712,#58713,#58714,#58715,#58716,#58717,#58718,#58719,
#58720,#58721,#58722,#58723,#58724,#58725,#58726,#58727,#58728,#58729,#58730,
#58731,#58732,#58733,#58734,#58735,#58736,#58737,#58738,#58739,#58740,#58741,
#58742,#58743,#58744,#58745,#58746,#58747,#58748,#58749,#58750,#58751,#58752,
#58753,#58754,#58755,#58756,#58757,#58758,#58759,#58760,#58761,#58762,#58763,
#58764,#58765,#58766,#58767,#58768,#58769,#58770,#58771,#58772,#58773,#58774,
#58775,#58776,#58777,#58778,#58779,#58780,#58781,#58782,#58783,#58784,#58785,
#58786,#58787,#58788,#58789,#58790,#58791,#58792,#58793,#58794,#58795,#58796,
#58797,#58798,#58799,#58800,#58801,#58802,#58803,#58804,#58805,#58806,#58807,
#58808,#58809,#58810,#58811,#58812,#58813,#58814,#58815,#58816,#58817,#58818,
#58819,#58820,#58821,#58822,#58823,#58824,#58825,#58826,#58827,#58828,#58829,
#58830,#58831,#58832,#58833,#58834,#58835,#58836,#58837,#58838,#58839,#58840,
#58841,#58842,#58843,#58844,#58845,#58846,#58847,#58848,#58849,#58850,#58851,
#58852,#58853,#58854,#58855,#58856,#58857,#58858,#58859,#58860,#58861,#58862,
#58863,#58864,#58865,#58866,#58867,#58868,#58869,#58870,#58871,#58872,#58873,
#58874,#58875,#58876,#58877,#58878,#58879,#58880,#58881,#58882,#58883,#58884,
#58885,#58886,#58887,#58888,#58889,#58890,#58891,#58892,#58893,#58894,#58895,
#58896,#58897,#58898,#58899,#58900,#58901,#58902,#58903,#58904,#58905,#58906,
#58907,#58908,#58909,#58910,#58911,#58912,#58913,#58914,#58915,#58916,#58917,
#58918,#58919,#58920,#58921,#58922,#58923,#58924,#58925,#58926,#58927,#58928,
#58929,#58930,#58931,#58932,#58933,#58934,#58935,#58936,#58937,#58938,#58939,
#58940,#58941,#58942,#58943,#58944,#58945,#58946,#58947,#58948,#58949,#58950,
#58951,#58952,#58953,#58954,#58955,#58956,#58957,#58958,#58959,#58960,#58961,
#58962,#58963,#58964,#58965,#58966,#58967,#58968,#58969,#58970,#58971,#58972,
#58973,#58974,#58975,#58976,#58977,#58978,#58979,#58980,#58981,#58982,#58983,
#58984,#58985,#58986,#58987,#58988,#58989,#58990,#58991,#58992,#58993,#58994,
#58995,#58996,#58997,#58998,#58999,#59000,#59001,#59002,#59003,#59004,#59005,
#59006,#59007,#59008,#59009,#59010,#59011,#59012,#59013,#59014,#59015,#59016,
#59017,#59018,#59019,#59020,#59021,#59022,#59023,#59024,#59025,#59026,#59027,
#59028,#59029,#59030,#59031,#59032,#59033,#59034,#59035,#59036,#59037,#59038,
#59039,#59040,#59041,#59042,#59043,#59044,#59045,#59046,#59047,#59048,#59049,
#59050,#59051,#59052,#59053,#59054,#59055,#59056,#59057,#59058,#59059,#59060,
#59061,#59062,#59063,#59064,#59065,#59066,#59067,#59068,#59069,#59070,#59071,
#59072,#59073,#59074,#59075,#59076,#59077,#59078,#59079,#59080,#59081,#59082,
#59083,#59084,#59085,#59086,#59087,#59088,#59089,#59090,#59091,#59092,#59093,
#59094,#59095,#59096,#59097,#59098,#59099,#59100,#59101,#59102,#59103,#59104,
#59105,#59106),(#59107,#59108,#59109,#59110,#59111,#59112,#59113,#59114,
#59115,#59116,#59117,#59118,#59119,#59120,#59121,#59122,#59123,#59124,#59125,
#59126,#59127,#59128,#59129,#59130,#59131,#59132,#59133,#59134,#59135,#59136,
#59137,#59138,#59139,#59140,#59141,#59142,#59143,#59144,#59145,#59146,#59147,
#59148,#59149,#59150,#59151,#59152,#59153,#59154,#59155,#59156,#59157,#59158,
#59159,#59160,#59161,#59162,#59163,#59164,#59165,#59166,#59167,#59168,#59169,
#59170,#59171,#59172,#59173,#59174,#59175,#59176,#59177,#59178,#59179,#59180,
#59181,#59182,#59183,#59184,#59185,#59186,#59187,#59188,#59189,#59190,#59191,
#59192,#59193,#59194,#59195,#59196,#59197,#59198,#59199,#59200,#59201,#59202,
#59203,#59204,#59205,#59206,#59207,#59208,#59209,#59210,#59211,#59212,#59213,
#59214,#59215,#59216,#59217,#59218,#59219,#59220,#59221,#59222,#59223,#59224,
#59225,#59226,#59227,#59228,#59229,#59230,#59231,#59232,#59233,#59234,#59235,
#59236,#59237,#59238,#59239,#59240,#59241,#59242,#59243,#59244,#59245,#59246,
#59247,#59248,#59249,#59250,#59251,#59252,#59253,#59254,#59255,#59256,#59257,
#59258,#59259,#59260,#59261,#59262,#59263,#59264,#59265,#59266,#59267,#59268,
#59269,#59270,#59271,#59272,#59273,#59274,#59275,#59276,#59277,#59278,#59279,
#59280,#59281,#59282,#59283,#59284,#59285,#59286,#59287,#59288,#59289,#59290,
#59291,#59292,#59293,#59294,#59295,#59296,#59297,#59298,#59299,#59300,#59301,
#59302,#59303,#59304,#59305,#59306,#59307,#59308,#59309,#59310,#59311,#59312,
#59313,#59314,#59315,#59316,#59317,#59318,#59319,#59320,#59321,#59322,#59323,
#59324,#59325,#59326,#59327,#59328,#59329,#59330,#59331,#59332,#59333,#59334,
#59335,#59336,#59337,#59338,#59339,#59340,#59341,#59342,#59343,#59344,#59345,
#59346,#59347,#59348,#59349,#59350,#59351,#59352,#59353,#59354,#59355,#59356,
#59357,#59358,#59359,#59360,#59361,#59362,#59363,#59364,#59365,#59366,#59367,
#59368,#59369,#59370,#59371,#59372,#59373,#59374,#59375,#59376,#59377,#59378,
#59379,#59380,#59381,#59382,#59383,#59384,#59385,#59386,#59387,#59388,#59389,
#59390,#59391,#59392,#59393,#59394,#59395,#59396,#59397,#59398,#59399,#59400,
#59401,#59402,#59403,#59404,#59405,#59406,#59407,#59408,#59409,#59410,#59411,
#59412,#59413,#59414,#59415,#59416,#59417,#59418,#59419,#59420,#59421,#59422,
#59423,#59424,#59425,#59426,#59427,#59428,#59429,#59430,#59431,#59432,#59433,
#59434,#59435,#59436,#59437,#59438,#59439,#59440,#59441,#59442,#59443,#59444,
#59445,#59446,#59447,#59448,#59449,#59450,#59451,#59452,#59453,#59454,#59455,
#59456,#59457,#59458,#59459,#59460,#59461,#59462,#59463,#59464,#59465,#59466,
#59467,#59468,#59469,#59470,#59471,#59472,#59473,#59474,#59475,#59476,#59477,
#59478,#59479,#59480,#59481,#59482,#59483,#59484,#59485,#59486,#59487,#59488,
#59489,#59490,#59491,#59492,#59493,#59494,#59495,#59496,#59497,#59498,#59499,
#59500,#59501,#59502,#59503,#59504,#59505,#59506,#59507,#59508,#59509,#59510,
#59511,#59512,#59513,#59514,#59515,#59516,#59517,#59518,#59519,#59520,#59521,
#59522,#59523,#59524,#59525,#59526,#59527,#59528,#59529,#59530,#59531,#59532,
#59533,#59534,#59535,#59536,#59537,#59538,#59539,#59540,#59541,#59542,#59543,
#59544,#59545,#59546,#59547,#59548,#59549,#59550,#59551,#59552,#59553,#59554,
#59555,#59556,#59557,#59558,#59559,#59560,#59561,#59562,#59563,#59564,#59565,
#59566,#59567,#59568,#59569,#59570,#59571,#59572,#59573,#59574,#59575,#59576,
#59577,#59578,#59579,#59580,#59581,#59582,#59583,#59584,#59585,#59586,#59587,
#59588,#59589,#59590,#59591,#59592,#59593,#59594,#59595,#59596,#59597,#59598,
#59599,#59600,#59601,#59602,#59603,#59604),(#59605,#59606,#59607,#59608,
#59609,#59610,#59611,#59612,#59613,#59614,#59615,#59616,#59617,#59618,#59619,
#59620,#59621,#59622,#59623,#59624,#59625,#59626,#59627,#59628,#59629,#59630,
#59631,#59632,#59633,#59634,#59635,#59636,#59637,#59638,#59639,#59640,#59641,
#59642,#59643,#59644,#59645,#59646,#59647,#59648,#59649,#59650,#59651,#59652,
#59653,#59654,#59655,#59656,#59657,#59658,#59659,#59660,#59661,#59662,#59663,
#59664,#59665,#59666,#59667,#59668,#59669,#59670,#59671,#59672,#59673,#59674,
#59675,#59676,#59677,#59678,#59679,#59680,#59681,#59682,#59683,#59684,#59685,
#59686,#59687,#59688,#59689,#59690,#59691,#59692,#59693,#59694,#59695,#59696,
#59697,#59698,#59699,#59700,#59701,#59702,#59703,#59704,#59705,#59706,#59707,
#59708,#59709,#59710,#59711,#59712,#59713,#59714,#59715,#59716,#59717,#59718,
#59719,#59720,#59721,#59722,#59723,#59724,#59725,#59726,#59727,#59728,#59729,
#59730,#59731,#59732,#59733,#59734,#59735,#59736,#59737,#59738,#59739,#59740,
#59741,#59742,#59743,#59744,#59745,#59746,#59747,#59748,#59749,#59750,#59751,
#59752,#59753,#59754,#59755,#59756,#59757,#59758,#59759,#59760,#59761,#59762,
#59763,#59764,#59765,#59766,#59767,#59768,#59769,#59770,#59771,#59772,#59773,
#59774,#59775,#59776,#59777,#59778,#59779,#59780,#59781,#59782,#59783,#59784,
#59785,#59786,#59787,#59788,#59789,#59790,#59791,#59792,#59793,#59794,#59795,
#59796,#59797,#59798,#59799,#59800,#59801,#59802,#59803,#59804,#59805,#59806,
#59807,#59808,#59809,#59810,#59811,#59812,#59813,#59814,#59815,#59816,#59817,
#59818,#59819,#59820,#59821,#59822,#59823,#59824,#59825,#59826,#59827,#59828,
#59829,#59830,#59831,#59832,#59833,#59834,#59835,#59836,#59837,#59838,#59839,
#59840,#59841,#59842,#59843,#59844,#59845,#59846,#59847,#59848,#59849,#59850,
#59851,#59852,#59853,#59854,#59855,#59856,#59857,#59858,#59859,#59860,#59861,
#59862,#59863,#59864,#59865,#59866,#59867,#59868,#59869,#59870,#59871,#59872,
#59873,#59874,#59875,#59876,#59877,#59878,#59879,#59880,#59881,#59882,#59883,
#59884,#59885,#59886,#59887,#59888,#59889,#59890,#59891,#59892,#59893,#59894,
#59895,#59896,#59897,#59898,#59899,#59900,#59901,#59902,#59903,#59904,#59905,
#59906,#59907,#59908,#59909,#59910,#59911,#59912,#59913,#59914,#59915,#59916,
#59917,#59918,#59919,#59920,#59921,#59922,#59923,#59924,#59925,#59926,#59927,
#59928,#59929,#59930,#59931,#59932,#59933,#59934,#59935,#59936,#59937,#59938,
#59939,#59940,#59941,#59942,#59943,#59944,#59945,#59946,#59947,#59948,#59949,
#59950,#59951,#59952,#59953,#59954,#59955,#59956,#59957,#59958,#59959,#59960,
#59961,#59962,#59963,#59964,#59965,#59966,#59967,#59968,#59969,#59970,#59971,
#59972,#59973,#59974,#59975,#59976,#59977,#59978,#59979,#59980,#59981,#59982,
#59983,#59984,#59985,#59986,#59987,#59988,#59989,#59990,#59991,#59992,#59993,
#59994,#59995,#59996,#59997,#59998,#59999,#60000,#60001,#60002,#60003,#60004,
#60005,#60006,#60007,#60008,#60009,#60010,#60011,#60012,#60013,#60014,#60015,
#60016,#60017,#60018,#60019,#60020,#60021,#60022,#60023,#60024,#60025,#60026,
#60027,#60028,#60029,#60030,#60031,#60032,#60033,#60034,#60035,#60036,#60037,
#60038,#60039,#60040,#60041,#60042,#60043,#60044,#60045,#60046,#60047,#60048,
#60049,#60050,#60051,#60052,#60053,#60054,#60055,#60056,#60057,#60058,#60059,
#60060,#60061,#60062,#60063,#60064,#60065,#60066,#60067,#60068,#60069,#60070,
#60071,#60072,#60073,#60074,#60075,#60076,#60077,#60078,#60079,#60080,#60081,
#60082,#60083,#60084,#60085,#60086,#60087,#60088,#60089,#60090,#60091,#60092,
#60093,#60094,#60095,#60096,#60097,#60098,#60099,#60100,#60101,#60102)),
 .UNSPECIFIED.,.F.,.F.,.F.,(4,4),(4,1,1,1,1,1,1,1,1,1,1,1,1,1,1,1,1,1,1,
1,1,1,1,1,1,1,1,1,1,1,1,1,1,1,1,1,1,1,1,1,1,1,1,1,1,1,1,1,1,1,1,1,1,1,1,
1,1,1,1,1,1,1,1,1,1,1,1,1,1,1,1,1,1,1,1,1,1,1,1,1,1,1,1,1,1,1,1,1,1,1,1,
1,1,1,1,1,1,1,1,1,1,1,1,1,1,1,1,1,1,1,1,1,1,1,1,1,1,1,1,1,1,1,1,1,1,1,1,
1,1,1,1,1,1,1,1,1,1,1,1,1,1,1,1,1,1,1,1,1,1,1,1,1,1,1,1,1,1,1,1,1,1,1,1,
1,1,1,1,1,1,1,1,1,1,1,1,1,1,1,1,1,1,1,1,1,1,1,1,1,1,1,1,1,1,1,1,1,1,1,1,
1,1,1,1,1,1,1,1,1,1,1,1,1,1,1,1,1,1,1,1,1,1,1,1,1,1,1,1,1,1,1,1,1,1,1,1,
1,1,1,1,1,1,1,1,1,1,1,1,1,1,1,1,1,1,1,1,1,1,1,1,1,1,1,1,1,1,1,1,1,1,1,1,
1,1,1,1,1,1,1,1,1,1,1,1,1,1,1,1,1,1,1,1,1,1,1,1,1,1,1,1,1,1,1,1,1,1,1,1,
1,1,1,1,1,1,1,1,1,1,1,1,1,1,1,1,1,1,1,1,1,1,1,1,1,1,1,1,1,1,1,1,1,1,1,1,
1,1,1,1,1,1,1,1,1,1,1,1,1,1,1,1,1,1,1,1,1,1,1,1,1,1,1,1,1,1,1,1,1,1,1,1,
1,1,1,1,1,1,1,1,1,1,1,1,1,1,1,1,1,1,1,1,1,1,1,1,1,1,1,1,1,1,1,1,1,1,1,1,
1,1,1,1,1,1,1,1,1,1,1,1,1,1,1,1,1,1,1,1,1,1,1,1,1,1,1,1,1,1,1,1,1,1,1,1,
1,1,1,1,1,1,1,1,1,1,1,1,1,1,1,1,1,1,1,1,1,1,1,1,1,1,1,1,1,1,1,1,1,1,1,1,
1,1,1,1,1,1,1,1,4),(0.,0.184512097253587),(8.98171729021681,9.48139635699984,
9.98107542378286,10.4807544905659,10.9804335573489,11.4801126241319,11.979791690915,
12.479470757698,12.979149824481,13.478828891264,13.9785079580471,14.4781870248301,
14.9778660916131,15.4775451583961,15.9772242251791,16.4769032919622,16.9765823587452,
17.4762614255282,17.9759404923112,18.4756195590943,18.9752986258773,19.4749776926603,
19.9746567594433,20.4743358262264,20.9740148930094,21.4736939597924,21.9733730265754,
22.4730520933585,22.9727311601415,23.4724102269245,23.9720892937075,24.4717683604905,
24.9714474272736,25.4711264940566,25.9708055608396,26.4704846276226,26.9701636944057,
27.4698427611887,27.9695218279717,28.4692008947547,28.9688799615378,29.4685590283208,
29.9682380951038,30.4679171618868,30.9675962286699,31.4672752954529,31.9669543622359,
32.4666334290189,32.966312495802,33.465991562585,33.965670629368,34.465349696151,
34.965028762934,35.4647078297171,35.9643868965001,36.4640659632831,36.9637450300661,
37.4634240968492,37.9631031636322,38.4627822304152,38.9624612971982,39.4621403639813,
39.9618194307643,40.4614984975473,40.9611775643303,41.4608566311134,41.9605356978964,
42.4602147646794,42.9598938314624,43.4595728982454,43.9592519650285,44.4589310318115,
44.9586100985945,45.4582891653775,45.9579682321606,46.4576472989436,46.9573263657266,
47.4570054325096,47.9566844992927,48.4563635660757,48.9560426328587,49.4557216996417,
49.9554007664248,50.4550798332078,50.9547588999908,51.4544379667738,51.9541170335568,
52.4537961003399,52.9534751671229,53.4531542339059,53.9528333006889,54.452512367472,
54.952191434255,55.451870501038,55.951549567821,56.4512286346041,56.9509077013871,
57.4505867681701,57.9502658349531,58.4499449017362,58.9496239685192,59.9489821020852,
60.9483402356513,61.9476983692173,62.9470565027834,63.9464146363494,64.9457727699155,
65.9451309034815,66.9444890370476,67.9438471706136,68.9432053041797,69.9425634377457,
70.9419215713118,71.9412797048778,72.9406378384438,73.9399959720099,74.9393541055759,
75.938712239142,76.938070372708,77.9374285062741,78.9367866398401,79.9361447734062,
80.9355029069722,81.9348610405383,82.9342191741043,83.9335773076704,84.9329354412364,
85.9322935748025,86.9316517083685,87.9310098419346,88.9303679755006,89.9297261090666,
90.9290842426327,91.9284423761987,92.9278005097648,93.9271586433308,94.9265167768969,
95.9258749104629,96.925233044029,97.924591177595,98.9239493111611,99.9233074447271,
100.922665578293,101.922023711859,102.921381845425,103.920739978991,104.920098112557,
105.919456246123,106.918814379689,107.918172513255,108.917530646822,109.916888780388,
110.916246913954,111.91560504752,112.914963181086,113.914321314652,114.913679448218,
115.913037581784,116.91239571535,117.911753848916,118.911111982482,119.910470116048,
120.909828249614,121.90918638318,122.908544516746,123.907902650312,124.907260783878,
125.906618917444,126.90597705101,127.905335184576,128.904693318142,129.904051451709,
130.903409585275,131.902767718841,132.902125852407,133.901483985973,134.900842119539,
135.900200253105,136.899558386671,137.898916520237,138.898274653803,139.897632787369,
140.896990920935,141.896349054501,142.895707188067,143.895065321633,144.894423455199,
145.893781588765,146.893139722331,147.892497855897,148.891855989463,149.891214123029,
150.890572256596,151.889930390162,152.889288523728,153.888646657294,154.88800479086,
155.887362924426,156.886721057992,157.886079191558,158.885437325124,159.88479545869,
160.884153592256,161.883511725822,162.882869859388,163.882227992954,164.88158612652,
165.880944260086,166.880302393652,167.879660527218,168.879018660784,169.87837679435,
170.877734927916,171.877093061483,172.876451195049,173.875809328615,174.875167462181,
175.874525595747,176.873883729313,177.873241862879,178.872599996445,179.871958130011,
180.871316263577,181.870674397143,182.870032530709,183.869390664275,184.868748797841,
185.868106931407,186.867465064973,187.866823198539,188.866181332105,189.865539465671,
190.864897599237,191.864255732803,192.86361386637,193.862971999936,194.862330133502,
195.861688267068,196.861046400634,197.8604045342,198.859762667766,199.859120801332,
200.858478934898,201.857837068464,202.85719520203,203.856553335596,204.855911469162,
205.855269602728,206.854627736294,207.85398586986,208.853344003426,209.852702136992,
210.852060270558,211.851418404124,212.85077653769,213.850134671257,214.849492804823,
215.848850938389,216.848209071955,217.847567205521,218.846925339087,219.846283472653,
220.845641606219,221.844999739785,222.844357873351,223.843716006917,224.843074140483,
225.842432274049,226.841790407615,227.841148541181,228.840506674747,229.839864808313,
230.839222941879,231.838581075445,232.837939209011,233.837297342577,234.836655476144,
235.83601360971,236.835371743276,237.834729876842,238.834088010408,239.833446143974,
240.83280427754,241.832162411106,242.831520544672,243.830878678238,244.830236811804,
245.82959494537,246.828953078936,247.828311212502,248.827669346068,249.827027479634,
250.8263856132,251.825743746766,252.825101880332,253.824460013898,254.823818147464,
255.82317628103,256.822534414597,257.821892548163,258.821250681729,259.820608815295,
260.819966948861,261.819325082427,262.818683215993,263.818041349559,264.817399483125,
265.816757616691,266.816115750257,267.815473883823,268.814832017389,269.814190150955,
270.813548284521,271.812906418087,272.812264551653,273.811622685219,274.810980818785,
275.810338952351,276.809697085917,277.809055219484,278.80841335305,279.807771486616,
280.807129620182,281.806487753748,282.805845887314,283.80520402088,284.804562154446,
285.803920288012,286.803278421578,287.802636555144,288.80199468871,289.801352822276,
290.800710955842,291.800069089408,292.799427222974,293.79878535654,294.798143490106,
295.797501623672,296.796859757238,297.796217890804,298.795576024371,299.794934157937,
300.794292291503,301.793650425069,302.793008558635,303.792366692201,304.791724825767,
305.791082959333,306.790441092899,307.789799226465,308.789157360031,309.788515493597,
310.787873627163,311.787231760729,312.786589894295,313.785948027861,314.785306161427,
315.784664294993,316.784022428559,317.783380562125,318.782738695691,319.782096829258,
320.781454962824,321.78081309639,322.780171229956,323.779529363522,324.778887497088,
325.778245630654,326.77760376422,327.776961897786,328.776320031352,329.775678164918,
330.775036298484,331.77439443205,332.773752565616,333.773110699182,334.772468832748,
335.771826966314,336.77118509988,337.770543233446,338.769901367012,339.769259500578,
340.768617634145,341.767975767711,342.767333901277,343.766692034843,344.766050168409,
345.765408301975,346.764766435541,347.764124569107,348.763482702673,349.762840836239,
350.762198969805,351.761557103371,352.760915236937,353.760273370503,354.259952437286,
354.759631504069,355.259310570852,355.758989637635,356.258668704418,356.758347771201,
357.258026837984,357.757705904767,358.25738497155,358.757064038333,359.256743105116,
359.756422171899,360.256101238682,360.755780305465,361.255459372248,361.755138439031,
362.254817505815,362.754496572598,363.254175639381,363.753854706164,364.253533772947,
364.75321283973,365.252891906513,365.752570973296,366.252250040079,366.751929106862,
367.251608173645,367.751287240428,368.250966307211,368.750645373994,369.250324440777,
369.75000350756,370.249682574343,370.749361641126,371.249040707909,371.748719774692,
372.248398841475,372.748077908258,373.247756975041,373.747436041824,374.247115108607,
374.74679417539,375.246473242173,375.746152308956,376.245831375739,376.745510442522,
377.245189509305,377.744868576088,378.244547642871,378.744226709654,379.243905776437,
379.74358484322,380.243263910003,380.742942976786,381.242622043569,381.742301110352,
382.241980177135,382.741659243918,383.241338310702,383.741017377485,384.240696444268,
384.740375511051,385.240054577834,385.739733644617,386.2394127114,386.739091778183,
387.238770844966,387.738449911749,388.238128978532,388.737808045315,389.237487112098,
389.737166178881,390.236845245664,390.736524312447,391.23620337923,391.735882446013,
392.235561512796,392.735240579579,393.234919646362,393.734598713145,394.234277779928,
394.733956846711,395.233635913494,395.733314980277,396.23299404706,396.732673113843,
397.232352180626,397.732031247409,398.231710314192,398.731389380975,399.231068447758,
399.730747514541,400.230426581324,400.730105648107,401.22978471489,401.729463781673,
402.229142848456,402.728821915239,403.228500982022,403.728180048805),
 .UNSPECIFIED.);
#18=B_SPLINE_SURFACE_WITH_KNOTS('',3,3,((#60196,#60197,#60198,#60199,#60200,
#60201,#60202,#60203,#60204,#60205,#60206,#60207,#60208,#60209,#60210,#60211,
#60212,#60213,#60214,#60215,#60216,#60217,#60218,#60219,#60220,#60221,#60222,
#60223,#60224,#60225,#60226,#60227,#60228,#60229,#60230,#60231,#60232,#60233,
#60234,#60235,#60236,#60237,#60238,#60239,#60240,#60241,#60242,#60243,#60244,
#60245,#60246,#60247,#60248,#60249,#60250,#60251,#60252,#60253,#60254,#60255,
#60256,#60257,#60258,#60259,#60260,#60261,#60262,#60263,#60264,#60265,#60266,
#60267,#60268,#60269,#60270,#60271,#60272,#60273,#60274,#60275,#60276,#60277,
#60278,#60279,#60280,#60281,#60282,#60283,#60284,#60285,#60286,#60287,#60288,
#60289,#60290,#60291,#60292,#60293,#60294,#60295,#60296,#60297,#60298,#60299,
#60300,#60301,#60302,#60303,#60304,#60305,#60306,#60307,#60308,#60309,#60310,
#60311,#60312,#60313,#60314,#60315,#60316,#60317,#60318,#60319,#60320,#60321,
#60322,#60323,#60324,#60325,#60326,#60327,#60328,#60329,#60330,#60331,#60332,
#60333,#60334,#60335,#60336,#60337,#60338,#60339,#60340,#60341,#60342,#60343,
#60344,#60345,#60346,#60347,#60348,#60349,#60350,#60351,#60352,#60353,#60354,
#60355,#60356,#60357,#60358,#60359,#60360,#60361,#60362,#60363,#60364,#60365,
#60366,#60367,#60368,#60369,#60370,#60371,#60372,#60373,#60374,#60375,#60376,
#60377,#60378,#60379,#60380,#60381,#60382,#60383,#60384,#60385,#60386,#60387,
#60388,#60389,#60390,#60391,#60392,#60393,#60394,#60395,#60396,#60397,#60398,
#60399,#60400,#60401,#60402,#60403,#60404,#60405,#60406,#60407,#60408,#60409,
#60410,#60411,#60412,#60413,#60414,#60415,#60416,#60417,#60418,#60419,#60420,
#60421,#60422,#60423,#60424,#60425,#60426,#60427,#60428,#60429,#60430,#60431,
#60432,#60433,#60434,#60435,#60436,#60437,#60438,#60439,#60440,#60441,#60442,
#60443,#60444,#60445,#60446,#60447,#60448,#60449,#60450,#60451,#60452,#60453,
#60454,#60455,#60456,#60457,#60458,#60459,#60460,#60461,#60462,#60463,#60464,
#60465,#60466,#60467,#60468,#60469,#60470,#60471,#60472,#60473,#60474,#60475,
#60476,#60477,#60478,#60479,#60480,#60481,#60482,#60483,#60484,#60485,#60486,
#60487,#60488,#60489,#60490,#60491,#60492,#60493,#60494,#60495,#60496,#60497,
#60498,#60499,#60500,#60501,#60502,#60503,#60504,#60505,#60506,#60507,#60508,
#60509,#60510,#60511,#60512,#60513,#60514,#60515,#60516,#60517,#60518,#60519,
#60520,#60521,#60522,#60523,#60524,#60525,#60526,#60527,#60528,#60529,#60530,
#60531,#60532,#60533,#60534,#60535,#60536,#60537,#60538,#60539,#60540,#60541,
#60542,#60543,#60544,#60545,#60546,#60547,#60548,#60549,#60550,#60551,#60552,
#60553,#60554,#60555,#60556,#60557,#60558,#60559,#60560,#60561,#60562,#60563,
#60564,#60565,#60566,#60567,#60568,#60569,#60570,#60571,#60572,#60573,#60574,
#60575,#60576,#60577,#60578,#60579,#60580,#60581,#60582,#60583,#60584,#60585,
#60586,#60587,#60588,#60589,#60590,#60591,#60592,#60593,#60594,#60595,#60596,
#60597,#60598,#60599,#60600,#60601,#60602,#60603,#60604,#60605,#60606,#60607,
#60608,#60609,#60610,#60611,#60612,#60613,#60614,#60615,#60616,#60617,#60618,
#60619,#60620,#60621,#60622,#60623,#60624,#60625,#60626,#60627,#60628,#60629,
#60630,#60631,#60632,#60633,#60634,#60635,#60636,#60637,#60638,#60639,#60640,
#60641,#60642,#60643,#60644,#60645,#60646,#60647,#60648,#60649,#60650,#60651,
#60652,#60653,#60654,#60655,#60656,#60657,#60658,#60659,#60660,#60661,#60662,
#60663,#60664,#60665,#60666,#60667,#60668,#60669,#60670,#60671,#60672,#60673,
#60674,#60675,#60676,#60677,#60678,#60679,#60680,#60681,#60682,#60683,#60684,
#60685,#60686,#60687,#60688,#60689,#60690,#60691,#60692,#60693),(#60694,
#60695,#60696,#60697,#60698,#60699,#60700,#60701,#60702,#60703,#60704,#60705,
#60706,#60707,#60708,#60709,#60710,#60711,#60712,#60713,#60714,#60715,#60716,
#60717,#60718,#60719,#60720,#60721,#60722,#60723,#60724,#60725,#60726,#60727,
#60728,#60729,#60730,#60731,#60732,#60733,#60734,#60735,#60736,#60737,#60738,
#60739,#60740,#60741,#60742,#60743,#60744,#60745,#60746,#60747,#60748,#60749,
#60750,#60751,#60752,#60753,#60754,#60755,#60756,#60757,#60758,#60759,#60760,
#60761,#60762,#60763,#60764,#60765,#60766,#60767,#60768,#60769,#60770,#60771,
#60772,#60773,#60774,#60775,#60776,#60777,#60778,#60779,#60780,#60781,#60782,
#60783,#60784,#60785,#60786,#60787,#60788,#60789,#60790,#60791,#60792,#60793,
#60794,#60795,#60796,#60797,#60798,#60799,#60800,#60801,#60802,#60803,#60804,
#60805,#60806,#60807,#60808,#60809,#60810,#60811,#60812,#60813,#60814,#60815,
#60816,#60817,#60818,#60819,#60820,#60821,#60822,#60823,#60824,#60825,#60826,
#60827,#60828,#60829,#60830,#60831,#60832,#60833,#60834,#60835,#60836,#60837,
#60838,#60839,#60840,#60841,#60842,#60843,#60844,#60845,#60846,#60847,#60848,
#60849,#60850,#60851,#60852,#60853,#60854,#60855,#60856,#60857,#60858,#60859,
#60860,#60861,#60862,#60863,#60864,#60865,#60866,#60867,#60868,#60869,#60870,
#60871,#60872,#60873,#60874,#60875,#60876,#60877,#60878,#60879,#60880,#60881,
#60882,#60883,#60884,#60885,#60886,#60887,#60888,#60889,#60890,#60891,#60892,
#60893,#60894,#60895,#60896,#60897,#60898,#60899,#60900,#60901,#60902,#60903,
#60904,#60905,#60906,#60907,#60908,#60909,#60910,#60911,#60912,#60913,#60914,
#60915,#60916,#60917,#60918,#60919,#60920,#60921,#60922,#60923,#60924,#60925,
#60926,#60927,#60928,#60929,#60930,#60931,#60932,#60933,#60934,#60935,#60936,
#60937,#60938,#60939,#60940,#60941,#60942,#60943,#60944,#60945,#60946,#60947,
#60948,#60949,#60950,#60951,#60952,#60953,#60954,#60955,#60956,#60957,#60958,
#60959,#60960,#60961,#60962,#60963,#60964,#60965,#60966,#60967,#60968,#60969,
#60970,#60971,#60972,#60973,#60974,#60975,#60976,#60977,#60978,#60979,#60980,
#60981,#60982,#60983,#60984,#60985,#60986,#60987,#60988,#60989,#60990,#60991,
#60992,#60993,#60994,#60995,#60996,#60997,#60998,#60999,#61000,#61001,#61002,
#61003,#61004,#61005,#61006,#61007,#61008,#61009,#61010,#61011,#61012,#61013,
#61014,#61015,#61016,#61017,#61018,#61019,#61020,#61021,#61022,#61023,#61024,
#61025,#61026,#61027,#61028,#61029,#61030,#61031,#61032,#61033,#61034,#61035,
#61036,#61037,#61038,#61039,#61040,#61041,#61042,#61043,#61044,#61045,#61046,
#61047,#61048,#61049,#61050,#61051,#61052,#61053,#61054,#61055,#61056,#61057,
#61058,#61059,#61060,#61061,#61062,#61063,#61064,#61065,#61066,#61067,#61068,
#61069,#61070,#61071,#61072,#61073,#61074,#61075,#61076,#61077,#61078,#61079,
#61080,#61081,#61082,#61083,#61084,#61085,#61086,#61087,#61088,#61089,#61090,
#61091,#61092,#61093,#61094,#61095,#61096,#61097,#61098,#61099,#61100,#61101,
#61102,#61103,#61104,#61105,#61106,#61107,#61108,#61109,#61110,#61111,#61112,
#61113,#61114,#61115,#61116,#61117,#61118,#61119,#61120,#61121,#61122,#61123,
#61124,#61125,#61126,#61127,#61128,#61129,#61130,#61131,#61132,#61133,#61134,
#61135,#61136,#61137,#61138,#61139,#61140,#61141,#61142,#61143,#61144,#61145,
#61146,#61147,#61148,#61149,#61150,#61151,#61152,#61153,#61154,#61155,#61156,
#61157,#61158,#61159,#61160,#61161,#61162,#61163,#61164,#61165,#61166,#61167,
#61168,#61169,#61170,#61171,#61172,#61173,#61174,#61175,#61176,#61177,#61178,
#61179,#61180,#61181,#61182,#61183,#61184,#61185,#61186,#61187,#61188,#61189,
#61190,#61191),(#61192,#61193,#61194,#61195,#61196,#61197,#61198,#61199,
#61200,#61201,#61202,#61203,#61204,#61205,#61206,#61207,#61208,#61209,#61210,
#61211,#61212,#61213,#61214,#61215,#61216,#61217,#61218,#61219,#61220,#61221,
#61222,#61223,#61224,#61225,#61226,#61227,#61228,#61229,#61230,#61231,#61232,
#61233,#61234,#61235,#61236,#61237,#61238,#61239,#61240,#61241,#61242,#61243,
#61244,#61245,#61246,#61247,#61248,#61249,#61250,#61251,#61252,#61253,#61254,
#61255,#61256,#61257,#61258,#61259,#61260,#61261,#61262,#61263,#61264,#61265,
#61266,#61267,#61268,#61269,#61270,#61271,#61272,#61273,#61274,#61275,#61276,
#61277,#61278,#61279,#61280,#61281,#61282,#61283,#61284,#61285,#61286,#61287,
#61288,#61289,#61290,#61291,#61292,#61293,#61294,#61295,#61296,#61297,#61298,
#61299,#61300,#61301,#61302,#61303,#61304,#61305,#61306,#61307,#61308,#61309,
#61310,#61311,#61312,#61313,#61314,#61315,#61316,#61317,#61318,#61319,#61320,
#61321,#61322,#61323,#61324,#61325,#61326,#61327,#61328,#61329,#61330,#61331,
#61332,#61333,#61334,#61335,#61336,#61337,#61338,#61339,#61340,#61341,#61342,
#61343,#61344,#61345,#61346,#61347,#61348,#61349,#61350,#61351,#61352,#61353,
#61354,#61355,#61356,#61357,#61358,#61359,#61360,#61361,#61362,#61363,#61364,
#61365,#61366,#61367,#61368,#61369,#61370,#61371,#61372,#61373,#61374,#61375,
#61376,#61377,#61378,#61379,#61380,#61381,#61382,#61383,#61384,#61385,#61386,
#61387,#61388,#61389,#61390,#61391,#61392,#61393,#61394,#61395,#61396,#61397,
#61398,#61399,#61400,#61401,#61402,#61403,#61404,#61405,#61406,#61407,#61408,
#61409,#61410,#61411,#61412,#61413,#61414,#61415,#61416,#61417,#61418,#61419,
#61420,#61421,#61422,#61423,#61424,#61425,#61426,#61427,#61428,#61429,#61430,
#61431,#61432,#61433,#61434,#61435,#61436,#61437,#61438,#61439,#61440,#61441,
#61442,#61443,#61444,#61445,#61446,#61447,#61448,#61449,#61450,#61451,#61452,
#61453,#61454,#61455,#61456,#61457,#61458,#61459,#61460,#61461,#61462,#61463,
#61464,#61465,#61466,#61467,#61468,#61469,#61470,#61471,#61472,#61473,#61474,
#61475,#61476,#61477,#61478,#61479,#61480,#61481,#61482,#61483,#61484,#61485,
#61486,#61487,#61488,#61489,#61490,#61491,#61492,#61493,#61494,#61495,#61496,
#61497,#61498,#61499,#61500,#61501,#61502,#61503,#61504,#61505,#61506,#61507,
#61508,#61509,#61510,#61511,#61512,#61513,#61514,#61515,#61516,#61517,#61518,
#61519,#61520,#61521,#61522,#61523,#61524,#61525,#61526,#61527,#61528,#61529,
#61530,#61531,#61532,#61533,#61534,#61535,#61536,#61537,#61538,#61539,#61540,
#61541,#61542,#61543,#61544,#61545,#61546,#61547,#61548,#61549,#61550,#61551,
#61552,#61553,#61554,#61555,#61556,#61557,#61558,#61559,#61560,#61561,#61562,
#61563,#61564,#61565,#61566,#61567,#61568,#61569,#61570,#61571,#61572,#61573,
#61574,#61575,#61576,#61577,#61578,#61579,#61580,#61581,#61582,#61583,#61584,
#61585,#61586,#61587,#61588,#61589,#61590,#61591,#61592,#61593,#61594,#61595,
#61596,#61597,#61598,#61599,#61600,#61601,#61602,#61603,#61604,#61605,#61606,
#61607,#61608,#61609,#61610,#61611,#61612,#61613,#61614,#61615,#61616,#61617,
#61618,#61619,#61620,#61621,#61622,#61623,#61624,#61625,#61626,#61627,#61628,
#61629,#61630,#61631,#61632,#61633,#61634,#61635,#61636,#61637,#61638,#61639,
#61640,#61641,#61642,#61643,#61644,#61645,#61646,#61647,#61648,#61649,#61650,
#61651,#61652,#61653,#61654,#61655,#61656,#61657,#61658,#61659,#61660,#61661,
#61662,#61663,#61664,#61665,#61666,#61667,#61668,#61669,#61670,#61671,#61672,
#61673,#61674,#61675,#61676,#61677,#61678,#61679,#61680,#61681,#61682,#61683,
#61684,#61685,#61686,#61687,#61688,#61689),(#61690,#61691,#61692,#61693,
#61694,#61695,#61696,#61697,#61698,#61699,#61700,#61701,#61702,#61703,#61704,
#61705,#61706,#61707,#61708,#61709,#61710,#61711,#61712,#61713,#61714,#61715,
#61716,#61717,#61718,#61719,#61720,#61721,#61722,#61723,#61724,#61725,#61726,
#61727,#61728,#61729,#61730,#61731,#61732,#61733,#61734,#61735,#61736,#61737,
#61738,#61739,#61740,#61741,#61742,#61743,#61744,#61745,#61746,#61747,#61748,
#61749,#61750,#61751,#61752,#61753,#61754,#61755,#61756,#61757,#61758,#61759,
#61760,#61761,#61762,#61763,#61764,#61765,#61766,#61767,#61768,#61769,#61770,
#61771,#61772,#61773,#61774,#61775,#61776,#61777,#61778,#61779,#61780,#61781,
#61782,#61783,#61784,#61785,#61786,#61787,#61788,#61789,#61790,#61791,#61792,
#61793,#61794,#61795,#61796,#61797,#61798,#61799,#61800,#61801,#61802,#61803,
#61804,#61805,#61806,#61807,#61808,#61809,#61810,#61811,#61812,#61813,#61814,
#61815,#61816,#61817,#61818,#61819,#61820,#61821,#61822,#61823,#61824,#61825,
#61826,#61827,#61828,#61829,#61830,#61831,#61832,#61833,#61834,#61835,#61836,
#61837,#61838,#61839,#61840,#61841,#61842,#61843,#61844,#61845,#61846,#61847,
#61848,#61849,#61850,#61851,#61852,#61853,#61854,#61855,#61856,#61857,#61858,
#61859,#61860,#61861,#61862,#61863,#61864,#61865,#61866,#61867,#61868,#61869,
#61870,#61871,#61872,#61873,#61874,#61875,#61876,#61877,#61878,#61879,#61880,
#61881,#61882,#61883,#61884,#61885,#61886,#61887,#61888,#61889,#61890,#61891,
#61892,#61893,#61894,#61895,#61896,#61897,#61898,#61899,#61900,#61901,#61902,
#61903,#61904,#61905,#61906,#61907,#61908,#61909,#61910,#61911,#61912,#61913,
#61914,#61915,#61916,#61917,#61918,#61919,#61920,#61921,#61922,#61923,#61924,
#61925,#61926,#61927,#61928,#61929,#61930,#61931,#61932,#61933,#61934,#61935,
#61936,#61937,#61938,#61939,#61940,#61941,#61942,#61943,#61944,#61945,#61946,
#61947,#61948,#61949,#61950,#61951,#61952,#61953,#61954,#61955,#61956,#61957,
#61958,#61959,#61960,#61961,#61962,#61963,#61964,#61965,#61966,#61967,#61968,
#61969,#61970,#61971,#61972,#61973,#61974,#61975,#61976,#61977,#61978,#61979,
#61980,#61981,#61982,#61983,#61984,#61985,#61986,#61987,#61988,#61989,#61990,
#61991,#61992,#61993,#61994,#61995,#61996,#61997,#61998,#61999,#62000,#62001,
#62002,#62003,#62004,#62005,#62006,#62007,#62008,#62009,#62010,#62011,#62012,
#62013,#62014,#62015,#62016,#62017,#62018,#62019,#62020,#62021,#62022,#62023,
#62024,#62025,#62026,#62027,#62028,#62029,#62030,#62031,#62032,#62033,#62034,
#62035,#62036,#62037,#62038,#62039,#62040,#62041,#62042,#62043,#62044,#62045,
#62046,#62047,#62048,#62049,#62050,#62051,#62052,#62053,#62054,#62055,#62056,
#62057,#62058,#62059,#62060,#62061,#62062,#62063,#62064,#62065,#62066,#62067,
#62068,#62069,#62070,#62071,#62072,#62073,#62074,#62075,#62076,#62077,#62078,
#62079,#62080,#62081,#62082,#62083,#62084,#62085,#62086,#62087,#62088,#62089,
#62090,#62091,#62092,#62093,#62094,#62095,#62096,#62097,#62098,#62099,#62100,
#62101,#62102,#62103,#62104,#62105,#62106,#62107,#62108,#62109,#62110,#62111,
#62112,#62113,#62114,#62115,#62116,#62117,#62118,#62119,#62120,#62121,#62122,
#62123,#62124,#62125,#62126,#62127,#62128,#62129,#62130,#62131,#62132,#62133,
#62134,#62135,#62136,#62137,#62138,#62139,#62140,#62141,#62142,#62143,#62144,
#62145,#62146,#62147,#62148,#62149,#62150,#62151,#62152,#62153,#62154,#62155,
#62156,#62157,#62158,#62159,#62160,#62161,#62162,#62163,#62164,#62165,#62166,
#62167,#62168,#62169,#62170,#62171,#62172,#62173,#62174,#62175,#62176,#62177,
#62178,#62179,#62180,#62181,#62182,#62183,#62184,#62185,#62186,#62187)),
 .UNSPECIFIED.,.F.,.F.,.F.,(4,4),(4,1,1,1,1,1,1,1,1,1,1,1,1,1,1,1,1,1,1,
1,1,1,1,1,1,1,1,1,1,1,1,1,1,1,1,1,1,1,1,1,1,1,1,1,1,1,1,1,1,1,1,1,1,1,1,
1,1,1,1,1,1,1,1,1,1,1,1,1,1,1,1,1,1,1,1,1,1,1,1,1,1,1,1,1,1,1,1,1,1,1,1,
1,1,1,1,1,1,1,1,1,1,1,1,1,1,1,1,1,1,1,1,1,1,1,1,1,1,1,1,1,1,1,1,1,1,1,1,
1,1,1,1,1,1,1,1,1,1,1,1,1,1,1,1,1,1,1,1,1,1,1,1,1,1,1,1,1,1,1,1,1,1,1,1,
1,1,1,1,1,1,1,1,1,1,1,1,1,1,1,1,1,1,1,1,1,1,1,1,1,1,1,1,1,1,1,1,1,1,1,1,
1,1,1,1,1,1,1,1,1,1,1,1,1,1,1,1,1,1,1,1,1,1,1,1,1,1,1,1,1,1,1,1,1,1,1,1,
1,1,1,1,1,1,1,1,1,1,1,1,1,1,1,1,1,1,1,1,1,1,1,1,1,1,1,1,1,1,1,1,1,1,1,1,
1,1,1,1,1,1,1,1,1,1,1,1,1,1,1,1,1,1,1,1,1,1,1,1,1,1,1,1,1,1,1,1,1,1,1,1,
1,1,1,1,1,1,1,1,1,1,1,1,1,1,1,1,1,1,1,1,1,1,1,1,1,1,1,1,1,1,1,1,1,1,1,1,
1,1,1,1,1,1,1,1,1,1,1,1,1,1,1,1,1,1,1,1,1,1,1,1,1,1,1,1,1,1,1,1,1,1,1,1,
1,1,1,1,1,1,1,1,1,1,1,1,1,1,1,1,1,1,1,1,1,1,1,1,1,1,1,1,1,1,1,1,1,1,1,1,
1,1,1,1,1,1,1,1,1,1,1,1,1,1,1,1,1,1,1,1,1,1,1,1,1,1,1,1,1,1,1,1,1,1,1,1,
1,1,1,1,1,1,1,1,1,1,1,1,1,1,1,1,1,1,1,1,1,1,1,1,1,1,1,1,1,1,1,1,1,1,1,1,
1,1,1,1,1,1,1,1,4),(0.,0.184512097253587),(12.0092477762453,12.5089268430284,
13.0086059098114,13.5082849765944,14.0079640433774,14.5076431101605,15.0073221769435,
15.5070012437265,16.0066803105095,16.5063593772925,17.0060384440756,17.5057175108586,
18.0053965776416,18.5050756444246,19.0047547112077,19.5044337779907,20.0041128447737,
20.5037919115567,21.0034709783398,21.5031500451228,22.0028291119058,22.5025081786888,
23.0021872454719,23.5018663122549,24.0015453790379,24.5012244458209,25.0009035126039,
25.500582579387,26.00026164617,26.499940712953,26.999619779736,27.4992988465191,
27.9989779133021,28.4986569800851,28.9983360468681,29.4980151136512,29.9976941804342,
30.4973732472172,30.9970523140002,31.4967313807832,31.9964104475663,32.4960895143493,
32.9957685811323,33.4954476479153,33.9951267146984,34.4948057814814,34.9944848482644,
35.4941639150474,35.9938429818305,36.4935220486135,36.9932011153965,37.4928801821795,
37.9925592489626,38.4922383157456,38.9919173825286,39.4915964493116,39.9912755160946,
40.4909545828777,40.9906336496607,41.4903127164437,41.9899917832267,42.4896708500098,
42.9893499167928,43.4890289835758,43.9887080503588,44.4883871171419,44.9880661839249,
45.4877452507079,45.9874243174909,46.4871033842739,46.986782451057,47.48646151784,
47.986140584623,48.485819651406,48.9854987181891,49.4851777849721,49.9848568517551,
50.4845359185381,50.9842149853212,51.4838940521042,51.9835731188872,52.4832521856702,
52.9829312524532,53.4826103192363,53.9822893860193,54.4819684528023,54.9816475195853,
55.4813265863684,55.9810056531514,56.4806847199344,56.9803637867174,57.4800428535005,
57.9797219202835,58.4794009870665,58.9790800538495,59.4787591206325,59.9784381874156,
60.4781172541986,60.9777963209816,61.4774753877646,61.9771544545477,62.9765125881137,
63.9758707216798,64.9752288552458,65.9745869888119,66.9739451223779,67.9733032559439,
68.97266138951,69.972019523076,70.9713776566421,71.9707357902081,72.9700939237742,
73.9694520573402,74.9688101909063,75.9681683244723,76.9675264580384,77.9668845916044,
78.9662427251705,79.9656008587365,80.9649589923026,81.9643171258686,82.9636752594347,
83.9630333930007,84.9623915265667,85.9617496601328,86.9611077936988,87.9604659272649,
88.9598240608309,89.959182194397,90.958540327963,91.9578984615291,92.9572565950951,
93.9566147286612,94.9559728622272,95.9553309957932,96.9546891293593,97.9540472629253,
98.9534053964914,99.9527635300574,100.952121663623,101.95147979719,102.950837930756,
103.950196064322,104.949554197888,105.948912331454,106.94827046502,107.947628598586,
108.946986732152,109.946344865718,110.945702999284,111.94506113285,112.944419266416,
113.943777399982,114.943135533548,115.942493667114,116.94185180068,117.941209934246,
118.940568067812,119.939926201378,120.939284334944,121.93864246851,122.938000602077,
123.937358735643,124.936716869209,125.936075002775,126.935433136341,127.934791269907,
128.934149403473,129.933507537039,130.932865670605,131.932223804171,132.931581937737,
133.930940071303,134.930298204869,135.929656338435,136.929014472001,137.928372605567,
138.927730739133,139.927088872699,140.926447006265,141.925805139831,142.925163273397,
143.924521406963,144.92387954053,145.923237674096,146.922595807662,147.921953941228,
148.921312074794,149.92067020836,150.920028341926,151.919386475492,152.918744609058,
153.918102742624,154.91746087619,155.916819009756,156.916177143322,157.915535276888,
158.914893410454,159.91425154402,160.913609677586,161.912967811152,162.912325944718,
163.911684078284,164.91104221185,165.910400345416,166.909758478983,167.909116612549,
168.908474746115,169.907832879681,170.907191013247,171.906549146813,172.905907280379,
173.905265413945,174.904623547511,175.903981681077,176.903339814643,177.902697948209,
178.902056081775,179.901414215341,180.900772348907,181.900130482473,182.899488616039,
183.898846749605,184.898204883171,185.897563016737,186.896921150303,187.89627928387,
188.895637417436,189.894995551002,190.894353684568,191.893711818134,192.8930699517,
193.892428085266,194.891786218832,195.891144352398,196.890502485964,197.88986061953,
198.889218753096,199.888576886662,200.887935020228,201.887293153794,202.88665128736,
203.886009420926,204.885367554492,205.884725688058,206.884083821624,207.88344195519,
208.882800088756,209.882158222323,210.881516355889,211.880874489455,212.880232623021,
213.879590756587,214.878948890153,215.878307023719,216.877665157285,217.877023290851,
218.876381424417,219.875739557983,220.875097691549,221.874455825115,222.873813958681,
223.873172092247,224.872530225813,225.871888359379,226.871246492945,227.870604626511,
228.869962760077,229.869320893643,230.86867902721,231.868037160776,232.867395294342,
233.866753427908,234.866111561474,235.86546969504,236.864827828606,237.864185962172,
238.863544095738,239.862902229304,240.86226036287,241.861618496436,242.860976630002,
243.860334763568,244.859692897134,245.8590510307,246.858409164266,247.857767297832,
248.857125431398,249.856483564964,250.85584169853,251.855199832097,252.854557965663,
253.853916099229,254.853274232795,255.852632366361,256.851990499927,257.851348633493,
258.850706767059,259.850064900625,260.849423034191,261.848781167757,262.848139301323,
263.847497434889,264.846855568455,265.846213702021,266.845571835587,267.844929969153,
268.844288102719,269.843646236285,270.843004369851,271.842362503417,272.841720636983,
273.84107877055,274.840436904116,275.839795037682,276.839153171248,277.838511304814,
278.83786943838,279.837227571946,280.836585705512,281.835943839078,282.835301972644,
283.83466010621,284.834018239776,285.833376373342,286.832734506908,287.832092640474,
288.83145077404,289.830808907606,290.830167041172,291.829525174738,292.828883308304,
293.82824144187,294.827599575437,295.826957709003,296.826315842569,297.825673976135,
298.825032109701,299.824390243267,300.823748376833,301.823106510399,302.822464643965,
303.821822777531,304.821180911097,305.820539044663,306.819897178229,307.819255311795,
308.818613445361,309.817971578927,310.817329712493,311.816687846059,312.816045979625,
313.815404113191,314.814762246757,315.814120380323,316.81347851389,317.812836647456,
318.812194781022,319.811552914588,320.810911048154,321.81026918172,322.809627315286,
323.808985448852,324.808343582418,325.807701715984,326.80705984955,327.806417983116,
328.805776116682,329.805134250248,330.804492383814,331.80385051738,332.803208650946,
333.802566784512,334.801924918078,335.801283051644,336.80064118521,337.799999318776,
338.799357452343,339.798715585909,340.798073719475,341.797431853041,342.796789986607,
343.796148120173,344.795506253739,345.794864387305,346.794222520871,347.793580654437,
348.792938788003,349.792296921569,350.791655055135,351.791013188701,352.790371322267,
353.789729455833,354.789087589399,355.788445722965,356.787803856531,357.287482923314,
357.787161990097,358.28684105688,358.786520123663,359.286199190446,359.78587825723,
360.285557324013,360.785236390796,361.284915457579,361.784594524362,362.284273591145,
362.783952657928,363.283631724711,363.783310791494,364.282989858277,364.78266892506,
365.282347991843,365.782027058626,366.281706125409,366.781385192192,367.281064258975,
367.780743325758,368.280422392541,368.780101459324,369.279780526107,369.77945959289,
370.279138659673,370.778817726456,371.278496793239,371.778175860022,372.277854926805,
372.777533993588,373.277213060371,373.776892127154,374.276571193937,374.77625026072,
375.275929327503,375.775608394286,376.275287461069,376.774966527852,377.274645594635,
377.774324661418,378.274003728201,378.773682794984,379.273361861767,379.77304092855,
380.272719995333,380.772399062117,381.2720781289,381.771757195683,382.271436262466,
382.771115329249,383.270794396032,383.770473462815,384.270152529598,384.769831596381,
385.269510663164,385.769189729947,386.26886879673,386.768547863513,387.268226930296,
387.767905997079,388.267585063862,388.767264130645,389.266943197428,389.766622264211,
390.266301330994,390.765980397777,391.26565946456,391.765338531343,392.265017598126,
392.764696664909,393.264375731692,393.764054798475,394.263733865258,394.763412932041,
395.263091998824,395.762771065607,396.26245013239,396.762129199173,397.261808265956,
397.761487332739,398.261166399522,398.760845466305,399.260524533088,399.760203599871,
400.259882666654,400.759561733437,401.25924080022,401.758919867003,402.258598933787,
402.75827800057,403.257957067353,403.757636134136,404.257315200919,404.756994267702,
405.256673334485,405.756352401268,406.256031468051,406.755710534834),
 .UNSPECIFIED.);
#19=ORIENTED_CLOSED_SHELL('',*,#23007,.F.);
#20=ORIENTED_CLOSED_SHELL('',*,#23011,.F.);
#21=ORIENTED_CLOSED_SHELL('',*,#23013,.F.);
#22=ORIENTED_CLOSED_SHELL('',*,#23024,.F.);
#23=ORIENTED_CLOSED_SHELL('',*,#23059,.F.);
#24=ORIENTED_CLOSED_SHELL('',*,#23068,.F.);
#25=ORIENTED_CLOSED_SHELL('',*,#23072,.F.);
#26=ORIENTED_CLOSED_SHELL('',*,#23074,.F.);
#27=ORIENTED_CLOSED_SHELL('',*,#23085,.F.);
#28=BREP_WITH_VOIDS('Body1',#23008,(#19));
#29=BREP_WITH_VOIDS('Body1',#23010,(#20));
#30=BREP_WITH_VOIDS('Body1',#23012,(#21));
#31=BREP_WITH_VOIDS('Body1',#23023,(#22));
#32=BREP_WITH_VOIDS('Body1',#23060,(#23));
#33=BREP_WITH_VOIDS('Body1',#23069,(#24));
#34=BREP_WITH_VOIDS('Body1',#23071,(#25));
#35=BREP_WITH_VOIDS('Body1',#23073,(#26));
#36=BREP_WITH_VOIDS('Body1',#23084,(#27));
#37=ITEM_DEFINED_TRANSFORMATION($,$,#24286,#24408);
#38=ITEM_DEFINED_TRANSFORMATION($,$,#24306,#24409);
#39=ITEM_DEFINED_TRANSFORMATION($,$,#24326,#24410);
#40=ITEM_DEFINED_TRANSFORMATION($,$,#24341,#24411);
#41=ITEM_DEFINED_TRANSFORMATION($,$,#24391,#24412);
#42=ITEM_DEFINED_TRANSFORMATION($,$,#24414,#24542);
#43=ITEM_DEFINED_TRANSFORMATION($,$,#24434,#24543);
#44=ITEM_DEFINED_TRANSFORMATION($,$,#24454,#24544);
#45=ITEM_DEFINED_TRANSFORMATION($,$,#24471,#24545);
#46=ITEM_DEFINED_TRANSFORMATION($,$,#24525,#24546);
#47=ITEM_DEFINED_TRANSFORMATION($,$,#24649,#24710);
#48=ITEM_DEFINED_TRANSFORMATION($,$,#24688,#24711);
#49=ITEM_DEFINED_TRANSFORMATION($,$,#24699,#24712);
#50=ITEM_DEFINED_TRANSFORMATION($,$,#24548,#24849);
#51=ITEM_DEFINED_TRANSFORMATION($,$,#24567,#24850);
#52=ITEM_DEFINED_TRANSFORMATION($,$,#24610,#24851);
#53=ITEM_DEFINED_TRANSFORMATION($,$,#24648,#24852);
#54=ITEM_DEFINED_TRANSFORMATION($,$,#24713,#24853);
#55=ITEM_DEFINED_TRANSFORMATION($,$,#24724,#24854);
#56=ITEM_DEFINED_TRANSFORMATION($,$,#24713,#24855);
#57=ITEM_DEFINED_TRANSFORMATION($,$,#24724,#24856);
#58=ITEM_DEFINED_TRANSFORMATION($,$,#24713,#24857);
#59=ITEM_DEFINED_TRANSFORMATION($,$,#24724,#24858);
#60=ITEM_DEFINED_TRANSFORMATION($,$,#24713,#24859);
#61=ITEM_DEFINED_TRANSFORMATION($,$,#24724,#24860);
#62=ITEM_DEFINED_TRANSFORMATION($,$,#24752,#24861);
#63=ITEM_DEFINED_TRANSFORMATION($,$,#24797,#24862);
#64=ITEM_DEFINED_TRANSFORMATION($,$,#24797,#24863);
#65=ITEM_DEFINED_TRANSFORMATION($,$,#24797,#24864);
#66=ITEM_DEFINED_TRANSFORMATION($,$,#24823,#24865);
#67=ITEM_DEFINED_TRANSFORMATION($,$,#24823,#24866);
#68=ITEM_DEFINED_TRANSFORMATION($,$,#24823,#24867);
#69=ITEM_DEFINED_TRANSFORMATION($,$,#24823,#24868);
#70=ITEM_DEFINED_TRANSFORMATION($,$,#24003,#25153);
#71=ITEM_DEFINED_TRANSFORMATION($,$,#24040,#25154);
#72=ITEM_DEFINED_TRANSFORMATION($,$,#24047,#25155);
#73=ITEM_DEFINED_TRANSFORMATION($,$,#24054,#25156);
#74=ITEM_DEFINED_TRANSFORMATION($,$,#24107,#25157);
#75=ITEM_DEFINED_TRANSFORMATION($,$,#24138,#25158);
#76=ITEM_DEFINED_TRANSFORMATION($,$,#24160,#25159);
#77=ITEM_DEFINED_TRANSFORMATION($,$,#24191,#25160);
#78=ITEM_DEFINED_TRANSFORMATION($,$,#24214,#25161);
#79=ITEM_DEFINED_TRANSFORMATION($,$,#24228,#25162);
#80=ITEM_DEFINED_TRANSFORMATION($,$,#24823,#25163);
#81=ITEM_DEFINED_TRANSFORMATION($,$,#24823,#25164);
#82=ITEM_DEFINED_TRANSFORMATION($,$,#24823,#25165);
#83=ITEM_DEFINED_TRANSFORMATION($,$,#24823,#25166);
#84=ITEM_DEFINED_TRANSFORMATION($,$,#24242,#25167);
#85=ITEM_DEFINED_TRANSFORMATION($,$,#24797,#25168);
#86=ITEM_DEFINED_TRANSFORMATION($,$,#24797,#25169);
#87=ITEM_DEFINED_TRANSFORMATION($,$,#24797,#25170);
#88=ITEM_DEFINED_TRANSFORMATION($,$,#24797,#25171);
#89=ITEM_DEFINED_TRANSFORMATION($,$,#24823,#25172);
#90=ITEM_DEFINED_TRANSFORMATION($,$,#24823,#25173);
#91=ITEM_DEFINED_TRANSFORMATION($,$,#24285,#25174);
#92=ITEM_DEFINED_TRANSFORMATION($,$,#24797,#25175);
#93=ITEM_DEFINED_TRANSFORMATION($,$,#24797,#25176);
#94=ITEM_DEFINED_TRANSFORMATION($,$,#24797,#25177);
#95=ITEM_DEFINED_TRANSFORMATION($,$,#25127,#25178);
#96=ITEM_DEFINED_TRANSFORMATION($,$,#25127,#25179);
#97=ITEM_DEFINED_TRANSFORMATION($,$,#24413,#25180);
#98=ITEM_DEFINED_TRANSFORMATION($,$,#24797,#25181);
#99=ITEM_DEFINED_TRANSFORMATION($,$,#24797,#25182);
#100=ITEM_DEFINED_TRANSFORMATION($,$,#24797,#25183);
#101=ITEM_DEFINED_TRANSFORMATION($,$,#24823,#25184);
#102=ITEM_DEFINED_TRANSFORMATION($,$,#24823,#25185);
#103=ITEM_DEFINED_TRANSFORMATION($,$,#24870,#25186);
#104=ITEM_DEFINED_TRANSFORMATION($,$,#25025,#25187);
#105=ITEM_DEFINED_TRANSFORMATION($,$,#25034,#25188);
#106=ITEM_DEFINED_TRANSFORMATION($,$,#25048,#25189);
#107=ITEM_DEFINED_TRANSFORMATION($,$,#25072,#25190);
#108=ITEM_DEFINED_TRANSFORMATION($,$,#25081,#25191);
#109=ITEM_DEFINED_TRANSFORMATION($,$,#25090,#25192);
#110=ITEM_DEFINED_TRANSFORMATION($,$,#25101,#25193);
#111=ITEM_DEFINED_TRANSFORMATION($,$,#25101,#25194);
#112=ITEM_DEFINED_TRANSFORMATION($,$,#25118,#25195);
#113=ITEM_DEFINED_TRANSFORMATION($,$,#25127,#25196);
#114=ITEM_DEFINED_TRANSFORMATION($,$,#24002,#25197);
#115=ITEM_DEFINED_TRANSFORMATION($,$,#24547,#25198);
#116=ITEM_DEFINED_TRANSFORMATION($,$,#24869,#25199);
#117=ITEM_DEFINED_TRANSFORMATION($,$,#25531,#25653);
#118=ITEM_DEFINED_TRANSFORMATION($,$,#25551,#25654);
#119=ITEM_DEFINED_TRANSFORMATION($,$,#25571,#25655);
#120=ITEM_DEFINED_TRANSFORMATION($,$,#25586,#25656);
#121=ITEM_DEFINED_TRANSFORMATION($,$,#25636,#25657);
#122=ITEM_DEFINED_TRANSFORMATION($,$,#25659,#25787);
#123=ITEM_DEFINED_TRANSFORMATION($,$,#25679,#25788);
#124=ITEM_DEFINED_TRANSFORMATION($,$,#25699,#25789);
#125=ITEM_DEFINED_TRANSFORMATION($,$,#25716,#25790);
#126=ITEM_DEFINED_TRANSFORMATION($,$,#25770,#25791);
#127=ITEM_DEFINED_TRANSFORMATION($,$,#25906,#25967);
#128=ITEM_DEFINED_TRANSFORMATION($,$,#25945,#25968);
#129=ITEM_DEFINED_TRANSFORMATION($,$,#25956,#25969);
#130=ITEM_DEFINED_TRANSFORMATION($,$,#25817,#26106);
#131=ITEM_DEFINED_TRANSFORMATION($,$,#25836,#26107);
#132=ITEM_DEFINED_TRANSFORMATION($,$,#25867,#26108);
#133=ITEM_DEFINED_TRANSFORMATION($,$,#25905,#26109);
#134=ITEM_DEFINED_TRANSFORMATION($,$,#25970,#26110);
#135=ITEM_DEFINED_TRANSFORMATION($,$,#25981,#26111);
#136=ITEM_DEFINED_TRANSFORMATION($,$,#25970,#26112);
#137=ITEM_DEFINED_TRANSFORMATION($,$,#25981,#26113);
#138=ITEM_DEFINED_TRANSFORMATION($,$,#25970,#26114);
#139=ITEM_DEFINED_TRANSFORMATION($,$,#25981,#26115);
#140=ITEM_DEFINED_TRANSFORMATION($,$,#25970,#26116);
#141=ITEM_DEFINED_TRANSFORMATION($,$,#25981,#26117);
#142=ITEM_DEFINED_TRANSFORMATION($,$,#26009,#26118);
#143=ITEM_DEFINED_TRANSFORMATION($,$,#26054,#26119);
#144=ITEM_DEFINED_TRANSFORMATION($,$,#26054,#26120);
#145=ITEM_DEFINED_TRANSFORMATION($,$,#26054,#26121);
#146=ITEM_DEFINED_TRANSFORMATION($,$,#26080,#26122);
#147=ITEM_DEFINED_TRANSFORMATION($,$,#26080,#26123);
#148=ITEM_DEFINED_TRANSFORMATION($,$,#26080,#26124);
#149=ITEM_DEFINED_TRANSFORMATION($,$,#26080,#26125);
#150=ITEM_DEFINED_TRANSFORMATION($,$,#25202,#26410);
#151=ITEM_DEFINED_TRANSFORMATION($,$,#25299,#26411);
#152=ITEM_DEFINED_TRANSFORMATION($,$,#25352,#26412);
#153=ITEM_DEFINED_TRANSFORMATION($,$,#25383,#26413);
#154=ITEM_DEFINED_TRANSFORMATION($,$,#25405,#26414);
#155=ITEM_DEFINED_TRANSFORMATION($,$,#25436,#26415);
#156=ITEM_DEFINED_TRANSFORMATION($,$,#25459,#26416);
#157=ITEM_DEFINED_TRANSFORMATION($,$,#25473,#26417);
#158=ITEM_DEFINED_TRANSFORMATION($,$,#26080,#26418);
#159=ITEM_DEFINED_TRANSFORMATION($,$,#26080,#26419);
#160=ITEM_DEFINED_TRANSFORMATION($,$,#26080,#26420);
#161=ITEM_DEFINED_TRANSFORMATION($,$,#26080,#26421);
#162=ITEM_DEFINED_TRANSFORMATION($,$,#25487,#26422);
#163=ITEM_DEFINED_TRANSFORMATION($,$,#26054,#26423);
#164=ITEM_DEFINED_TRANSFORMATION($,$,#26054,#26424);
#165=ITEM_DEFINED_TRANSFORMATION($,$,#26054,#26425);
#166=ITEM_DEFINED_TRANSFORMATION($,$,#26054,#26426);
#167=ITEM_DEFINED_TRANSFORMATION($,$,#26080,#26427);
#168=ITEM_DEFINED_TRANSFORMATION($,$,#26080,#26428);
#169=ITEM_DEFINED_TRANSFORMATION($,$,#25530,#26429);
#170=ITEM_DEFINED_TRANSFORMATION($,$,#26054,#26430);
#171=ITEM_DEFINED_TRANSFORMATION($,$,#26054,#26431);
#172=ITEM_DEFINED_TRANSFORMATION($,$,#26054,#26432);
#173=ITEM_DEFINED_TRANSFORMATION($,$,#26384,#26433);
#174=ITEM_DEFINED_TRANSFORMATION($,$,#26384,#26434);
#175=ITEM_DEFINED_TRANSFORMATION($,$,#25658,#26435);
#176=ITEM_DEFINED_TRANSFORMATION($,$,#26054,#26436);
#177=ITEM_DEFINED_TRANSFORMATION($,$,#26054,#26437);
#178=ITEM_DEFINED_TRANSFORMATION($,$,#26054,#26438);
#179=ITEM_DEFINED_TRANSFORMATION($,$,#26080,#26439);
#180=ITEM_DEFINED_TRANSFORMATION($,$,#26080,#26440);
#181=ITEM_DEFINED_TRANSFORMATION($,$,#25792,#26441);
#182=ITEM_DEFINED_TRANSFORMATION($,$,#25792,#26442);
#183=ITEM_DEFINED_TRANSFORMATION($,$,#25792,#26443);
#184=ITEM_DEFINED_TRANSFORMATION($,$,#25792,#26444);
#185=ITEM_DEFINED_TRANSFORMATION($,$,#26127,#26445);
#186=ITEM_DEFINED_TRANSFORMATION($,$,#26282,#26446);
#187=ITEM_DEFINED_TRANSFORMATION($,$,#26291,#26447);
#188=ITEM_DEFINED_TRANSFORMATION($,$,#26305,#26448);
#189=ITEM_DEFINED_TRANSFORMATION($,$,#26329,#26449);
#190=ITEM_DEFINED_TRANSFORMATION($,$,#26338,#26450);
#191=ITEM_DEFINED_TRANSFORMATION($,$,#26347,#26451);
#192=ITEM_DEFINED_TRANSFORMATION($,$,#26358,#26452);
#193=ITEM_DEFINED_TRANSFORMATION($,$,#26358,#26453);
#194=ITEM_DEFINED_TRANSFORMATION($,$,#26375,#26454);
#195=ITEM_DEFINED_TRANSFORMATION($,$,#26384,#26455);
#196=ITEM_DEFINED_TRANSFORMATION($,$,#25201,#26456);
#197=ITEM_DEFINED_TRANSFORMATION($,$,#25816,#26457);
#198=ITEM_DEFINED_TRANSFORMATION($,$,#26126,#26458);
#199=ITEM_DEFINED_TRANSFORMATION($,$,#24001,#26459);
#200=ITEM_DEFINED_TRANSFORMATION($,$,#25200,#26460);
#201=(
REPRESENTATION_RELATIONSHIP($,$,#63364,#63363)
REPRESENTATION_RELATIONSHIP_WITH_TRANSFORMATION(#37)
SHAPE_REPRESENTATION_RELATIONSHIP()
);
#202=(
REPRESENTATION_RELATIONSHIP($,$,#63365,#63363)
REPRESENTATION_RELATIONSHIP_WITH_TRANSFORMATION(#38)
SHAPE_REPRESENTATION_RELATIONSHIP()
);
#203=(
REPRESENTATION_RELATIONSHIP($,$,#63366,#63363)
REPRESENTATION_RELATIONSHIP_WITH_TRANSFORMATION(#39)
SHAPE_REPRESENTATION_RELATIONSHIP()
);
#204=(
REPRESENTATION_RELATIONSHIP($,$,#63367,#63363)
REPRESENTATION_RELATIONSHIP_WITH_TRANSFORMATION(#40)
SHAPE_REPRESENTATION_RELATIONSHIP()
);
#205=(
REPRESENTATION_RELATIONSHIP($,$,#63368,#63363)
REPRESENTATION_RELATIONSHIP_WITH_TRANSFORMATION(#41)
SHAPE_REPRESENTATION_RELATIONSHIP()
);
#206=(
REPRESENTATION_RELATIONSHIP($,$,#63370,#63369)
REPRESENTATION_RELATIONSHIP_WITH_TRANSFORMATION(#42)
SHAPE_REPRESENTATION_RELATIONSHIP()
);
#207=(
REPRESENTATION_RELATIONSHIP($,$,#63371,#63369)
REPRESENTATION_RELATIONSHIP_WITH_TRANSFORMATION(#43)
SHAPE_REPRESENTATION_RELATIONSHIP()
);
#208=(
REPRESENTATION_RELATIONSHIP($,$,#63372,#63369)
REPRESENTATION_RELATIONSHIP_WITH_TRANSFORMATION(#44)
SHAPE_REPRESENTATION_RELATIONSHIP()
);
#209=(
REPRESENTATION_RELATIONSHIP($,$,#63373,#63369)
REPRESENTATION_RELATIONSHIP_WITH_TRANSFORMATION(#45)
SHAPE_REPRESENTATION_RELATIONSHIP()
);
#210=(
REPRESENTATION_RELATIONSHIP($,$,#63374,#63369)
REPRESENTATION_RELATIONSHIP_WITH_TRANSFORMATION(#46)
SHAPE_REPRESENTATION_RELATIONSHIP()
);
#211=(
REPRESENTATION_RELATIONSHIP($,$,#63380,#63379)
REPRESENTATION_RELATIONSHIP_WITH_TRANSFORMATION(#47)
SHAPE_REPRESENTATION_RELATIONSHIP()
);
#212=(
REPRESENTATION_RELATIONSHIP($,$,#63381,#63379)
REPRESENTATION_RELATIONSHIP_WITH_TRANSFORMATION(#48)
SHAPE_REPRESENTATION_RELATIONSHIP()
);
#213=(
REPRESENTATION_RELATIONSHIP($,$,#63382,#63379)
REPRESENTATION_RELATIONSHIP_WITH_TRANSFORMATION(#49)
SHAPE_REPRESENTATION_RELATIONSHIP()
);
#214=(
REPRESENTATION_RELATIONSHIP($,$,#63376,#63375)
REPRESENTATION_RELATIONSHIP_WITH_TRANSFORMATION(#50)
SHAPE_REPRESENTATION_RELATIONSHIP()
);
#215=(
REPRESENTATION_RELATIONSHIP($,$,#63377,#63375)
REPRESENTATION_RELATIONSHIP_WITH_TRANSFORMATION(#51)
SHAPE_REPRESENTATION_RELATIONSHIP()
);
#216=(
REPRESENTATION_RELATIONSHIP($,$,#63378,#63375)
REPRESENTATION_RELATIONSHIP_WITH_TRANSFORMATION(#52)
SHAPE_REPRESENTATION_RELATIONSHIP()
);
#217=(
REPRESENTATION_RELATIONSHIP($,$,#63379,#63375)
REPRESENTATION_RELATIONSHIP_WITH_TRANSFORMATION(#53)
SHAPE_REPRESENTATION_RELATIONSHIP()
);
#218=(
REPRESENTATION_RELATIONSHIP($,$,#63383,#63375)
REPRESENTATION_RELATIONSHIP_WITH_TRANSFORMATION(#54)
SHAPE_REPRESENTATION_RELATIONSHIP()
);
#219=(
REPRESENTATION_RELATIONSHIP($,$,#63384,#63375)
REPRESENTATION_RELATIONSHIP_WITH_TRANSFORMATION(#55)
SHAPE_REPRESENTATION_RELATIONSHIP()
);
#220=(
REPRESENTATION_RELATIONSHIP($,$,#63383,#63375)
REPRESENTATION_RELATIONSHIP_WITH_TRANSFORMATION(#56)
SHAPE_REPRESENTATION_RELATIONSHIP()
);
#221=(
REPRESENTATION_RELATIONSHIP($,$,#63384,#63375)
REPRESENTATION_RELATIONSHIP_WITH_TRANSFORMATION(#57)
SHAPE_REPRESENTATION_RELATIONSHIP()
);
#222=(
REPRESENTATION_RELATIONSHIP($,$,#63383,#63375)
REPRESENTATION_RELATIONSHIP_WITH_TRANSFORMATION(#58)
SHAPE_REPRESENTATION_RELATIONSHIP()
);
#223=(
REPRESENTATION_RELATIONSHIP($,$,#63384,#63375)
REPRESENTATION_RELATIONSHIP_WITH_TRANSFORMATION(#59)
SHAPE_REPRESENTATION_RELATIONSHIP()
);
#224=(
REPRESENTATION_RELATIONSHIP($,$,#63383,#63375)
REPRESENTATION_RELATIONSHIP_WITH_TRANSFORMATION(#60)
SHAPE_REPRESENTATION_RELATIONSHIP()
);
#225=(
REPRESENTATION_RELATIONSHIP($,$,#63384,#63375)
REPRESENTATION_RELATIONSHIP_WITH_TRANSFORMATION(#61)
SHAPE_REPRESENTATION_RELATIONSHIP()
);
#226=(
REPRESENTATION_RELATIONSHIP($,$,#63385,#63375)
REPRESENTATION_RELATIONSHIP_WITH_TRANSFORMATION(#62)
SHAPE_REPRESENTATION_RELATIONSHIP()
);
#227=(
REPRESENTATION_RELATIONSHIP($,$,#63386,#63375)
REPRESENTATION_RELATIONSHIP_WITH_TRANSFORMATION(#63)
SHAPE_REPRESENTATION_RELATIONSHIP()
);
#228=(
REPRESENTATION_RELATIONSHIP($,$,#63386,#63375)
REPRESENTATION_RELATIONSHIP_WITH_TRANSFORMATION(#64)
SHAPE_REPRESENTATION_RELATIONSHIP()
);
#229=(
REPRESENTATION_RELATIONSHIP($,$,#63386,#63375)
REPRESENTATION_RELATIONSHIP_WITH_TRANSFORMATION(#65)
SHAPE_REPRESENTATION_RELATIONSHIP()
);
#230=(
REPRESENTATION_RELATIONSHIP($,$,#63387,#63375)
REPRESENTATION_RELATIONSHIP_WITH_TRANSFORMATION(#66)
SHAPE_REPRESENTATION_RELATIONSHIP()
);
#231=(
REPRESENTATION_RELATIONSHIP($,$,#63387,#63375)
REPRESENTATION_RELATIONSHIP_WITH_TRANSFORMATION(#67)
SHAPE_REPRESENTATION_RELATIONSHIP()
);
#232=(
REPRESENTATION_RELATIONSHIP($,$,#63387,#63375)
REPRESENTATION_RELATIONSHIP_WITH_TRANSFORMATION(#68)
SHAPE_REPRESENTATION_RELATIONSHIP()
);
#233=(
REPRESENTATION_RELATIONSHIP($,$,#63387,#63375)
REPRESENTATION_RELATIONSHIP_WITH_TRANSFORMATION(#69)
SHAPE_REPRESENTATION_RELATIONSHIP()
);
#234=(
REPRESENTATION_RELATIONSHIP($,$,#63352,#63351)
REPRESENTATION_RELATIONSHIP_WITH_TRANSFORMATION(#70)
SHAPE_REPRESENTATION_RELATIONSHIP()
);
#235=(
REPRESENTATION_RELATIONSHIP($,$,#63353,#63351)
REPRESENTATION_RELATIONSHIP_WITH_TRANSFORMATION(#71)
SHAPE_REPRESENTATION_RELATIONSHIP()
);
#236=(
REPRESENTATION_RELATIONSHIP($,$,#63354,#63351)
REPRESENTATION_RELATIONSHIP_WITH_TRANSFORMATION(#72)
SHAPE_REPRESENTATION_RELATIONSHIP()
);
#237=(
REPRESENTATION_RELATIONSHIP($,$,#63355,#63351)
REPRESENTATION_RELATIONSHIP_WITH_TRANSFORMATION(#73)
SHAPE_REPRESENTATION_RELATIONSHIP()
);
#238=(
REPRESENTATION_RELATIONSHIP($,$,#63356,#63351)
REPRESENTATION_RELATIONSHIP_WITH_TRANSFORMATION(#74)
SHAPE_REPRESENTATION_RELATIONSHIP()
);
#239=(
REPRESENTATION_RELATIONSHIP($,$,#63357,#63351)
REPRESENTATION_RELATIONSHIP_WITH_TRANSFORMATION(#75)
SHAPE_REPRESENTATION_RELATIONSHIP()
);
#240=(
REPRESENTATION_RELATIONSHIP($,$,#63358,#63351)
REPRESENTATION_RELATIONSHIP_WITH_TRANSFORMATION(#76)
SHAPE_REPRESENTATION_RELATIONSHIP()
);
#241=(
REPRESENTATION_RELATIONSHIP($,$,#63359,#63351)
REPRESENTATION_RELATIONSHIP_WITH_TRANSFORMATION(#77)
SHAPE_REPRESENTATION_RELATIONSHIP()
);
#242=(
REPRESENTATION_RELATIONSHIP($,$,#63360,#63351)
REPRESENTATION_RELATIONSHIP_WITH_TRANSFORMATION(#78)
SHAPE_REPRESENTATION_RELATIONSHIP()
);
#243=(
REPRESENTATION_RELATIONSHIP($,$,#63361,#63351)
REPRESENTATION_RELATIONSHIP_WITH_TRANSFORMATION(#79)
SHAPE_REPRESENTATION_RELATIONSHIP()
);
#244=(
REPRESENTATION_RELATIONSHIP($,$,#63387,#63351)
REPRESENTATION_RELATIONSHIP_WITH_TRANSFORMATION(#80)
SHAPE_REPRESENTATION_RELATIONSHIP()
);
#245=(
REPRESENTATION_RELATIONSHIP($,$,#63387,#63351)
REPRESENTATION_RELATIONSHIP_WITH_TRANSFORMATION(#81)
SHAPE_REPRESENTATION_RELATIONSHIP()
);
#246=(
REPRESENTATION_RELATIONSHIP($,$,#63387,#63351)
REPRESENTATION_RELATIONSHIP_WITH_TRANSFORMATION(#82)
SHAPE_REPRESENTATION_RELATIONSHIP()
);
#247=(
REPRESENTATION_RELATIONSHIP($,$,#63387,#63351)
REPRESENTATION_RELATIONSHIP_WITH_TRANSFORMATION(#83)
SHAPE_REPRESENTATION_RELATIONSHIP()
);
#248=(
REPRESENTATION_RELATIONSHIP($,$,#63362,#63351)
REPRESENTATION_RELATIONSHIP_WITH_TRANSFORMATION(#84)
SHAPE_REPRESENTATION_RELATIONSHIP()
);
#249=(
REPRESENTATION_RELATIONSHIP($,$,#63386,#63351)
REPRESENTATION_RELATIONSHIP_WITH_TRANSFORMATION(#85)
SHAPE_REPRESENTATION_RELATIONSHIP()
);
#250=(
REPRESENTATION_RELATIONSHIP($,$,#63386,#63351)
REPRESENTATION_RELATIONSHIP_WITH_TRANSFORMATION(#86)
SHAPE_REPRESENTATION_RELATIONSHIP()
);
#251=(
REPRESENTATION_RELATIONSHIP($,$,#63386,#63351)
REPRESENTATION_RELATIONSHIP_WITH_TRANSFORMATION(#87)
SHAPE_REPRESENTATION_RELATIONSHIP()
);
#252=(
REPRESENTATION_RELATIONSHIP($,$,#63386,#63351)
REPRESENTATION_RELATIONSHIP_WITH_TRANSFORMATION(#88)
SHAPE_REPRESENTATION_RELATIONSHIP()
);
#253=(
REPRESENTATION_RELATIONSHIP($,$,#63387,#63351)
REPRESENTATION_RELATIONSHIP_WITH_TRANSFORMATION(#89)
SHAPE_REPRESENTATION_RELATIONSHIP()
);
#254=(
REPRESENTATION_RELATIONSHIP($,$,#63387,#63351)
REPRESENTATION_RELATIONSHIP_WITH_TRANSFORMATION(#90)
SHAPE_REPRESENTATION_RELATIONSHIP()
);
#255=(
REPRESENTATION_RELATIONSHIP($,$,#63363,#63351)
REPRESENTATION_RELATIONSHIP_WITH_TRANSFORMATION(#91)
SHAPE_REPRESENTATION_RELATIONSHIP()
);
#256=(
REPRESENTATION_RELATIONSHIP($,$,#63386,#63351)
REPRESENTATION_RELATIONSHIP_WITH_TRANSFORMATION(#92)
SHAPE_REPRESENTATION_RELATIONSHIP()
);
#257=(
REPRESENTATION_RELATIONSHIP($,$,#63386,#63351)
REPRESENTATION_RELATIONSHIP_WITH_TRANSFORMATION(#93)
SHAPE_REPRESENTATION_RELATIONSHIP()
);
#258=(
REPRESENTATION_RELATIONSHIP($,$,#63386,#63351)
REPRESENTATION_RELATIONSHIP_WITH_TRANSFORMATION(#94)
SHAPE_REPRESENTATION_RELATIONSHIP()
);
#259=(
REPRESENTATION_RELATIONSHIP($,$,#63398,#63351)
REPRESENTATION_RELATIONSHIP_WITH_TRANSFORMATION(#95)
SHAPE_REPRESENTATION_RELATIONSHIP()
);
#260=(
REPRESENTATION_RELATIONSHIP($,$,#63398,#63351)
REPRESENTATION_RELATIONSHIP_WITH_TRANSFORMATION(#96)
SHAPE_REPRESENTATION_RELATIONSHIP()
);
#261=(
REPRESENTATION_RELATIONSHIP($,$,#63369,#63351)
REPRESENTATION_RELATIONSHIP_WITH_TRANSFORMATION(#97)
SHAPE_REPRESENTATION_RELATIONSHIP()
);
#262=(
REPRESENTATION_RELATIONSHIP($,$,#63386,#63351)
REPRESENTATION_RELATIONSHIP_WITH_TRANSFORMATION(#98)
SHAPE_REPRESENTATION_RELATIONSHIP()
);
#263=(
REPRESENTATION_RELATIONSHIP($,$,#63386,#63351)
REPRESENTATION_RELATIONSHIP_WITH_TRANSFORMATION(#99)
SHAPE_REPRESENTATION_RELATIONSHIP()
);
#264=(
REPRESENTATION_RELATIONSHIP($,$,#63386,#63351)
REPRESENTATION_RELATIONSHIP_WITH_TRANSFORMATION(#100)
SHAPE_REPRESENTATION_RELATIONSHIP()
);
#265=(
REPRESENTATION_RELATIONSHIP($,$,#63387,#63351)
REPRESENTATION_RELATIONSHIP_WITH_TRANSFORMATION(#101)
SHAPE_REPRESENTATION_RELATIONSHIP()
);
#266=(
REPRESENTATION_RELATIONSHIP($,$,#63387,#63351)
REPRESENTATION_RELATIONSHIP_WITH_TRANSFORMATION(#102)
SHAPE_REPRESENTATION_RELATIONSHIP()
);
#267=(
REPRESENTATION_RELATIONSHIP($,$,#63389,#63388)
REPRESENTATION_RELATIONSHIP_WITH_TRANSFORMATION(#103)
SHAPE_REPRESENTATION_RELATIONSHIP()
);
#268=(
REPRESENTATION_RELATIONSHIP($,$,#63390,#63388)
REPRESENTATION_RELATIONSHIP_WITH_TRANSFORMATION(#104)
SHAPE_REPRESENTATION_RELATIONSHIP()
);
#269=(
REPRESENTATION_RELATIONSHIP($,$,#63391,#63388)
REPRESENTATION_RELATIONSHIP_WITH_TRANSFORMATION(#105)
SHAPE_REPRESENTATION_RELATIONSHIP()
);
#270=(
REPRESENTATION_RELATIONSHIP($,$,#63392,#63388)
REPRESENTATION_RELATIONSHIP_WITH_TRANSFORMATION(#106)
SHAPE_REPRESENTATION_RELATIONSHIP()
);
#271=(
REPRESENTATION_RELATIONSHIP($,$,#63393,#63388)
REPRESENTATION_RELATIONSHIP_WITH_TRANSFORMATION(#107)
SHAPE_REPRESENTATION_RELATIONSHIP()
);
#272=(
REPRESENTATION_RELATIONSHIP($,$,#63394,#63388)
REPRESENTATION_RELATIONSHIP_WITH_TRANSFORMATION(#108)
SHAPE_REPRESENTATION_RELATIONSHIP()
);
#273=(
REPRESENTATION_RELATIONSHIP($,$,#63395,#63388)
REPRESENTATION_RELATIONSHIP_WITH_TRANSFORMATION(#109)
SHAPE_REPRESENTATION_RELATIONSHIP()
);
#274=(
REPRESENTATION_RELATIONSHIP($,$,#63396,#63388)
REPRESENTATION_RELATIONSHIP_WITH_TRANSFORMATION(#110)
SHAPE_REPRESENTATION_RELATIONSHIP()
);
#275=(
REPRESENTATION_RELATIONSHIP($,$,#63396,#63388)
REPRESENTATION_RELATIONSHIP_WITH_TRANSFORMATION(#111)
SHAPE_REPRESENTATION_RELATIONSHIP()
);
#276=(
REPRESENTATION_RELATIONSHIP($,$,#63397,#63388)
REPRESENTATION_RELATIONSHIP_WITH_TRANSFORMATION(#112)
SHAPE_REPRESENTATION_RELATIONSHIP()
);
#277=(
REPRESENTATION_RELATIONSHIP($,$,#63398,#63388)
REPRESENTATION_RELATIONSHIP_WITH_TRANSFORMATION(#113)
SHAPE_REPRESENTATION_RELATIONSHIP()
);
#278=(
REPRESENTATION_RELATIONSHIP($,$,#63351,#63350)
REPRESENTATION_RELATIONSHIP_WITH_TRANSFORMATION(#114)
SHAPE_REPRESENTATION_RELATIONSHIP()
);
#279=(
REPRESENTATION_RELATIONSHIP($,$,#63375,#63350)
REPRESENTATION_RELATIONSHIP_WITH_TRANSFORMATION(#115)
SHAPE_REPRESENTATION_RELATIONSHIP()
);
#280=(
REPRESENTATION_RELATIONSHIP($,$,#63388,#63350)
REPRESENTATION_RELATIONSHIP_WITH_TRANSFORMATION(#116)
SHAPE_REPRESENTATION_RELATIONSHIP()
);
#281=(
REPRESENTATION_RELATIONSHIP($,$,#63411,#63410)
REPRESENTATION_RELATIONSHIP_WITH_TRANSFORMATION(#117)
SHAPE_REPRESENTATION_RELATIONSHIP()
);
#282=(
REPRESENTATION_RELATIONSHIP($,$,#63412,#63410)
REPRESENTATION_RELATIONSHIP_WITH_TRANSFORMATION(#118)
SHAPE_REPRESENTATION_RELATIONSHIP()
);
#283=(
REPRESENTATION_RELATIONSHIP($,$,#63413,#63410)
REPRESENTATION_RELATIONSHIP_WITH_TRANSFORMATION(#119)
SHAPE_REPRESENTATION_RELATIONSHIP()
);
#284=(
REPRESENTATION_RELATIONSHIP($,$,#63414,#63410)
REPRESENTATION_RELATIONSHIP_WITH_TRANSFORMATION(#120)
SHAPE_REPRESENTATION_RELATIONSHIP()
);
#285=(
REPRESENTATION_RELATIONSHIP($,$,#63415,#63410)
REPRESENTATION_RELATIONSHIP_WITH_TRANSFORMATION(#121)
SHAPE_REPRESENTATION_RELATIONSHIP()
);
#286=(
REPRESENTATION_RELATIONSHIP($,$,#63417,#63416)
REPRESENTATION_RELATIONSHIP_WITH_TRANSFORMATION(#122)
SHAPE_REPRESENTATION_RELATIONSHIP()
);
#287=(
REPRESENTATION_RELATIONSHIP($,$,#63418,#63416)
REPRESENTATION_RELATIONSHIP_WITH_TRANSFORMATION(#123)
SHAPE_REPRESENTATION_RELATIONSHIP()
);
#288=(
REPRESENTATION_RELATIONSHIP($,$,#63419,#63416)
REPRESENTATION_RELATIONSHIP_WITH_TRANSFORMATION(#124)
SHAPE_REPRESENTATION_RELATIONSHIP()
);
#289=(
REPRESENTATION_RELATIONSHIP($,$,#63420,#63416)
REPRESENTATION_RELATIONSHIP_WITH_TRANSFORMATION(#125)
SHAPE_REPRESENTATION_RELATIONSHIP()
);
#290=(
REPRESENTATION_RELATIONSHIP($,$,#63421,#63416)
REPRESENTATION_RELATIONSHIP_WITH_TRANSFORMATION(#126)
SHAPE_REPRESENTATION_RELATIONSHIP()
);
#291=(
REPRESENTATION_RELATIONSHIP($,$,#63428,#63427)
REPRESENTATION_RELATIONSHIP_WITH_TRANSFORMATION(#127)
SHAPE_REPRESENTATION_RELATIONSHIP()
);
#292=(
REPRESENTATION_RELATIONSHIP($,$,#63429,#63427)
REPRESENTATION_RELATIONSHIP_WITH_TRANSFORMATION(#128)
SHAPE_REPRESENTATION_RELATIONSHIP()
);
#293=(
REPRESENTATION_RELATIONSHIP($,$,#63430,#63427)
REPRESENTATION_RELATIONSHIP_WITH_TRANSFORMATION(#129)
SHAPE_REPRESENTATION_RELATIONSHIP()
);
#294=(
REPRESENTATION_RELATIONSHIP($,$,#63424,#63423)
REPRESENTATION_RELATIONSHIP_WITH_TRANSFORMATION(#130)
SHAPE_REPRESENTATION_RELATIONSHIP()
);
#295=(
REPRESENTATION_RELATIONSHIP($,$,#63425,#63423)
REPRESENTATION_RELATIONSHIP_WITH_TRANSFORMATION(#131)
SHAPE_REPRESENTATION_RELATIONSHIP()
);
#296=(
REPRESENTATION_RELATIONSHIP($,$,#63426,#63423)
REPRESENTATION_RELATIONSHIP_WITH_TRANSFORMATION(#132)
SHAPE_REPRESENTATION_RELATIONSHIP()
);
#297=(
REPRESENTATION_RELATIONSHIP($,$,#63427,#63423)
REPRESENTATION_RELATIONSHIP_WITH_TRANSFORMATION(#133)
SHAPE_REPRESENTATION_RELATIONSHIP()
);
#298=(
REPRESENTATION_RELATIONSHIP($,$,#63431,#63423)
REPRESENTATION_RELATIONSHIP_WITH_TRANSFORMATION(#134)
SHAPE_REPRESENTATION_RELATIONSHIP()
);
#299=(
REPRESENTATION_RELATIONSHIP($,$,#63432,#63423)
REPRESENTATION_RELATIONSHIP_WITH_TRANSFORMATION(#135)
SHAPE_REPRESENTATION_RELATIONSHIP()
);
#300=(
REPRESENTATION_RELATIONSHIP($,$,#63431,#63423)
REPRESENTATION_RELATIONSHIP_WITH_TRANSFORMATION(#136)
SHAPE_REPRESENTATION_RELATIONSHIP()
);
#301=(
REPRESENTATION_RELATIONSHIP($,$,#63432,#63423)
REPRESENTATION_RELATIONSHIP_WITH_TRANSFORMATION(#137)
SHAPE_REPRESENTATION_RELATIONSHIP()
);
#302=(
REPRESENTATION_RELATIONSHIP($,$,#63431,#63423)
REPRESENTATION_RELATIONSHIP_WITH_TRANSFORMATION(#138)
SHAPE_REPRESENTATION_RELATIONSHIP()
);
#303=(
REPRESENTATION_RELATIONSHIP($,$,#63432,#63423)
REPRESENTATION_RELATIONSHIP_WITH_TRANSFORMATION(#139)
SHAPE_REPRESENTATION_RELATIONSHIP()
);
#304=(
REPRESENTATION_RELATIONSHIP($,$,#63431,#63423)
REPRESENTATION_RELATIONSHIP_WITH_TRANSFORMATION(#140)
SHAPE_REPRESENTATION_RELATIONSHIP()
);
#305=(
REPRESENTATION_RELATIONSHIP($,$,#63432,#63423)
REPRESENTATION_RELATIONSHIP_WITH_TRANSFORMATION(#141)
SHAPE_REPRESENTATION_RELATIONSHIP()
);
#306=(
REPRESENTATION_RELATIONSHIP($,$,#63433,#63423)
REPRESENTATION_RELATIONSHIP_WITH_TRANSFORMATION(#142)
SHAPE_REPRESENTATION_RELATIONSHIP()
);
#307=(
REPRESENTATION_RELATIONSHIP($,$,#63434,#63423)
REPRESENTATION_RELATIONSHIP_WITH_TRANSFORMATION(#143)
SHAPE_REPRESENTATION_RELATIONSHIP()
);
#308=(
REPRESENTATION_RELATIONSHIP($,$,#63434,#63423)
REPRESENTATION_RELATIONSHIP_WITH_TRANSFORMATION(#144)
SHAPE_REPRESENTATION_RELATIONSHIP()
);
#309=(
REPRESENTATION_RELATIONSHIP($,$,#63434,#63423)
REPRESENTATION_RELATIONSHIP_WITH_TRANSFORMATION(#145)
SHAPE_REPRESENTATION_RELATIONSHIP()
);
#310=(
REPRESENTATION_RELATIONSHIP($,$,#63435,#63423)
REPRESENTATION_RELATIONSHIP_WITH_TRANSFORMATION(#146)
SHAPE_REPRESENTATION_RELATIONSHIP()
);
#311=(
REPRESENTATION_RELATIONSHIP($,$,#63435,#63423)
REPRESENTATION_RELATIONSHIP_WITH_TRANSFORMATION(#147)
SHAPE_REPRESENTATION_RELATIONSHIP()
);
#312=(
REPRESENTATION_RELATIONSHIP($,$,#63435,#63423)
REPRESENTATION_RELATIONSHIP_WITH_TRANSFORMATION(#148)
SHAPE_REPRESENTATION_RELATIONSHIP()
);
#313=(
REPRESENTATION_RELATIONSHIP($,$,#63435,#63423)
REPRESENTATION_RELATIONSHIP_WITH_TRANSFORMATION(#149)
SHAPE_REPRESENTATION_RELATIONSHIP()
);
#314=(
REPRESENTATION_RELATIONSHIP($,$,#63401,#63400)
REPRESENTATION_RELATIONSHIP_WITH_TRANSFORMATION(#150)
SHAPE_REPRESENTATION_RELATIONSHIP()
);
#315=(
REPRESENTATION_RELATIONSHIP($,$,#63402,#63400)
REPRESENTATION_RELATIONSHIP_WITH_TRANSFORMATION(#151)
SHAPE_REPRESENTATION_RELATIONSHIP()
);
#316=(
REPRESENTATION_RELATIONSHIP($,$,#63403,#63400)
REPRESENTATION_RELATIONSHIP_WITH_TRANSFORMATION(#152)
SHAPE_REPRESENTATION_RELATIONSHIP()
);
#317=(
REPRESENTATION_RELATIONSHIP($,$,#63404,#63400)
REPRESENTATION_RELATIONSHIP_WITH_TRANSFORMATION(#153)
SHAPE_REPRESENTATION_RELATIONSHIP()
);
#318=(
REPRESENTATION_RELATIONSHIP($,$,#63405,#63400)
REPRESENTATION_RELATIONSHIP_WITH_TRANSFORMATION(#154)
SHAPE_REPRESENTATION_RELATIONSHIP()
);
#319=(
REPRESENTATION_RELATIONSHIP($,$,#63406,#63400)
REPRESENTATION_RELATIONSHIP_WITH_TRANSFORMATION(#155)
SHAPE_REPRESENTATION_RELATIONSHIP()
);
#320=(
REPRESENTATION_RELATIONSHIP($,$,#63407,#63400)
REPRESENTATION_RELATIONSHIP_WITH_TRANSFORMATION(#156)
SHAPE_REPRESENTATION_RELATIONSHIP()
);
#321=(
REPRESENTATION_RELATIONSHIP($,$,#63408,#63400)
REPRESENTATION_RELATIONSHIP_WITH_TRANSFORMATION(#157)
SHAPE_REPRESENTATION_RELATIONSHIP()
);
#322=(
REPRESENTATION_RELATIONSHIP($,$,#63435,#63400)
REPRESENTATION_RELATIONSHIP_WITH_TRANSFORMATION(#158)
SHAPE_REPRESENTATION_RELATIONSHIP()
);
#323=(
REPRESENTATION_RELATIONSHIP($,$,#63435,#63400)
REPRESENTATION_RELATIONSHIP_WITH_TRANSFORMATION(#159)
SHAPE_REPRESENTATION_RELATIONSHIP()
);
#324=(
REPRESENTATION_RELATIONSHIP($,$,#63435,#63400)
REPRESENTATION_RELATIONSHIP_WITH_TRANSFORMATION(#160)
SHAPE_REPRESENTATION_RELATIONSHIP()
);
#325=(
REPRESENTATION_RELATIONSHIP($,$,#63435,#63400)
REPRESENTATION_RELATIONSHIP_WITH_TRANSFORMATION(#161)
SHAPE_REPRESENTATION_RELATIONSHIP()
);
#326=(
REPRESENTATION_RELATIONSHIP($,$,#63409,#63400)
REPRESENTATION_RELATIONSHIP_WITH_TRANSFORMATION(#162)
SHAPE_REPRESENTATION_RELATIONSHIP()
);
#327=(
REPRESENTATION_RELATIONSHIP($,$,#63434,#63400)
REPRESENTATION_RELATIONSHIP_WITH_TRANSFORMATION(#163)
SHAPE_REPRESENTATION_RELATIONSHIP()
);
#328=(
REPRESENTATION_RELATIONSHIP($,$,#63434,#63400)
REPRESENTATION_RELATIONSHIP_WITH_TRANSFORMATION(#164)
SHAPE_REPRESENTATION_RELATIONSHIP()
);
#329=(
REPRESENTATION_RELATIONSHIP($,$,#63434,#63400)
REPRESENTATION_RELATIONSHIP_WITH_TRANSFORMATION(#165)
SHAPE_REPRESENTATION_RELATIONSHIP()
);
#330=(
REPRESENTATION_RELATIONSHIP($,$,#63434,#63400)
REPRESENTATION_RELATIONSHIP_WITH_TRANSFORMATION(#166)
SHAPE_REPRESENTATION_RELATIONSHIP()
);
#331=(
REPRESENTATION_RELATIONSHIP($,$,#63435,#63400)
REPRESENTATION_RELATIONSHIP_WITH_TRANSFORMATION(#167)
SHAPE_REPRESENTATION_RELATIONSHIP()
);
#332=(
REPRESENTATION_RELATIONSHIP($,$,#63435,#63400)
REPRESENTATION_RELATIONSHIP_WITH_TRANSFORMATION(#168)
SHAPE_REPRESENTATION_RELATIONSHIP()
);
#333=(
REPRESENTATION_RELATIONSHIP($,$,#63410,#63400)
REPRESENTATION_RELATIONSHIP_WITH_TRANSFORMATION(#169)
SHAPE_REPRESENTATION_RELATIONSHIP()
);
#334=(
REPRESENTATION_RELATIONSHIP($,$,#63434,#63400)
REPRESENTATION_RELATIONSHIP_WITH_TRANSFORMATION(#170)
SHAPE_REPRESENTATION_RELATIONSHIP()
);
#335=(
REPRESENTATION_RELATIONSHIP($,$,#63434,#63400)
REPRESENTATION_RELATIONSHIP_WITH_TRANSFORMATION(#171)
SHAPE_REPRESENTATION_RELATIONSHIP()
);
#336=(
REPRESENTATION_RELATIONSHIP($,$,#63434,#63400)
REPRESENTATION_RELATIONSHIP_WITH_TRANSFORMATION(#172)
SHAPE_REPRESENTATION_RELATIONSHIP()
);
#337=(
REPRESENTATION_RELATIONSHIP($,$,#63446,#63400)
REPRESENTATION_RELATIONSHIP_WITH_TRANSFORMATION(#173)
SHAPE_REPRESENTATION_RELATIONSHIP()
);
#338=(
REPRESENTATION_RELATIONSHIP($,$,#63446,#63400)
REPRESENTATION_RELATIONSHIP_WITH_TRANSFORMATION(#174)
SHAPE_REPRESENTATION_RELATIONSHIP()
);
#339=(
REPRESENTATION_RELATIONSHIP($,$,#63416,#63400)
REPRESENTATION_RELATIONSHIP_WITH_TRANSFORMATION(#175)
SHAPE_REPRESENTATION_RELATIONSHIP()
);
#340=(
REPRESENTATION_RELATIONSHIP($,$,#63434,#63400)
REPRESENTATION_RELATIONSHIP_WITH_TRANSFORMATION(#176)
SHAPE_REPRESENTATION_RELATIONSHIP()
);
#341=(
REPRESENTATION_RELATIONSHIP($,$,#63434,#63400)
REPRESENTATION_RELATIONSHIP_WITH_TRANSFORMATION(#177)
SHAPE_REPRESENTATION_RELATIONSHIP()
);
#342=(
REPRESENTATION_RELATIONSHIP($,$,#63434,#63400)
REPRESENTATION_RELATIONSHIP_WITH_TRANSFORMATION(#178)
SHAPE_REPRESENTATION_RELATIONSHIP()
);
#343=(
REPRESENTATION_RELATIONSHIP($,$,#63435,#63400)
REPRESENTATION_RELATIONSHIP_WITH_TRANSFORMATION(#179)
SHAPE_REPRESENTATION_RELATIONSHIP()
);
#344=(
REPRESENTATION_RELATIONSHIP($,$,#63435,#63400)
REPRESENTATION_RELATIONSHIP_WITH_TRANSFORMATION(#180)
SHAPE_REPRESENTATION_RELATIONSHIP()
);
#345=(
REPRESENTATION_RELATIONSHIP($,$,#63422,#63400)
REPRESENTATION_RELATIONSHIP_WITH_TRANSFORMATION(#181)
SHAPE_REPRESENTATION_RELATIONSHIP()
);
#346=(
REPRESENTATION_RELATIONSHIP($,$,#63422,#63400)
REPRESENTATION_RELATIONSHIP_WITH_TRANSFORMATION(#182)
SHAPE_REPRESENTATION_RELATIONSHIP()
);
#347=(
REPRESENTATION_RELATIONSHIP($,$,#63422,#63400)
REPRESENTATION_RELATIONSHIP_WITH_TRANSFORMATION(#183)
SHAPE_REPRESENTATION_RELATIONSHIP()
);
#348=(
REPRESENTATION_RELATIONSHIP($,$,#63422,#63400)
REPRESENTATION_RELATIONSHIP_WITH_TRANSFORMATION(#184)
SHAPE_REPRESENTATION_RELATIONSHIP()
);
#349=(
REPRESENTATION_RELATIONSHIP($,$,#63437,#63436)
REPRESENTATION_RELATIONSHIP_WITH_TRANSFORMATION(#185)
SHAPE_REPRESENTATION_RELATIONSHIP()
);
#350=(
REPRESENTATION_RELATIONSHIP($,$,#63438,#63436)
REPRESENTATION_RELATIONSHIP_WITH_TRANSFORMATION(#186)
SHAPE_REPRESENTATION_RELATIONSHIP()
);
#351=(
REPRESENTATION_RELATIONSHIP($,$,#63439,#63436)
REPRESENTATION_RELATIONSHIP_WITH_TRANSFORMATION(#187)
SHAPE_REPRESENTATION_RELATIONSHIP()
);
#352=(
REPRESENTATION_RELATIONSHIP($,$,#63440,#63436)
REPRESENTATION_RELATIONSHIP_WITH_TRANSFORMATION(#188)
SHAPE_REPRESENTATION_RELATIONSHIP()
);
#353=(
REPRESENTATION_RELATIONSHIP($,$,#63441,#63436)
REPRESENTATION_RELATIONSHIP_WITH_TRANSFORMATION(#189)
SHAPE_REPRESENTATION_RELATIONSHIP()
);
#354=(
REPRESENTATION_RELATIONSHIP($,$,#63442,#63436)
REPRESENTATION_RELATIONSHIP_WITH_TRANSFORMATION(#190)
SHAPE_REPRESENTATION_RELATIONSHIP()
);
#355=(
REPRESENTATION_RELATIONSHIP($,$,#63443,#63436)
REPRESENTATION_RELATIONSHIP_WITH_TRANSFORMATION(#191)
SHAPE_REPRESENTATION_RELATIONSHIP()
);
#356=(
REPRESENTATION_RELATIONSHIP($,$,#63444,#63436)
REPRESENTATION_RELATIONSHIP_WITH_TRANSFORMATION(#192)
SHAPE_REPRESENTATION_RELATIONSHIP()
);
#357=(
REPRESENTATION_RELATIONSHIP($,$,#63444,#63436)
REPRESENTATION_RELATIONSHIP_WITH_TRANSFORMATION(#193)
SHAPE_REPRESENTATION_RELATIONSHIP()
);
#358=(
REPRESENTATION_RELATIONSHIP($,$,#63445,#63436)
REPRESENTATION_RELATIONSHIP_WITH_TRANSFORMATION(#194)
SHAPE_REPRESENTATION_RELATIONSHIP()
);
#359=(
REPRESENTATION_RELATIONSHIP($,$,#63446,#63436)
REPRESENTATION_RELATIONSHIP_WITH_TRANSFORMATION(#195)
SHAPE_REPRESENTATION_RELATIONSHIP()
);
#360=(
REPRESENTATION_RELATIONSHIP($,$,#63400,#63399)
REPRESENTATION_RELATIONSHIP_WITH_TRANSFORMATION(#196)
SHAPE_REPRESENTATION_RELATIONSHIP()
);
#361=(
REPRESENTATION_RELATIONSHIP($,$,#63423,#63399)
REPRESENTATION_RELATIONSHIP_WITH_TRANSFORMATION(#197)
SHAPE_REPRESENTATION_RELATIONSHIP()
);
#362=(
REPRESENTATION_RELATIONSHIP($,$,#63436,#63399)
REPRESENTATION_RELATIONSHIP_WITH_TRANSFORMATION(#198)
SHAPE_REPRESENTATION_RELATIONSHIP()
);
#363=(
REPRESENTATION_RELATIONSHIP($,$,#63350,#63349)
REPRESENTATION_RELATIONSHIP_WITH_TRANSFORMATION(#199)
SHAPE_REPRESENTATION_RELATIONSHIP()
);
#364=(
REPRESENTATION_RELATIONSHIP($,$,#63399,#63349)
REPRESENTATION_RELATIONSHIP_WITH_TRANSFORMATION(#200)
SHAPE_REPRESENTATION_RELATIONSHIP()
);
#365=CONTEXT_DEPENDENT_SHAPE_REPRESENTATION(#201,#63107);
#366=CONTEXT_DEPENDENT_SHAPE_REPRESENTATION(#202,#63108);
#367=CONTEXT_DEPENDENT_SHAPE_REPRESENTATION(#203,#63109);
#368=CONTEXT_DEPENDENT_SHAPE_REPRESENTATION(#204,#63110);
#369=CONTEXT_DEPENDENT_SHAPE_REPRESENTATION(#205,#63111);
#370=CONTEXT_DEPENDENT_SHAPE_REPRESENTATION(#206,#63118);
#371=CONTEXT_DEPENDENT_SHAPE_REPRESENTATION(#207,#63119);
#372=CONTEXT_DEPENDENT_SHAPE_REPRESENTATION(#208,#63120);
#373=CONTEXT_DEPENDENT_SHAPE_REPRESENTATION(#209,#63121);
#374=CONTEXT_DEPENDENT_SHAPE_REPRESENTATION(#210,#63122);
#375=CONTEXT_DEPENDENT_SHAPE_REPRESENTATION(#211,#63131);
#376=CONTEXT_DEPENDENT_SHAPE_REPRESENTATION(#212,#63132);
#377=CONTEXT_DEPENDENT_SHAPE_REPRESENTATION(#213,#63133);
#378=CONTEXT_DEPENDENT_SHAPE_REPRESENTATION(#214,#63139);
#379=CONTEXT_DEPENDENT_SHAPE_REPRESENTATION(#215,#63140);
#380=CONTEXT_DEPENDENT_SHAPE_REPRESENTATION(#216,#63141);
#381=CONTEXT_DEPENDENT_SHAPE_REPRESENTATION(#217,#63142);
#382=CONTEXT_DEPENDENT_SHAPE_REPRESENTATION(#218,#63143);
#383=CONTEXT_DEPENDENT_SHAPE_REPRESENTATION(#219,#63144);
#384=CONTEXT_DEPENDENT_SHAPE_REPRESENTATION(#220,#63145);
#385=CONTEXT_DEPENDENT_SHAPE_REPRESENTATION(#221,#63146);
#386=CONTEXT_DEPENDENT_SHAPE_REPRESENTATION(#222,#63147);
#387=CONTEXT_DEPENDENT_SHAPE_REPRESENTATION(#223,#63148);
#388=CONTEXT_DEPENDENT_SHAPE_REPRESENTATION(#224,#63149);
#389=CONTEXT_DEPENDENT_SHAPE_REPRESENTATION(#225,#63150);
#390=CONTEXT_DEPENDENT_SHAPE_REPRESENTATION(#226,#63151);
#391=CONTEXT_DEPENDENT_SHAPE_REPRESENTATION(#227,#63152);
#392=CONTEXT_DEPENDENT_SHAPE_REPRESENTATION(#228,#63153);
#393=CONTEXT_DEPENDENT_SHAPE_REPRESENTATION(#229,#63154);
#394=CONTEXT_DEPENDENT_SHAPE_REPRESENTATION(#230,#63155);
#395=CONTEXT_DEPENDENT_SHAPE_REPRESENTATION(#231,#63156);
#396=CONTEXT_DEPENDENT_SHAPE_REPRESENTATION(#232,#63157);
#397=CONTEXT_DEPENDENT_SHAPE_REPRESENTATION(#233,#63158);
#398=CONTEXT_DEPENDENT_SHAPE_REPRESENTATION(#234,#63170);
#399=CONTEXT_DEPENDENT_SHAPE_REPRESENTATION(#235,#63171);
#400=CONTEXT_DEPENDENT_SHAPE_REPRESENTATION(#236,#63172);
#401=CONTEXT_DEPENDENT_SHAPE_REPRESENTATION(#237,#63173);
#402=CONTEXT_DEPENDENT_SHAPE_REPRESENTATION(#238,#63174);
#403=CONTEXT_DEPENDENT_SHAPE_REPRESENTATION(#239,#63175);
#404=CONTEXT_DEPENDENT_SHAPE_REPRESENTATION(#240,#63176);
#405=CONTEXT_DEPENDENT_SHAPE_REPRESENTATION(#241,#63177);
#406=CONTEXT_DEPENDENT_SHAPE_REPRESENTATION(#242,#63178);
#407=CONTEXT_DEPENDENT_SHAPE_REPRESENTATION(#243,#63179);
#408=CONTEXT_DEPENDENT_SHAPE_REPRESENTATION(#244,#63180);
#409=CONTEXT_DEPENDENT_SHAPE_REPRESENTATION(#245,#63181);
#410=CONTEXT_DEPENDENT_SHAPE_REPRESENTATION(#246,#63182);
#411=CONTEXT_DEPENDENT_SHAPE_REPRESENTATION(#247,#63183);
#412=CONTEXT_DEPENDENT_SHAPE_REPRESENTATION(#248,#63184);
#413=CONTEXT_DEPENDENT_SHAPE_REPRESENTATION(#249,#63185);
#414=CONTEXT_DEPENDENT_SHAPE_REPRESENTATION(#250,#63186);
#415=CONTEXT_DEPENDENT_SHAPE_REPRESENTATION(#251,#63187);
#416=CONTEXT_DEPENDENT_SHAPE_REPRESENTATION(#252,#63188);
#417=CONTEXT_DEPENDENT_SHAPE_REPRESENTATION(#253,#63189);
#418=CONTEXT_DEPENDENT_SHAPE_REPRESENTATION(#254,#63190);
#419=CONTEXT_DEPENDENT_SHAPE_REPRESENTATION(#255,#63191);
#420=CONTEXT_DEPENDENT_SHAPE_REPRESENTATION(#256,#63192);
#421=CONTEXT_DEPENDENT_SHAPE_REPRESENTATION(#257,#63193);
#422=CONTEXT_DEPENDENT_SHAPE_REPRESENTATION(#258,#63194);
#423=CONTEXT_DEPENDENT_SHAPE_REPRESENTATION(#259,#63195);
#424=CONTEXT_DEPENDENT_SHAPE_REPRESENTATION(#260,#63196);
#425=CONTEXT_DEPENDENT_SHAPE_REPRESENTATION(#261,#63197);
#426=CONTEXT_DEPENDENT_SHAPE_REPRESENTATION(#262,#63198);
#427=CONTEXT_DEPENDENT_SHAPE_REPRESENTATION(#263,#63199);
#428=CONTEXT_DEPENDENT_SHAPE_REPRESENTATION(#264,#63200);
#429=CONTEXT_DEPENDENT_SHAPE_REPRESENTATION(#265,#63201);
#430=CONTEXT_DEPENDENT_SHAPE_REPRESENTATION(#266,#63202);
#431=CONTEXT_DEPENDENT_SHAPE_REPRESENTATION(#267,#63203);
#432=CONTEXT_DEPENDENT_SHAPE_REPRESENTATION(#268,#63204);
#433=CONTEXT_DEPENDENT_SHAPE_REPRESENTATION(#269,#63205);
#434=CONTEXT_DEPENDENT_SHAPE_REPRESENTATION(#270,#63206);
#435=CONTEXT_DEPENDENT_SHAPE_REPRESENTATION(#271,#63207);
#436=CONTEXT_DEPENDENT_SHAPE_REPRESENTATION(#272,#63208);
#437=CONTEXT_DEPENDENT_SHAPE_REPRESENTATION(#273,#63209);
#438=CONTEXT_DEPENDENT_SHAPE_REPRESENTATION(#274,#63210);
#439=CONTEXT_DEPENDENT_SHAPE_REPRESENTATION(#275,#63211);
#440=CONTEXT_DEPENDENT_SHAPE_REPRESENTATION(#276,#63212);
#441=CONTEXT_DEPENDENT_SHAPE_REPRESENTATION(#277,#63213);
#442=CONTEXT_DEPENDENT_SHAPE_REPRESENTATION(#278,#63214);
#443=CONTEXT_DEPENDENT_SHAPE_REPRESENTATION(#279,#63215);
#444=CONTEXT_DEPENDENT_SHAPE_REPRESENTATION(#280,#63216);
#445=CONTEXT_DEPENDENT_SHAPE_REPRESENTATION(#281,#63234);
#446=CONTEXT_DEPENDENT_SHAPE_REPRESENTATION(#282,#63235);
#447=CONTEXT_DEPENDENT_SHAPE_REPRESENTATION(#283,#63236);
#448=CONTEXT_DEPENDENT_SHAPE_REPRESENTATION(#284,#63237);
#449=CONTEXT_DEPENDENT_SHAPE_REPRESENTATION(#285,#63238);
#450=CONTEXT_DEPENDENT_SHAPE_REPRESENTATION(#286,#63245);
#451=CONTEXT_DEPENDENT_SHAPE_REPRESENTATION(#287,#63246);
#452=CONTEXT_DEPENDENT_SHAPE_REPRESENTATION(#288,#63247);
#453=CONTEXT_DEPENDENT_SHAPE_REPRESENTATION(#289,#63248);
#454=CONTEXT_DEPENDENT_SHAPE_REPRESENTATION(#290,#63249);
#455=CONTEXT_DEPENDENT_SHAPE_REPRESENTATION(#291,#63259);
#456=CONTEXT_DEPENDENT_SHAPE_REPRESENTATION(#292,#63260);
#457=CONTEXT_DEPENDENT_SHAPE_REPRESENTATION(#293,#63261);
#458=CONTEXT_DEPENDENT_SHAPE_REPRESENTATION(#294,#63267);
#459=CONTEXT_DEPENDENT_SHAPE_REPRESENTATION(#295,#63268);
#460=CONTEXT_DEPENDENT_SHAPE_REPRESENTATION(#296,#63269);
#461=CONTEXT_DEPENDENT_SHAPE_REPRESENTATION(#297,#63270);
#462=CONTEXT_DEPENDENT_SHAPE_REPRESENTATION(#298,#63271);
#463=CONTEXT_DEPENDENT_SHAPE_REPRESENTATION(#299,#63272);
#464=CONTEXT_DEPENDENT_SHAPE_REPRESENTATION(#300,#63273);
#465=CONTEXT_DEPENDENT_SHAPE_REPRESENTATION(#301,#63274);
#466=CONTEXT_DEPENDENT_SHAPE_REPRESENTATION(#302,#63275);
#467=CONTEXT_DEPENDENT_SHAPE_REPRESENTATION(#303,#63276);
#468=CONTEXT_DEPENDENT_SHAPE_REPRESENTATION(#304,#63277);
#469=CONTEXT_DEPENDENT_SHAPE_REPRESENTATION(#305,#63278);
#470=CONTEXT_DEPENDENT_SHAPE_REPRESENTATION(#306,#63279);
#471=CONTEXT_DEPENDENT_SHAPE_REPRESENTATION(#307,#63280);
#472=CONTEXT_DEPENDENT_SHAPE_REPRESENTATION(#308,#63281);
#473=CONTEXT_DEPENDENT_SHAPE_REPRESENTATION(#309,#63282);
#474=CONTEXT_DEPENDENT_SHAPE_REPRESENTATION(#310,#63283);
#475=CONTEXT_DEPENDENT_SHAPE_REPRESENTATION(#311,#63284);
#476=CONTEXT_DEPENDENT_SHAPE_REPRESENTATION(#312,#63285);
#477=CONTEXT_DEPENDENT_SHAPE_REPRESENTATION(#313,#63286);
#478=CONTEXT_DEPENDENT_SHAPE_REPRESENTATION(#314,#63298);
#479=CONTEXT_DEPENDENT_SHAPE_REPRESENTATION(#315,#63299);
#480=CONTEXT_DEPENDENT_SHAPE_REPRESENTATION(#316,#63300);
#481=CONTEXT_DEPENDENT_SHAPE_REPRESENTATION(#317,#63301);
#482=CONTEXT_DEPENDENT_SHAPE_REPRESENTATION(#318,#63302);
#483=CONTEXT_DEPENDENT_SHAPE_REPRESENTATION(#319,#63303);
#484=CONTEXT_DEPENDENT_SHAPE_REPRESENTATION(#320,#63304);
#485=CONTEXT_DEPENDENT_SHAPE_REPRESENTATION(#321,#63305);
#486=CONTEXT_DEPENDENT_SHAPE_REPRESENTATION(#322,#63306);
#487=CONTEXT_DEPENDENT_SHAPE_REPRESENTATION(#323,#63307);
#488=CONTEXT_DEPENDENT_SHAPE_REPRESENTATION(#324,#63308);
#489=CONTEXT_DEPENDENT_SHAPE_REPRESENTATION(#325,#63309);
#490=CONTEXT_DEPENDENT_SHAPE_REPRESENTATION(#326,#63310);
#491=CONTEXT_DEPENDENT_SHAPE_REPRESENTATION(#327,#63311);
#492=CONTEXT_DEPENDENT_SHAPE_REPRESENTATION(#328,#63312);
#493=CONTEXT_DEPENDENT_SHAPE_REPRESENTATION(#329,#63313);
#494=CONTEXT_DEPENDENT_SHAPE_REPRESENTATION(#330,#63314);
#495=CONTEXT_DEPENDENT_SHAPE_REPRESENTATION(#331,#63315);
#496=CONTEXT_DEPENDENT_SHAPE_REPRESENTATION(#332,#63316);
#497=CONTEXT_DEPENDENT_SHAPE_REPRESENTATION(#333,#63317);
#498=CONTEXT_DEPENDENT_SHAPE_REPRESENTATION(#334,#63318);
#499=CONTEXT_DEPENDENT_SHAPE_REPRESENTATION(#335,#63319);
#500=CONTEXT_DEPENDENT_SHAPE_REPRESENTATION(#336,#63320);
#501=CONTEXT_DEPENDENT_SHAPE_REPRESENTATION(#337,#63321);
#502=CONTEXT_DEPENDENT_SHAPE_REPRESENTATION(#338,#63322);
#503=CONTEXT_DEPENDENT_SHAPE_REPRESENTATION(#339,#63323);
#504=CONTEXT_DEPENDENT_SHAPE_REPRESENTATION(#340,#63324);
#505=CONTEXT_DEPENDENT_SHAPE_REPRESENTATION(#341,#63325);
#506=CONTEXT_DEPENDENT_SHAPE_REPRESENTATION(#342,#63326);
#507=CONTEXT_DEPENDENT_SHAPE_REPRESENTATION(#343,#63327);
#508=CONTEXT_DEPENDENT_SHAPE_REPRESENTATION(#344,#63328);
#509=CONTEXT_DEPENDENT_SHAPE_REPRESENTATION(#345,#63329);
#510=CONTEXT_DEPENDENT_SHAPE_REPRESENTATION(#346,#63330);
#511=CONTEXT_DEPENDENT_SHAPE_REPRESENTATION(#347,#63331);
#512=CONTEXT_DEPENDENT_SHAPE_REPRESENTATION(#348,#63332);
#513=CONTEXT_DEPENDENT_SHAPE_REPRESENTATION(#349,#63333);
#514=CONTEXT_DEPENDENT_SHAPE_REPRESENTATION(#350,#63334);
#515=CONTEXT_DEPENDENT_SHAPE_REPRESENTATION(#351,#63335);
#516=CONTEXT_DEPENDENT_SHAPE_REPRESENTATION(#352,#63336);
#517=CONTEXT_DEPENDENT_SHAPE_REPRESENTATION(#353,#63337);
#518=CONTEXT_DEPENDENT_SHAPE_REPRESENTATION(#354,#63338);
#519=CONTEXT_DEPENDENT_SHAPE_REPRESENTATION(#355,#63339);
#520=CONTEXT_DEPENDENT_SHAPE_REPRESENTATION(#356,#63340);
#521=CONTEXT_DEPENDENT_SHAPE_REPRESENTATION(#357,#63341);
#522=CONTEXT_DEPENDENT_SHAPE_REPRESENTATION(#358,#63342);
#523=CONTEXT_DEPENDENT_SHAPE_REPRESENTATION(#359,#63343);
#524=CONTEXT_DEPENDENT_SHAPE_REPRESENTATION(#360,#63344);
#525=CONTEXT_DEPENDENT_SHAPE_REPRESENTATION(#361,#63345);
#526=CONTEXT_DEPENDENT_SHAPE_REPRESENTATION(#362,#63346);
#527=CONTEXT_DEPENDENT_SHAPE_REPRESENTATION(#363,#63347);
#528=CONTEXT_DEPENDENT_SHAPE_REPRESENTATION(#364,#63348);
#529=NEXT_ASSEMBLY_USAGE_OCCURRENCE('Inner ring:1','Inner ring:1',
'Inner ring:1',#63462,#63463,'Inner ring:1');
#530=NEXT_ASSEMBLY_USAGE_OCCURRENCE('Outer ring:1','Outer ring:1',
'Outer ring:1',#63462,#63464,'Outer ring:1');
#531=NEXT_ASSEMBLY_USAGE_OCCURRENCE('Balls:1','Balls:1','Balls:1',#63462,
#63465,'Balls:1');
#532=NEXT_ASSEMBLY_USAGE_OCCURRENCE('Cage:1','Cage:1','Cage:1',#63462,#63466,
'Cage:1');
#533=NEXT_ASSEMBLY_USAGE_OCCURRENCE('Seals 2RS:1','Seals 2RS:1',
'Seals 2RS:1',#63462,#63467,'Seals 2RS:1');
#534=NEXT_ASSEMBLY_USAGE_OCCURRENCE('Inner ring (1):1',
'Inner ring (1):1','Inner ring (1):1',#63468,#63469,'Inner ring (1):1');
#535=NEXT_ASSEMBLY_USAGE_OCCURRENCE('Outer ring (1):1',
'Outer ring (1):1','Outer ring (1):1',#63468,#63470,'Outer ring (1):1');
#536=NEXT_ASSEMBLY_USAGE_OCCURRENCE('Balls (1):1','Balls (1):1',
'Balls (1):1',#63468,#63471,'Balls (1):1');
#537=NEXT_ASSEMBLY_USAGE_OCCURRENCE('Cage (1):1','Cage (1):1',
'Cage (1):1',#63468,#63472,'Cage (1):1');
#538=NEXT_ASSEMBLY_USAGE_OCCURRENCE('Seals 2RS (1):1','Seals 2RS (1):1',
'Seals 2RS (1):1',#63468,#63473,'Seals 2RS (1):1');
#539=NEXT_ASSEMBLY_USAGE_OCCURRENCE('Block:1','Block:1','Block:1',#63478,
#63479,'Block:1');
#540=NEXT_ASSEMBLY_USAGE_OCCURRENCE('End cap +:1','End cap +:1',
'End cap +:1',#63478,#63480,'End cap +:1');
#541=NEXT_ASSEMBLY_USAGE_OCCURRENCE('End cap:1','End cap:1','End cap:1',
#63478,#63481,'End cap:1');
#542=NEXT_ASSEMBLY_USAGE_OCCURRENCE('X Stage - 05 Carriage spacer:1',
'X Stage - 05 Carriage spacer:1','X Stage - 05 Carriage spacer:1',#63474,
#63475,'X Stage - 05 Carriage spacer:1');
#543=NEXT_ASSEMBLY_USAGE_OCCURRENCE('X Stage - 06 Table:1',
'X Stage - 06 Table:1','X Stage - 06 Table:1',#63474,#63476,
'X Stage - 06 Table:1');
#544=NEXT_ASSEMBLY_USAGE_OCCURRENCE('X Stage - 07 Nut bracket:1',
'X Stage - 07 Nut bracket:1','X Stage - 07 Nut bracket:1',#63474,#63477,
'X Stage - 07 Nut bracket:1');
#545=NEXT_ASSEMBLY_USAGE_OCCURRENCE(
'Flanged Linear Guide Carriage - 15 mm:2',
'Flanged Linear Guide Carriage - 15 mm:2',
'Flanged Linear Guide Carriage - 15 mm:2',#63474,#63478,
'Flanged Linear Guide Carriage - 15 mm:2');
#546=NEXT_ASSEMBLY_USAGE_OCCURRENCE('Flat Washer - M5:2',
'Flat Washer - M5:2','Flat Washer - M5:2',#63474,#63482,
'Flat Washer - M5:2');
#547=NEXT_ASSEMBLY_USAGE_OCCURRENCE('M5x30 frame screw:2',
'M5x30 frame screw:2','M5x30 frame screw:2',#63474,#63483,
'M5x30 frame screw:2');
#548=NEXT_ASSEMBLY_USAGE_OCCURRENCE('Flat Washer - M5:3',
'Flat Washer - M5:3','Flat Washer - M5:3',#63474,#63482,
'Flat Washer - M5:3');
#549=NEXT_ASSEMBLY_USAGE_OCCURRENCE('M5x30 frame screw:3',
'M5x30 frame screw:3','M5x30 frame screw:3',#63474,#63483,
'M5x30 frame screw:3');
#550=NEXT_ASSEMBLY_USAGE_OCCURRENCE('Flat Washer - M5:4',
'Flat Washer - M5:4','Flat Washer - M5:4',#63474,#63482,
'Flat Washer - M5:4');
#551=NEXT_ASSEMBLY_USAGE_OCCURRENCE('M5x30 frame screw:4',
'M5x30 frame screw:4','M5x30 frame screw:4',#63474,#63483,
'M5x30 frame screw:4');
#552=NEXT_ASSEMBLY_USAGE_OCCURRENCE('Flat Washer - M5:5',
'Flat Washer - M5:5','Flat Washer - M5:5',#63474,#63482,
'Flat Washer - M5:5');
#553=NEXT_ASSEMBLY_USAGE_OCCURRENCE('M5x30 frame screw:5',
'M5x30 frame screw:5','M5x30 frame screw:5',#63474,#63483,
'M5x30 frame screw:5');
#554=NEXT_ASSEMBLY_USAGE_OCCURRENCE('Flanged lead nut:2',
'Flanged lead nut:2','Flanged lead nut:2',#63474,#63484,
'Flanged lead nut:2');
#555=NEXT_ASSEMBLY_USAGE_OCCURRENCE('Cap Screw - M4x16:6',
'Cap Screw - M4x16:6','Cap Screw - M4x16:6',#63474,#63485,
'Cap Screw - M4x16:6');
#556=NEXT_ASSEMBLY_USAGE_OCCURRENCE('Cap Screw - M4x16:7',
'Cap Screw - M4x16:7','Cap Screw - M4x16:7',#63474,#63485,
'Cap Screw - M4x16:7');
#557=NEXT_ASSEMBLY_USAGE_OCCURRENCE('Cap Screw - M4x16:8',
'Cap Screw - M4x16:8','Cap Screw - M4x16:8',#63474,#63485,
'Cap Screw - M4x16:8');
#558=NEXT_ASSEMBLY_USAGE_OCCURRENCE('Cap Screw - M5x20:6',
'Cap Screw - M5x20:6','Cap Screw - M5x20:6',#63474,#63486,
'Cap Screw - M5x20:6');
#559=NEXT_ASSEMBLY_USAGE_OCCURRENCE('Cap Screw - M5x20:7',
'Cap Screw - M5x20:7','Cap Screw - M5x20:7',#63474,#63486,
'Cap Screw - M5x20:7');
#560=NEXT_ASSEMBLY_USAGE_OCCURRENCE('Cap Screw - M5x20:8',
'Cap Screw - M5x20:8','Cap Screw - M5x20:8',#63474,#63486,
'Cap Screw - M5x20:8');
#561=NEXT_ASSEMBLY_USAGE_OCCURRENCE('Cap Screw - M5x20:9',
'Cap Screw - M5x20:9','Cap Screw - M5x20:9',#63474,#63486,
'Cap Screw - M5x20:9');
#562=NEXT_ASSEMBLY_USAGE_OCCURRENCE('X Stage - 02 Base:1',
'X Stage - 02 Base:1','X Stage - 02 Base:1',#63450,#63451,
'X Stage - 02 Base:1');
#563=NEXT_ASSEMBLY_USAGE_OCCURRENCE('X Stage - 03 Bonded skid:1',
'X Stage - 03 Bonded skid:1','X Stage - 03 Bonded skid:1',#63450,#63452,
'X Stage - 03 Bonded skid:1');
#564=NEXT_ASSEMBLY_USAGE_OCCURRENCE('X Stage - 03 Bonded skid (1):1',
'X Stage - 03 Bonded skid (1):1','X Stage - 03 Bonded skid (1):1',#63450,
#63453,'X Stage - 03 Bonded skid (1):1');
#565=NEXT_ASSEMBLY_USAGE_OCCURRENCE('X Stage - 04 Rail adapter:1',
'X Stage - 04 Rail adapter:1','X Stage - 04 Rail adapter:1',#63450,#63454,
'X Stage - 04 Rail adapter:1');
#566=NEXT_ASSEMBLY_USAGE_OCCURRENCE(
'X Stage - 08 Floating bearing support:1',
'X Stage - 08 Floating bearing support:1',
'X Stage - 08 Floating bearing support:1',#63450,#63455,
'X Stage - 08 Floating bearing support:1');
#567=NEXT_ASSEMBLY_USAGE_OCCURRENCE('X Stage - 10 Floating cap:1',
'X Stage - 10 Floating cap:1','X Stage - 10 Floating cap:1',#63450,#63456,
'X Stage - 10 Floating cap:1');
#568=NEXT_ASSEMBLY_USAGE_OCCURRENCE(
'X Stage - 09 Fixed bearing support:1',
'X Stage - 09 Fixed bearing support:1',
'X Stage - 09 Fixed bearing support:1',#63450,#63457,
'X Stage - 09 Fixed bearing support:1');
#569=NEXT_ASSEMBLY_USAGE_OCCURRENCE('X Stage - 11 Fixed cap:1',
'X Stage - 11 Fixed cap:1','X Stage - 11 Fixed cap:1',#63450,#63458,
'X Stage - 11 Fixed cap:1');
#570=NEXT_ASSEMBLY_USAGE_OCCURRENCE('X Stage - 12 End stop:1',
'X Stage - 12 End stop:1','X Stage - 12 End stop:1',#63450,#63459,
'X Stage - 12 End stop:1');
#571=NEXT_ASSEMBLY_USAGE_OCCURRENCE('X Stage - 12 End stop (1):1',
'X Stage - 12 End stop (1):1','X Stage - 12 End stop (1):1',#63450,#63460,
'X Stage - 12 End stop (1):1');
#572=NEXT_ASSEMBLY_USAGE_OCCURRENCE('Cap Screw - M5x20:2',
'Cap Screw - M5x20:2','Cap Screw - M5x20:2',#63450,#63486,
'Cap Screw - M5x20:2');
#573=NEXT_ASSEMBLY_USAGE_OCCURRENCE('Cap Screw - M5x20:3',
'Cap Screw - M5x20:3','Cap Screw - M5x20:3',#63450,#63486,
'Cap Screw - M5x20:3');
#574=NEXT_ASSEMBLY_USAGE_OCCURRENCE('Cap Screw - M5x20:4',
'Cap Screw - M5x20:4','Cap Screw - M5x20:4',#63450,#63486,
'Cap Screw - M5x20:4');
#575=NEXT_ASSEMBLY_USAGE_OCCURRENCE('Cap Screw - M5x20:5',
'Cap Screw - M5x20:5','Cap Screw - M5x20:5',#63450,#63486,
'Cap Screw - M5x20:5');
#576=NEXT_ASSEMBLY_USAGE_OCCURRENCE(
'Linear Guide Rail - 15 mm, 220 mm Long:2',
'Linear Guide Rail - 15 mm, 220 mm Long:2',
'Linear Guide Rail - 15 mm, 220 mm Long:2',#63450,#63461,
'Linear Guide Rail - 15 mm, 220 mm Long:2');
#577=NEXT_ASSEMBLY_USAGE_OCCURRENCE('Cap Screw - M4x16:2',
'Cap Screw - M4x16:2','Cap Screw - M4x16:2',#63450,#63485,
'Cap Screw - M4x16:2');
#578=NEXT_ASSEMBLY_USAGE_OCCURRENCE('Cap Screw - M4x16:3',
'Cap Screw - M4x16:3','Cap Screw - M4x16:3',#63450,#63485,
'Cap Screw - M4x16:3');
#579=NEXT_ASSEMBLY_USAGE_OCCURRENCE('Cap Screw - M4x16:4',
'Cap Screw - M4x16:4','Cap Screw - M4x16:4',#63450,#63485,
'Cap Screw - M4x16:4');
#580=NEXT_ASSEMBLY_USAGE_OCCURRENCE('Cap Screw - M4x16:5',
'Cap Screw - M4x16:5','Cap Screw - M4x16:5',#63450,#63485,
'Cap Screw - M4x16:5');
#581=NEXT_ASSEMBLY_USAGE_OCCURRENCE('Cap Screw - M5x20:10',
'Cap Screw - M5x20:10','Cap Screw - M5x20:10',#63450,#63486,
'Cap Screw - M5x20:10');
#582=NEXT_ASSEMBLY_USAGE_OCCURRENCE('Cap Screw - M5x20:11',
'Cap Screw - M5x20:11','Cap Screw - M5x20:11',#63450,#63486,
'Cap Screw - M5x20:11');
#583=NEXT_ASSEMBLY_USAGE_OCCURRENCE(
'Sealed Ball Bearing - 12 x 32 x 10 mm:2',
'Sealed Ball Bearing - 12 x 32 x 10 mm:2',
'Sealed Ball Bearing - 12 x 32 x 10 mm:2',#63450,#63462,
'Sealed Ball Bearing - 12 x 32 x 10 mm:2');
#584=NEXT_ASSEMBLY_USAGE_OCCURRENCE('Cap Screw - M4x16:9',
'Cap Screw - M4x16:9','Cap Screw - M4x16:9',#63450,#63485,
'Cap Screw - M4x16:9');
#585=NEXT_ASSEMBLY_USAGE_OCCURRENCE('Cap Screw - M4x16:10',
'Cap Screw - M4x16:10','Cap Screw - M4x16:10',#63450,#63485,
'Cap Screw - M4x16:10');
#586=NEXT_ASSEMBLY_USAGE_OCCURRENCE('Cap Screw - M4x16:11',
'Cap Screw - M4x16:11','Cap Screw - M4x16:11',#63450,#63485,
'Cap Screw - M4x16:11');
#587=NEXT_ASSEMBLY_USAGE_OCCURRENCE('Cap Screw - M6x25:2',
'Cap Screw - M6x25:2','Cap Screw - M6x25:2',#63450,#63497,
'Cap Screw - M6x25:2');
#588=NEXT_ASSEMBLY_USAGE_OCCURRENCE('Cap Screw - M6x25:3',
'Cap Screw - M6x25:3','Cap Screw - M6x25:3',#63450,#63497,
'Cap Screw - M6x25:3');
#589=NEXT_ASSEMBLY_USAGE_OCCURRENCE(
'Sealed Ball Bearing - 20 x 47 x 14 mm:2',
'Sealed Ball Bearing - 20 x 47 x 14 mm:2',
'Sealed Ball Bearing - 20 x 47 x 14 mm:2',#63450,#63468,
'Sealed Ball Bearing - 20 x 47 x 14 mm:2');
#590=NEXT_ASSEMBLY_USAGE_OCCURRENCE('Cap Screw - M4x16:12',
'Cap Screw - M4x16:12','Cap Screw - M4x16:12',#63450,#63485,
'Cap Screw - M4x16:12');
#591=NEXT_ASSEMBLY_USAGE_OCCURRENCE('Cap Screw - M4x16:13',
'Cap Screw - M4x16:13','Cap Screw - M4x16:13',#63450,#63485,
'Cap Screw - M4x16:13');
#592=NEXT_ASSEMBLY_USAGE_OCCURRENCE('Cap Screw - M4x16:14',
'Cap Screw - M4x16:14','Cap Screw - M4x16:14',#63450,#63485,
'Cap Screw - M4x16:14');
#593=NEXT_ASSEMBLY_USAGE_OCCURRENCE('Cap Screw - M5x20:12',
'Cap Screw - M5x20:12','Cap Screw - M5x20:12',#63450,#63486,
'Cap Screw - M5x20:12');
#594=NEXT_ASSEMBLY_USAGE_OCCURRENCE('Cap Screw - M5x20:13',
'Cap Screw - M5x20:13','Cap Screw - M5x20:13',#63450,#63486,
'Cap Screw - M5x20:13');
#595=NEXT_ASSEMBLY_USAGE_OCCURRENCE(
'X Stage - 01 Supported TR12x3 screw:2',
'X Stage - 01 Supported TR12x3 screw:2',
'X Stage - 01 Supported TR12x3 screw:2',#63487,#63488,
'X Stage - 01 Supported TR12x3 screw:2');
#596=NEXT_ASSEMBLY_USAGE_OCCURRENCE('Inner race spacer:2',
'Inner race spacer:2','Inner race spacer:2',#63487,#63489,
'Inner race spacer:2');
#597=NEXT_ASSEMBLY_USAGE_OCCURRENCE('Shaft retaining collar:2',
'Shaft retaining collar:2','Shaft retaining collar:2',#63487,#63490,
'Shaft retaining collar:2');
#598=NEXT_ASSEMBLY_USAGE_OCCURRENCE('Handwheel:2','Handwheel:2',
'Handwheel:2',#63487,#63491,'Handwheel:2');
#599=NEXT_ASSEMBLY_USAGE_OCCURRENCE('Handle pivot sleeve:2',
'Handle pivot sleeve:2','Handle pivot sleeve:2',#63487,#63492,
'Handle pivot sleeve:2');
#600=NEXT_ASSEMBLY_USAGE_OCCURRENCE('Revolving handle:2',
'Revolving handle:2','Revolving handle:2',#63487,#63493,
'Revolving handle:2');
#601=NEXT_ASSEMBLY_USAGE_OCCURRENCE('Key 6x6x20:2','Key 6x6x20:2',
'Key 6x6x20:2',#63487,#63494,'Key 6x6x20:2');
#602=NEXT_ASSEMBLY_USAGE_OCCURRENCE('Socket Set Screw - M5x8:2',
'Socket Set Screw - M5x8:2','Socket Set Screw - M5x8:2',#63487,#63495,
'Socket Set Screw - M5x8:2');
#603=NEXT_ASSEMBLY_USAGE_OCCURRENCE('Socket Set Screw - M5x8:3',
'Socket Set Screw - M5x8:3','Socket Set Screw - M5x8:3',#63487,#63495,
'Socket Set Screw - M5x8:3');
#604=NEXT_ASSEMBLY_USAGE_OCCURRENCE('Flat Washer - M6:2',
'Flat Washer - M6:2','Flat Washer - M6:2',#63487,#63496,
'Flat Washer - M6:2');
#605=NEXT_ASSEMBLY_USAGE_OCCURRENCE('Cap Screw - M6x25:4',
'Cap Screw - M6x25:4','Cap Screw - M6x25:4',#63487,#63497,
'Cap Screw - M6x25:4');
#606=NEXT_ASSEMBLY_USAGE_OCCURRENCE('Rail and screw supports:1',
'Rail and screw supports:1','Rail and screw supports:1',#63449,#63450,
'Rail and screw supports:1');
#607=NEXT_ASSEMBLY_USAGE_OCCURRENCE('Moving table and nut:1',
'Moving table and nut:1','Moving table and nut:1',#63449,#63474,
'Moving table and nut:1');
#608=NEXT_ASSEMBLY_USAGE_OCCURRENCE('Lead screw and handwheel:1',
'Lead screw and handwheel:1','Lead screw and handwheel:1',#63449,#63487,
'Lead screw and handwheel:1');
#609=NEXT_ASSEMBLY_USAGE_OCCURRENCE('Inner ring (2):1',
'Inner ring (2):1','Inner ring (2):1',#63509,#63510,'Inner ring (2):1');
#610=NEXT_ASSEMBLY_USAGE_OCCURRENCE('Outer ring (2):1',
'Outer ring (2):1','Outer ring (2):1',#63509,#63511,'Outer ring (2):1');
#611=NEXT_ASSEMBLY_USAGE_OCCURRENCE('Balls (2):1','Balls (2):1',
'Balls (2):1',#63509,#63512,'Balls (2):1');
#612=NEXT_ASSEMBLY_USAGE_OCCURRENCE('Cage (2):1','Cage (2):1',
'Cage (2):1',#63509,#63513,'Cage (2):1');
#613=NEXT_ASSEMBLY_USAGE_OCCURRENCE('Seals 2RS (2):1','Seals 2RS (2):1',
'Seals 2RS (2):1',#63509,#63514,'Seals 2RS (2):1');
#614=NEXT_ASSEMBLY_USAGE_OCCURRENCE('Inner ring (1) (1):1',
'Inner ring (1) (1):1','Inner ring (1) (1):1',#63515,#63516,
'Inner ring (1) (1):1');
#615=NEXT_ASSEMBLY_USAGE_OCCURRENCE('Outer ring (1) (1):1',
'Outer ring (1) (1):1','Outer ring (1) (1):1',#63515,#63517,
'Outer ring (1) (1):1');
#616=NEXT_ASSEMBLY_USAGE_OCCURRENCE('Balls (1) (1):1','Balls (1) (1):1',
'Balls (1) (1):1',#63515,#63518,'Balls (1) (1):1');
#617=NEXT_ASSEMBLY_USAGE_OCCURRENCE('Cage (1) (1):1','Cage (1) (1):1',
'Cage (1) (1):1',#63515,#63519,'Cage (1) (1):1');
#618=NEXT_ASSEMBLY_USAGE_OCCURRENCE('Seals 2RS (1) (1):1',
'Seals 2RS (1) (1):1','Seals 2RS (1) (1):1',#63515,#63520,
'Seals 2RS (1) (1):1');
#619=NEXT_ASSEMBLY_USAGE_OCCURRENCE('Block (1):1','Block (1):1',
'Block (1):1',#63526,#63527,'Block (1):1');
#620=NEXT_ASSEMBLY_USAGE_OCCURRENCE('End cap + (1):1','End cap + (1):1',
'End cap + (1):1',#63526,#63528,'End cap + (1):1');
#621=NEXT_ASSEMBLY_USAGE_OCCURRENCE('End cap (1):1','End cap (1):1',
'End cap (1):1',#63526,#63529,'End cap (1):1');
#622=NEXT_ASSEMBLY_USAGE_OCCURRENCE('Y Stage - 05 Carriage spacer:1',
'Y Stage - 05 Carriage spacer:1','Y Stage - 05 Carriage spacer:1',#63522,
#63523,'Y Stage - 05 Carriage spacer:1');
#623=NEXT_ASSEMBLY_USAGE_OCCURRENCE('Y Stage - 06 Table:1',
'Y Stage - 06 Table:1','Y Stage - 06 Table:1',#63522,#63524,
'Y Stage - 06 Table:1');
#624=NEXT_ASSEMBLY_USAGE_OCCURRENCE('Y Stage - 07 Nut bracket:1',
'Y Stage - 07 Nut bracket:1','Y Stage - 07 Nut bracket:1',#63522,#63525,
'Y Stage - 07 Nut bracket:1');
#625=NEXT_ASSEMBLY_USAGE_OCCURRENCE(
'Flanged Linear Guide Carriage - 15 mm (1):2',
'Flanged Linear Guide Carriage - 15 mm (1):2',
'Flanged Linear Guide Carriage - 15 mm (1):2',#63522,#63526,
'Flanged Linear Guide Carriage - 15 mm (1):2');
#626=NEXT_ASSEMBLY_USAGE_OCCURRENCE('Flat Washer - M5 (1):2',
'Flat Washer - M5 (1):2','Flat Washer - M5 (1):2',#63522,#63530,
'Flat Washer - M5 (1):2');
#627=NEXT_ASSEMBLY_USAGE_OCCURRENCE('M5x30 frame screw (1):2',
'M5x30 frame screw (1):2','M5x30 frame screw (1):2',#63522,#63531,
'M5x30 frame screw (1):2');
#628=NEXT_ASSEMBLY_USAGE_OCCURRENCE('Flat Washer - M5 (1):3',
'Flat Washer - M5 (1):3','Flat Washer - M5 (1):3',#63522,#63530,
'Flat Washer - M5 (1):3');
#629=NEXT_ASSEMBLY_USAGE_OCCURRENCE('M5x30 frame screw (1):3',
'M5x30 frame screw (1):3','M5x30 frame screw (1):3',#63522,#63531,
'M5x30 frame screw (1):3');
#630=NEXT_ASSEMBLY_USAGE_OCCURRENCE('Flat Washer - M5 (1):4',
'Flat Washer - M5 (1):4','Flat Washer - M5 (1):4',#63522,#63530,
'Flat Washer - M5 (1):4');
#631=NEXT_ASSEMBLY_USAGE_OCCURRENCE('M5x30 frame screw (1):4',
'M5x30 frame screw (1):4','M5x30 frame screw (1):4',#63522,#63531,
'M5x30 frame screw (1):4');
#632=NEXT_ASSEMBLY_USAGE_OCCURRENCE('Flat Washer - M5 (1):5',
'Flat Washer - M5 (1):5','Flat Washer - M5 (1):5',#63522,#63530,
'Flat Washer - M5 (1):5');
#633=NEXT_ASSEMBLY_USAGE_OCCURRENCE('M5x30 frame screw (1):5',
'M5x30 frame screw (1):5','M5x30 frame screw (1):5',#63522,#63531,
'M5x30 frame screw (1):5');
#634=NEXT_ASSEMBLY_USAGE_OCCURRENCE('Flanged lead nut (1):2',
'Flanged lead nut (1):2','Flanged lead nut (1):2',#63522,#63532,
'Flanged lead nut (1):2');
#635=NEXT_ASSEMBLY_USAGE_OCCURRENCE('Cap Screw - M4x16 (1):6',
'Cap Screw - M4x16 (1):6','Cap Screw - M4x16 (1):6',#63522,#63533,
'Cap Screw - M4x16 (1):6');
#636=NEXT_ASSEMBLY_USAGE_OCCURRENCE('Cap Screw - M4x16 (1):7',
'Cap Screw - M4x16 (1):7','Cap Screw - M4x16 (1):7',#63522,#63533,
'Cap Screw - M4x16 (1):7');
#637=NEXT_ASSEMBLY_USAGE_OCCURRENCE('Cap Screw - M4x16 (1):8',
'Cap Screw - M4x16 (1):8','Cap Screw - M4x16 (1):8',#63522,#63533,
'Cap Screw - M4x16 (1):8');
#638=NEXT_ASSEMBLY_USAGE_OCCURRENCE('Cap Screw - M5x20 (1):6',
'Cap Screw - M5x20 (1):6','Cap Screw - M5x20 (1):6',#63522,#63534,
'Cap Screw - M5x20 (1):6');
#639=NEXT_ASSEMBLY_USAGE_OCCURRENCE('Cap Screw - M5x20 (1):7',
'Cap Screw - M5x20 (1):7','Cap Screw - M5x20 (1):7',#63522,#63534,
'Cap Screw - M5x20 (1):7');
#640=NEXT_ASSEMBLY_USAGE_OCCURRENCE('Cap Screw - M5x20 (1):8',
'Cap Screw - M5x20 (1):8','Cap Screw - M5x20 (1):8',#63522,#63534,
'Cap Screw - M5x20 (1):8');
#641=NEXT_ASSEMBLY_USAGE_OCCURRENCE('Cap Screw - M5x20 (1):9',
'Cap Screw - M5x20 (1):9','Cap Screw - M5x20 (1):9',#63522,#63534,
'Cap Screw - M5x20 (1):9');
#642=NEXT_ASSEMBLY_USAGE_OCCURRENCE('Y Stage - 02 Base:1',
'Y Stage - 02 Base:1','Y Stage - 02 Base:1',#63499,#63500,
'Y Stage - 02 Base:1');
#643=NEXT_ASSEMBLY_USAGE_OCCURRENCE('Y Stage - 04 Rail adapter:1',
'Y Stage - 04 Rail adapter:1','Y Stage - 04 Rail adapter:1',#63499,#63501,
'Y Stage - 04 Rail adapter:1');
#644=NEXT_ASSEMBLY_USAGE_OCCURRENCE(
'Y Stage - 08 Floating bearing support:1',
'Y Stage - 08 Floating bearing support:1',
'Y Stage - 08 Floating bearing support:1',#63499,#63502,
'Y Stage - 08 Floating bearing support:1');
#645=NEXT_ASSEMBLY_USAGE_OCCURRENCE('Y Stage - 10 Floating cap:1',
'Y Stage - 10 Floating cap:1','Y Stage - 10 Floating cap:1',#63499,#63503,
'Y Stage - 10 Floating cap:1');
#646=NEXT_ASSEMBLY_USAGE_OCCURRENCE(
'Y Stage - 09 Fixed bearing support:1',
'Y Stage - 09 Fixed bearing support:1',
'Y Stage - 09 Fixed bearing support:1',#63499,#63504,
'Y Stage - 09 Fixed bearing support:1');
#647=NEXT_ASSEMBLY_USAGE_OCCURRENCE('Y Stage - 11 Fixed cap:1',
'Y Stage - 11 Fixed cap:1','Y Stage - 11 Fixed cap:1',#63499,#63505,
'Y Stage - 11 Fixed cap:1');
#648=NEXT_ASSEMBLY_USAGE_OCCURRENCE('Y Stage - 12 End stop:1',
'Y Stage - 12 End stop:1','Y Stage - 12 End stop:1',#63499,#63506,
'Y Stage - 12 End stop:1');
#649=NEXT_ASSEMBLY_USAGE_OCCURRENCE('Y Stage - 12 End stop (1):1',
'Y Stage - 12 End stop (1):1','Y Stage - 12 End stop (1):1',#63499,#63507,
'Y Stage - 12 End stop (1):1');
#650=NEXT_ASSEMBLY_USAGE_OCCURRENCE('Cap Screw - M5x20 (1):2',
'Cap Screw - M5x20 (1):2','Cap Screw - M5x20 (1):2',#63499,#63534,
'Cap Screw - M5x20 (1):2');
#651=NEXT_ASSEMBLY_USAGE_OCCURRENCE('Cap Screw - M5x20 (1):3',
'Cap Screw - M5x20 (1):3','Cap Screw - M5x20 (1):3',#63499,#63534,
'Cap Screw - M5x20 (1):3');
#652=NEXT_ASSEMBLY_USAGE_OCCURRENCE('Cap Screw - M5x20 (1):4',
'Cap Screw - M5x20 (1):4','Cap Screw - M5x20 (1):4',#63499,#63534,
'Cap Screw - M5x20 (1):4');
#653=NEXT_ASSEMBLY_USAGE_OCCURRENCE('Cap Screw - M5x20 (1):5',
'Cap Screw - M5x20 (1):5','Cap Screw - M5x20 (1):5',#63499,#63534,
'Cap Screw - M5x20 (1):5');
#654=NEXT_ASSEMBLY_USAGE_OCCURRENCE(
'Linear Guide Rail - 15 mm, 220 mm Long (1):2',
'Linear Guide Rail - 15 mm, 220 mm Long (1):2',
'Linear Guide Rail - 15 mm, 220 mm Long (1):2',#63499,#63508,
'Linear Guide Rail - 15 mm, 220 mm Long (1):2');
#655=NEXT_ASSEMBLY_USAGE_OCCURRENCE('Cap Screw - M4x16 (1):2',
'Cap Screw - M4x16 (1):2','Cap Screw - M4x16 (1):2',#63499,#63533,
'Cap Screw - M4x16 (1):2');
#656=NEXT_ASSEMBLY_USAGE_OCCURRENCE('Cap Screw - M4x16 (1):3',
'Cap Screw - M4x16 (1):3','Cap Screw - M4x16 (1):3',#63499,#63533,
'Cap Screw - M4x16 (1):3');
#657=NEXT_ASSEMBLY_USAGE_OCCURRENCE('Cap Screw - M4x16 (1):4',
'Cap Screw - M4x16 (1):4','Cap Screw - M4x16 (1):4',#63499,#63533,
'Cap Screw - M4x16 (1):4');
#658=NEXT_ASSEMBLY_USAGE_OCCURRENCE('Cap Screw - M4x16 (1):5',
'Cap Screw - M4x16 (1):5','Cap Screw - M4x16 (1):5',#63499,#63533,
'Cap Screw - M4x16 (1):5');
#659=NEXT_ASSEMBLY_USAGE_OCCURRENCE('Cap Screw - M5x20 (1):10',
'Cap Screw - M5x20 (1):10','Cap Screw - M5x20 (1):10',#63499,#63534,
'Cap Screw - M5x20 (1):10');
#660=NEXT_ASSEMBLY_USAGE_OCCURRENCE('Cap Screw - M5x20 (1):11',
'Cap Screw - M5x20 (1):11','Cap Screw - M5x20 (1):11',#63499,#63534,
'Cap Screw - M5x20 (1):11');
#661=NEXT_ASSEMBLY_USAGE_OCCURRENCE(
'Sealed Ball Bearing - 12 x 32 x 10 mm (1):2',
'Sealed Ball Bearing - 12 x 32 x 10 mm (1):2',
'Sealed Ball Bearing - 12 x 32 x 10 mm (1):2',#63499,#63509,
'Sealed Ball Bearing - 12 x 32 x 10 mm (1):2');
#662=NEXT_ASSEMBLY_USAGE_OCCURRENCE('Cap Screw - M4x16 (1):9',
'Cap Screw - M4x16 (1):9','Cap Screw - M4x16 (1):9',#63499,#63533,
'Cap Screw - M4x16 (1):9');
#663=NEXT_ASSEMBLY_USAGE_OCCURRENCE('Cap Screw - M4x16 (1):10',
'Cap Screw - M4x16 (1):10','Cap Screw - M4x16 (1):10',#63499,#63533,
'Cap Screw - M4x16 (1):10');
#664=NEXT_ASSEMBLY_USAGE_OCCURRENCE('Cap Screw - M4x16 (1):11',
'Cap Screw - M4x16 (1):11','Cap Screw - M4x16 (1):11',#63499,#63533,
'Cap Screw - M4x16 (1):11');
#665=NEXT_ASSEMBLY_USAGE_OCCURRENCE('Cap Screw - M6x25 (1):2',
'Cap Screw - M6x25 (1):2','Cap Screw - M6x25 (1):2',#63499,#63545,
'Cap Screw - M6x25 (1):2');
#666=NEXT_ASSEMBLY_USAGE_OCCURRENCE('Cap Screw - M6x25 (1):3',
'Cap Screw - M6x25 (1):3','Cap Screw - M6x25 (1):3',#63499,#63545,
'Cap Screw - M6x25 (1):3');
#667=NEXT_ASSEMBLY_USAGE_OCCURRENCE(
'Sealed Ball Bearing - 20 x 47 x 14 mm (1):2',
'Sealed Ball Bearing - 20 x 47 x 14 mm (1):2',
'Sealed Ball Bearing - 20 x 47 x 14 mm (1):2',#63499,#63515,
'Sealed Ball Bearing - 20 x 47 x 14 mm (1):2');
#668=NEXT_ASSEMBLY_USAGE_OCCURRENCE('Cap Screw - M4x16 (1):12',
'Cap Screw - M4x16 (1):12','Cap Screw - M4x16 (1):12',#63499,#63533,
'Cap Screw - M4x16 (1):12');
#669=NEXT_ASSEMBLY_USAGE_OCCURRENCE('Cap Screw - M4x16 (1):13',
'Cap Screw - M4x16 (1):13','Cap Screw - M4x16 (1):13',#63499,#63533,
'Cap Screw - M4x16 (1):13');
#670=NEXT_ASSEMBLY_USAGE_OCCURRENCE('Cap Screw - M4x16 (1):14',
'Cap Screw - M4x16 (1):14','Cap Screw - M4x16 (1):14',#63499,#63533,
'Cap Screw - M4x16 (1):14');
#671=NEXT_ASSEMBLY_USAGE_OCCURRENCE('Cap Screw - M5x20 (1):12',
'Cap Screw - M5x20 (1):12','Cap Screw - M5x20 (1):12',#63499,#63534,
'Cap Screw - M5x20 (1):12');
#672=NEXT_ASSEMBLY_USAGE_OCCURRENCE('Cap Screw - M5x20 (1):13',
'Cap Screw - M5x20 (1):13','Cap Screw - M5x20 (1):13',#63499,#63534,
'Cap Screw - M5x20 (1):13');
#673=NEXT_ASSEMBLY_USAGE_OCCURRENCE('M5x14 Cap Screw:2',
'M5x14 Cap Screw:2','M5x14 Cap Screw:2',#63499,#63521,
'M5x14 Cap Screw:2');
#674=NEXT_ASSEMBLY_USAGE_OCCURRENCE('M5x14 Cap Screw:3',
'M5x14 Cap Screw:3','M5x14 Cap Screw:3',#63499,#63521,
'M5x14 Cap Screw:3');
#675=NEXT_ASSEMBLY_USAGE_OCCURRENCE('M5x14 Cap Screw:4',
'M5x14 Cap Screw:4','M5x14 Cap Screw:4',#63499,#63521,
'M5x14 Cap Screw:4');
#676=NEXT_ASSEMBLY_USAGE_OCCURRENCE('M5x14 Cap Screw:5',
'M5x14 Cap Screw:5','M5x14 Cap Screw:5',#63499,#63521,
'M5x14 Cap Screw:5');
#677=NEXT_ASSEMBLY_USAGE_OCCURRENCE(
'Y Stage - 01 Supported TR12x3 screw:2',
'Y Stage - 01 Supported TR12x3 screw:2',
'Y Stage - 01 Supported TR12x3 screw:2',#63535,#63536,
'Y Stage - 01 Supported TR12x3 screw:2');
#678=NEXT_ASSEMBLY_USAGE_OCCURRENCE('Inner race spacer (1):2',
'Inner race spacer (1):2','Inner race spacer (1):2',#63535,#63537,
'Inner race spacer (1):2');
#679=NEXT_ASSEMBLY_USAGE_OCCURRENCE('Shaft retaining collar (1):2',
'Shaft retaining collar (1):2','Shaft retaining collar (1):2',#63535,#63538,
'Shaft retaining collar (1):2');
#680=NEXT_ASSEMBLY_USAGE_OCCURRENCE('Handwheel (1):2','Handwheel (1):2',
'Handwheel (1):2',#63535,#63539,'Handwheel (1):2');
#681=NEXT_ASSEMBLY_USAGE_OCCURRENCE('Handle pivot sleeve (1):2',
'Handle pivot sleeve (1):2','Handle pivot sleeve (1):2',#63535,#63540,
'Handle pivot sleeve (1):2');
#682=NEXT_ASSEMBLY_USAGE_OCCURRENCE('Revolving handle (1):2',
'Revolving handle (1):2','Revolving handle (1):2',#63535,#63541,
'Revolving handle (1):2');
#683=NEXT_ASSEMBLY_USAGE_OCCURRENCE('Key 6x6x20 (1):2',
'Key 6x6x20 (1):2','Key 6x6x20 (1):2',#63535,#63542,'Key 6x6x20 (1):2');
#684=NEXT_ASSEMBLY_USAGE_OCCURRENCE('Socket Set Screw - M5x8 (1):2',
'Socket Set Screw - M5x8 (1):2','Socket Set Screw - M5x8 (1):2',#63535,
#63543,'Socket Set Screw - M5x8 (1):2');
#685=NEXT_ASSEMBLY_USAGE_OCCURRENCE('Socket Set Screw - M5x8 (1):3',
'Socket Set Screw - M5x8 (1):3','Socket Set Screw - M5x8 (1):3',#63535,
#63543,'Socket Set Screw - M5x8 (1):3');
#686=NEXT_ASSEMBLY_USAGE_OCCURRENCE('Flat Washer - M6 (1):2',
'Flat Washer - M6 (1):2','Flat Washer - M6 (1):2',#63535,#63544,
'Flat Washer - M6 (1):2');
#687=NEXT_ASSEMBLY_USAGE_OCCURRENCE('Cap Screw - M6x25 (1):4',
'Cap Screw - M6x25 (1):4','Cap Screw - M6x25 (1):4',#63535,#63545,
'Cap Screw - M6x25 (1):4');
#688=NEXT_ASSEMBLY_USAGE_OCCURRENCE('Rail and screw supports (1):1',
'Rail and screw supports (1):1','Rail and screw supports (1):1',#63498,
#63499,'Rail and screw supports (1):1');
#689=NEXT_ASSEMBLY_USAGE_OCCURRENCE('Moving table and nut (1):1',
'Moving table and nut (1):1','Moving table and nut (1):1',#63498,#63522,
'Moving table and nut (1):1');
#690=NEXT_ASSEMBLY_USAGE_OCCURRENCE('Lead screw and handwheel (1):1',
'Lead screw and handwheel (1):1','Lead screw and handwheel (1):1',#63498,
#63535,'Lead screw and handwheel (1):1');
#691=NEXT_ASSEMBLY_USAGE_OCCURRENCE('X feed stage:1','X feed stage:1',
'X feed stage:1',#63448,#63449,'X feed stage:1');
#692=NEXT_ASSEMBLY_USAGE_OCCURRENCE('Y feed stage:1','Y feed stage:1',
'Y feed stage:1',#63448,#63498,'Y feed stage:1');
#693=B_SPLINE_CURVE_WITH_KNOTS('',3,(#33674,#33675,#33676,#33677,#33678,
#33679,#33680,#33681,#33682,#33683,#33684,#33685,#33686,#33687,#33688,#33689,
#33690,#33691,#33692,#33693,#33694,#33695),.UNSPECIFIED.,.F.,.F.,(4,2,2,
2,2,2,2,2,2,2,4),(0.0591825211272536,0.157966726598481,0.236950089897721,
0.315933453196962,0.391576304923761,0.46721915665056,0.54286200837736,0.618504860104159,
0.697488223403399,0.77647158670264,0.875255792173867),.UNSPECIFIED.);
#694=B_SPLINE_CURVE_WITH_KNOTS('',3,(#33699,#33700,#33701,#33702,#33703,
#33704,#33705,#33706,#33707,#33708,#33709,#33710,#33711,#33712,#33713,#33714,
#33715,#33716,#33717,#33718,#33719,#33720),.UNSPECIFIED.,.F.,.F.,(4,2,2,
2,2,2,2,2,2,2,4),(0.0581119756758434,0.106553146291161,0.213106292582322,
0.30849933801665,0.386091982889075,0.4636846277615,0.541277272633925,0.61886991750635,
0.714262962940678,0.820816109231839,0.869257279847157),.UNSPECIFIED.);
#695=B_SPLINE_CURVE_WITH_KNOTS('',3,(#33726,#33727,#33728,#33729,#33730,
#33731,#33732,#33733,#33734,#33735,#33736,#33737,#33738,#33739,#33740,#33741,
#33742,#33743,#33744,#33745,#33746,#33747),.UNSPECIFIED.,.F.,.F.,(4,2,2,
2,2,2,2,2,2,2,4),(0.0581119756758434,0.106553146291161,0.213106292582322,
0.30849933801665,0.386091982889075,0.4636846277615,0.541277272633925,0.61886991750635,
0.714262962940679,0.820816109231839,0.869257279847157),.UNSPECIFIED.);
#696=B_SPLINE_CURVE_WITH_KNOTS('',3,(#33751,#33752,#33753,#33754,#33755,
#33756,#33757,#33758,#33759,#33760,#33761,#33762,#33763,#33764,#33765,#33766,
#33767,#33768,#33769,#33770,#33771,#33772),.UNSPECIFIED.,.F.,.F.,(4,2,2,
2,2,2,2,2,2,2,4),(0.0581119756758433,0.106553146291161,0.213106292582322,
0.308499338016649,0.386091982889075,0.4636846277615,0.541277272633925,0.61886991750635,
0.714262962940678,0.820816109231839,0.869257279847157),.UNSPECIFIED.);
#697=B_SPLINE_CURVE_WITH_KNOTS('',3,(#33781,#33782,#33783,#33784,#33785,
#33786,#33787,#33788,#33789,#33790,#33791,#33792,#33793,#33794,#33795,#33796,
#33797,#33798,#33799,#33800,#33801,#33802),.UNSPECIFIED.,.F.,.F.,(4,2,2,
2,2,2,2,2,2,2,4),(0.0581119756758433,0.106553146291161,0.213106292582322,
0.30849933801665,0.386091982889075,0.4636846277615,0.541277272633925,0.61886991750635,
0.714262962940678,0.820816109231839,0.869257279847157),.UNSPECIFIED.);
#698=B_SPLINE_CURVE_WITH_KNOTS('',3,(#33806,#33807,#33808,#33809,#33810,
#33811,#33812,#33813,#33814,#33815,#33816,#33817,#33818,#33819,#33820,#33821,
#33822,#33823,#33824,#33825,#33826,#33827),.UNSPECIFIED.,.F.,.F.,(4,2,2,
2,2,2,2,2,2,2,4),(0.0581119756758434,0.106553146291161,0.213106292582322,
0.30849933801665,0.386091982889075,0.4636846277615,0.541277272633925,0.61886991750635,
0.714262962940678,0.820816109231839,0.869257279847157),.UNSPECIFIED.);
#699=B_SPLINE_CURVE_WITH_KNOTS('',3,(#33831,#33832,#33833,#33834,#33835,
#33836,#33837,#33838,#33839,#33840,#33841,#33842,#33843,#33844,#33845,#33846,
#33847,#33848,#33849,#33850,#33851,#33852),.UNSPECIFIED.,.F.,.F.,(4,2,2,
2,2,2,2,2,2,2,4),(0.0581119756758434,0.106553146291161,0.213106292582322,
0.30849933801665,0.386091982889075,0.4636846277615,0.541277272633925,0.61886991750635,
0.714262962940678,0.820816109231839,0.869257279847157),.UNSPECIFIED.);
#700=B_SPLINE_CURVE_WITH_KNOTS('',3,(#33856,#33857,#33858,#33859,#33860,
#33861,#33862,#33863,#33864,#33865,#33866,#33867,#33868,#33869,#33870,#33871,
#33872,#33873,#33874,#33875,#33876,#33877),.UNSPECIFIED.,.F.,.F.,(4,2,2,
2,2,2,2,2,2,2,4),(0.0581119756758433,0.106553146291161,0.213106292582322,
0.30849933801665,0.386091982889075,0.4636846277615,0.541277272633925,0.61886991750635,
0.714262962940678,0.820816109231839,0.869257279847157),.UNSPECIFIED.);
#701=B_SPLINE_CURVE_WITH_KNOTS('',3,(#33885,#33886,#33887,#33888,#33889,
#33890,#33891,#33892,#33893,#33894,#33895,#33896,#33897,#33898,#33899,#33900,
#33901,#33902,#33903,#33904,#33905,#33906),.UNSPECIFIED.,.F.,.F.,(4,2,2,
2,2,2,2,2,2,2,4),(0.0591825211272536,0.157966726598481,0.236950089897721,
0.315933453196962,0.391576304923761,0.467219156650561,0.54286200837736,
0.618504860104159,0.697488223403399,0.77647158670264,0.875255792173867),
 .UNSPECIFIED.);
#702=B_SPLINE_CURVE_WITH_KNOTS('',3,(#33914,#33915,#33916,#33917,#33918,
#33919,#33920,#33921,#33922,#33923,#33924,#33925,#33926,#33927,#33928,#33929,
#33930,#33931,#33932,#33933,#33934,#33935),.UNSPECIFIED.,.F.,.F.,(4,2,2,
2,2,2,2,2,2,2,4),(0.0591825211272536,0.157966726598481,0.236950089897722,
0.315933453196962,0.391576304923761,0.467219156650561,0.54286200837736,
0.618504860104159,0.697488223403399,0.77647158670264,0.875255792173867),
 .UNSPECIFIED.);
#703=B_SPLINE_CURVE_WITH_KNOTS('',3,(#33945,#33946,#33947,#33948,#33949,
#33950,#33951,#33952,#33953,#33954,#33955,#33956,#33957,#33958,#33959,#33960,
#33961,#33962,#33963,#33964,#33965,#33966),.UNSPECIFIED.,.F.,.F.,(4,2,2,
2,2,2,2,2,2,2,4),(0.0591825211272536,0.157966726598481,0.236950089897721,
0.315933453196962,0.391576304923761,0.46721915665056,0.54286200837736,0.618504860104159,
0.697488223403399,0.77647158670264,0.875255792173867),.UNSPECIFIED.);
#704=B_SPLINE_CURVE_WITH_KNOTS('',3,(#33974,#33975,#33976,#33977,#33978,
#33979,#33980,#33981,#33982,#33983,#33984,#33985,#33986,#33987,#33988,#33989,
#33990,#33991,#33992,#33993,#33994,#33995),.UNSPECIFIED.,.F.,.F.,(4,2,2,
2,2,2,2,2,2,2,4),(0.0591825211272536,0.157966726598481,0.236950089897721,
0.315933453196962,0.391576304923761,0.46721915665056,0.542862008377359,
0.618504860104159,0.697488223403399,0.776471586702639,0.875255792173867),
 .UNSPECIFIED.);
#705=B_SPLINE_CURVE_WITH_KNOTS('',3,(#34003,#34004,#34005,#34006,#34007,
#34008,#34009,#34010,#34011,#34012,#34013,#34014,#34015,#34016,#34017,#34018,
#34019,#34020,#34021,#34022,#34023,#34024),.UNSPECIFIED.,.F.,.F.,(4,2,2,
2,2,2,2,2,2,2,4),(0.0591825211272536,0.157966726598481,0.236950089897721,
0.315933453196962,0.391576304923761,0.46721915665056,0.54286200837736,0.618504860104159,
0.697488223403399,0.77647158670264,0.875255792173867),.UNSPECIFIED.);
#706=B_SPLINE_CURVE_WITH_KNOTS('',3,(#34033,#34034,#34035,#34036,#34037,
#34038,#34039,#34040,#34041,#34042,#34043,#34044,#34045,#34046,#34047,#34048,
#34049,#34050,#34051,#34052,#34053,#34054),.UNSPECIFIED.,.F.,.F.,(4,2,2,
2,2,2,2,2,2,2,4),(0.0591825211272536,0.157966726598481,0.236950089897721,
0.315933453196962,0.391576304923761,0.46721915665056,0.542862008377359,
0.618504860104159,0.697488223403399,0.776471586702639,0.875255792173867),
 .UNSPECIFIED.);
#707=B_SPLINE_CURVE_WITH_KNOTS('',3,(#34204,#34205,#34206,#34207,#34208,
#34209,#34210,#34211,#34212,#34213,#34214,#34215,#34216,#34217,#34218,#34219,
#34220,#34221,#34222,#34223,#34224,#34225),.UNSPECIFIED.,.F.,.F.,(4,2,2,
2,2,2,2,2,2,2,4),(0.0789094028588958,0.210573405340968,0.315860108011452,
0.421146810681936,0.522142632548711,0.623138454415485,0.72413427628226,
0.825130098149035,0.930416800819519,1.03570350349,1.16736750597208),
 .UNSPECIFIED.);
#708=B_SPLINE_CURVE_WITH_KNOTS('',3,(#34229,#34230,#34231,#34232,#34233,
#34234,#34235,#34236,#34237,#34238,#34239,#34240,#34241,#34242,#34243,#34244,
#34245,#34246,#34247,#34248,#34249,#34250),.UNSPECIFIED.,.F.,.F.,(4,2,2,
2,2,2,2,2,2,2,4),(0.0774793363974613,0.142088896491891,0.284177792983782,
0.411119756996526,0.514392970548519,0.617666184100513,0.720939397652506,
0.8242126112045,0.951154575217244,1.09324347170913,1.15785303180356),
 .UNSPECIFIED.);
#709=B_SPLINE_CURVE_WITH_KNOTS('',3,(#34256,#34257,#34258,#34259,#34260,
#34261,#34262,#34263,#34264,#34265,#34266,#34267,#34268,#34269,#34270,#34271,
#34272,#34273,#34274,#34275,#34276,#34277),.UNSPECIFIED.,.F.,.F.,(4,2,2,
2,2,2,2,2,2,2,4),(0.0774793363974613,0.142088896491891,0.284177792983782,
0.411119756996525,0.514392970548519,0.617666184100513,0.720939397652506,
0.8242126112045,0.951154575217243,1.09324347170913,1.15785303180356),
 .UNSPECIFIED.);
#710=B_SPLINE_CURVE_WITH_KNOTS('',3,(#34281,#34282,#34283,#34284,#34285,
#34286,#34287,#34288,#34289,#34290,#34291,#34292,#34293,#34294,#34295,#34296,
#34297,#34298,#34299,#34300,#34301,#34302),.UNSPECIFIED.,.F.,.F.,(4,2,2,
2,2,2,2,2,2,2,4),(0.0774793363974614,0.142088896491891,0.284177792983781,
0.411119756996525,0.514392970548519,0.617666184100512,0.720939397652506,
0.824212611204499,0.951154575217243,1.09324347170913,1.15785303180356),
 .UNSPECIFIED.);
#711=B_SPLINE_CURVE_WITH_KNOTS('',3,(#34306,#34307,#34308,#34309,#34310,
#34311,#34312,#34313,#34314,#34315,#34316,#34317),.UNSPECIFIED.,.F.,.F.,
(4,2,2,2,2,4),(0.0774793363974613,0.142088896491891,0.284177792983781,0.411119756996525,
0.514392970548519,0.617666184100512),.UNSPECIFIED.);
#712=B_SPLINE_CURVE_WITH_KNOTS('',3,(#34322,#34323,#34324,#34325,#34326,
#34327,#34328,#34329,#34330,#34331,#34332,#34333),.UNSPECIFIED.,.F.,.F.,
(4,2,2,2,2,4),(0.617666184100512,0.720939397652506,0.824212611204499,0.951154575217243,
1.09324347170913,1.15785303180356),.UNSPECIFIED.);
#713=B_SPLINE_CURVE_WITH_KNOTS('',3,(#34337,#34338,#34339,#34340,#34341,
#34342,#34343,#34344,#34345,#34346,#34347,#34348,#34349,#34350,#34351,#34352,
#34353,#34354,#34355,#34356,#34357,#34358),.UNSPECIFIED.,.F.,.F.,(4,2,2,
2,2,2,2,2,2,2,4),(0.0774793363974613,0.142088896491891,0.284177792983782,
0.411119756996526,0.514392970548519,0.617666184100513,0.720939397652507,
0.8242126112045,0.951154575217245,1.09324347170914,1.15785303180356),
 .UNSPECIFIED.);
#714=B_SPLINE_CURVE_WITH_KNOTS('',3,(#34362,#34363,#34364,#34365,#34366,
#34367,#34368,#34369,#34370,#34371,#34372,#34373,#34374,#34375,#34376,#34377,
#34378,#34379,#34380,#34381,#34382,#34383),.UNSPECIFIED.,.F.,.F.,(4,2,2,
2,2,2,2,2,2,2,4),(0.0774793363974613,0.142088896491891,0.284177792983782,
0.411119756996526,0.514392970548519,0.617666184100513,0.720939397652506,
0.824212611204499,0.951154575217243,1.09324347170913,1.15785303180356),
 .UNSPECIFIED.);
#715=B_SPLINE_CURVE_WITH_KNOTS('',3,(#34387,#34388,#34389,#34390,#34391,
#34392,#34393,#34394,#34395,#34396,#34397,#34398,#34399,#34400,#34401,#34402,
#34403,#34404,#34405,#34406,#34407,#34408),.UNSPECIFIED.,.F.,.F.,(4,2,2,
2,2,2,2,2,2,2,4),(0.0774793363974613,0.142088896491891,0.284177792983782,
0.411119756996526,0.514392970548519,0.617666184100513,0.720939397652506,
0.8242126112045,0.951154575217244,1.09324347170913,1.15785303180356),
 .UNSPECIFIED.);
#716=B_SPLINE_CURVE_WITH_KNOTS('',3,(#34412,#34413,#34414,#34415,#34416,
#34417,#34418,#34419,#34420,#34421,#34422,#34423,#34424,#34425,#34426,#34427,
#34428,#34429,#34430,#34431,#34432,#34433),.UNSPECIFIED.,.F.,.F.,(4,2,2,
2,2,2,2,2,2,2,4),(0.0774793363974613,0.142088896491891,0.284177792983782,
0.411119756996526,0.514392970548519,0.617666184100513,0.720939397652506,
0.8242126112045,0.951154575217243,1.09324347170913,1.15785303180356),
 .UNSPECIFIED.);
#717=B_SPLINE_CURVE_WITH_KNOTS('',3,(#34441,#34442,#34443,#34444,#34445,
#34446,#34447,#34448,#34449,#34450,#34451,#34452,#34453,#34454,#34455,#34456,
#34457,#34458,#34459,#34460,#34461,#34462),.UNSPECIFIED.,.F.,.F.,(4,2,2,
2,2,2,2,2,2,2,4),(0.0789094028588958,0.210573405340968,0.315860108011452,
0.421146810681936,0.522142632548711,0.623138454415485,0.72413427628226,
0.825130098149035,0.930416800819519,1.03570350349,1.16736750597208),
 .UNSPECIFIED.);
#718=B_SPLINE_CURVE_WITH_KNOTS('',3,(#34470,#34471,#34472,#34473,#34474,
#34475,#34476,#34477,#34478,#34479,#34480,#34481,#34482,#34483,#34484,#34485,
#34486,#34487,#34488,#34489,#34490,#34491),.UNSPECIFIED.,.F.,.F.,(4,2,2,
2,2,2,2,2,2,2,4),(0.0789094028588958,0.210573405340969,0.315860108011453,
0.421146810681937,0.522142632548712,0.623138454415486,0.724134276282261,
0.825130098149035,0.930416800819519,1.03570350349,1.16736750597208),
 .UNSPECIFIED.);
#719=B_SPLINE_CURVE_WITH_KNOTS('',3,(#34500,#34501,#34502,#34503,#34504,
#34505,#34506,#34507,#34508,#34509,#34510,#34511),.UNSPECIFIED.,.F.,.F.,
(4,2,2,2,2,4),(0.0789094028588958,0.210573405340968,0.315860108011452,0.421146810681937,
0.522142632548711,0.623138454415486),.UNSPECIFIED.);
#720=B_SPLINE_CURVE_WITH_KNOTS('',3,(#34513,#34514,#34515,#34516,#34517,
#34518,#34519,#34520,#34521,#34522,#34523,#34524),.UNSPECIFIED.,.F.,.F.,
(4,2,2,2,2,4),(0.623138454415486,0.72413427628226,0.825130098149035,0.930416800819519,
1.03570350349,1.16736750597208),.UNSPECIFIED.);
#721=B_SPLINE_CURVE_WITH_KNOTS('',3,(#34531,#34532,#34533,#34534,#34535,
#34536,#34537,#34538,#34539,#34540,#34541,#34542,#34543,#34544,#34545,#34546,
#34547,#34548,#34549,#34550,#34551,#34552),.UNSPECIFIED.,.F.,.F.,(4,2,2,
2,2,2,2,2,2,2,4),(0.0789094028588958,0.210573405340968,0.315860108011452,
0.421146810681936,0.522142632548711,0.623138454415486,0.72413427628226,
0.825130098149035,0.930416800819519,1.03570350349,1.16736750597208),
 .UNSPECIFIED.);
#722=B_SPLINE_CURVE_WITH_KNOTS('',3,(#34560,#34561,#34562,#34563,#34564,
#34565,#34566,#34567,#34568,#34569,#34570,#34571,#34572,#34573,#34574,#34575,
#34576,#34577,#34578,#34579,#34580,#34581),.UNSPECIFIED.,.F.,.F.,(4,2,2,
2,2,2,2,2,2,2,4),(0.0789094028588957,0.210573405340968,0.315860108011452,
0.421146810681936,0.522142632548711,0.623138454415485,0.72413427628226,
0.825130098149035,0.930416800819519,1.03570350349,1.16736750597207),
 .UNSPECIFIED.);
#723=B_SPLINE_CURVE_WITH_KNOTS('',3,(#34589,#34590,#34591,#34592,#34593,
#34594,#34595,#34596,#34597,#34598,#34599,#34600,#34601,#34602,#34603,#34604,
#34605,#34606,#34607,#34608,#34609,#34610),.UNSPECIFIED.,.F.,.F.,(4,2,2,
2,2,2,2,2,2,2,4),(0.0789094028588958,0.210573405340968,0.315860108011452,
0.421146810681936,0.522142632548711,0.623138454415486,0.72413427628226,
0.825130098149035,0.930416800819519,1.03570350349,1.16736750597208),
 .UNSPECIFIED.);
#724=B_SPLINE_CURVE_WITH_KNOTS('',3,(#34619,#34620,#34621,#34622,#34623,
#34624,#34625,#34626,#34627,#34628,#34629,#34630,#34631,#34632,#34633,#34634,
#34635,#34636,#34637,#34638,#34639,#34640),.UNSPECIFIED.,.F.,.F.,(4,2,2,
2,2,2,2,2,2,2,4),(0.0789094028588958,0.210573405340968,0.315860108011452,
0.421146810681936,0.522142632548711,0.623138454415485,0.72413427628226,
0.825130098149035,0.930416800819519,1.03570350349,1.16736750597208),
 .UNSPECIFIED.);
#725=B_SPLINE_CURVE_WITH_KNOTS('',3,(#35262,#35263,#35264,#35265,#35266,
#35267,#35268,#35269,#35270,#35271,#35272,#35273,#35274,#35275,#35276,#35277,
#35278,#35279,#35280,#35281,#35282,#35283,#35284,#35285,#35286),
 .UNSPECIFIED.,.F.,.F.,(4,3,3,3,3,3,3,3,4),(-3.56038179279204,-3.46201024481372,
-2.96743735269747,-2.47286446058123,-1.97829156846498,-1.48371867634874,
-0.989145784232491,-0.494572892116246,0.),.UNSPECIFIED.);
#726=B_SPLINE_CURVE_WITH_KNOTS('',3,(#35289,#35290,#35291,#35292,#35293,
#35294,#35295,#35296,#35297,#35298,#35299,#35300,#35301,#35302,#35303,#35304,
#35305,#35306,#35307,#35308,#35309,#35310,#35311,#35312,#35313,#35314,#35315,
#35316,#35317,#35318,#35319,#35320,#35321,#35322,#35323,#35324,#35325,#35326,
#35327,#35328),.UNSPECIFIED.,.F.,.F.,(4,3,3,3,3,3,3,3,3,3,3,3,3,4),(0.937891254796418,
0.989145784232494,1.48371867634874,1.97829156846498,2.47286446058123,2.96743735269748,
3.46201024481372,3.95658313692997,4.45115602904621,4.94572892116246,5.44030181327871,
5.93487470539495,6.42944759751119,6.80228742277363),.UNSPECIFIED.);
#727=B_SPLINE_CURVE_WITH_KNOTS('',3,(#35333,#35334,#35335,#35336,#35337,
#35338,#35339,#35340,#35341,#35342,#35343,#35344,#35345,#35346,#35347,#35348,
#35349,#35350,#35351,#35352,#35353,#35354,#35355,#35356,#35357,#35358,#35359,
#35360,#35361,#35362,#35363,#35364,#35365,#35366,#35367,#35368,#35369,#35370,
#35371,#35372),.UNSPECIFIED.,.F.,.F.,(4,3,3,3,3,3,3,3,3,3,3,3,3,4),(-9.8435670999716,
-9.39688495020867,-8.90231205809242,-8.40773916597618,-7.91316627385993,
-7.41859338174369,-6.92402048962744,-6.42944759751119,-5.93487470539495,
-5.4403018132787,-4.94572892116246,-4.45115602904621,-3.95658313692996,
-3.56038179279204),.UNSPECIFIED.);
#728=B_SPLINE_CURVE_WITH_KNOTS('',3,(#35373,#35374,#35375,#35376,#35377,
#35378,#35379,#35380,#35381,#35382,#35383,#35384,#35385,#35386,#35387,#35388,
#35389,#35390,#35391,#35392,#35393,#35394,#35395,#35396,#35397,#35398,#35399,
#35400,#35401,#35402,#35403,#35404,#35405,#35406,#35407,#35408,#35409,#35410,
#35411,#35412,#35413,#35414,#35415),.UNSPECIFIED.,.F.,.F.,(4,3,3,3,3,3,
3,3,3,3,3,3,3,3,4),(6.80228742277363,6.92402048962744,7.41859338174369,
7.91316627385993,8.40773916597617,8.90231205809242,9.39688495020867,9.89145784232491,
10.3860307344412,10.8806036265574,11.3751765186736,11.8697494107899,12.3643223029061,
12.8588951950224,13.0854727299532),.UNSPECIFIED.);
#729=B_SPLINE_CURVE_WITH_KNOTS('',3,(#35420,#35421,#35422,#35423,#35424,
#35425,#35426,#35427,#35428,#35429,#35430,#35431,#35432,#35433,#35434,#35435,
#35436,#35437,#35438,#35439,#35440,#35441,#35442,#35443,#35444,#35445,#35446,
#35447,#35448,#35449,#35450,#35451,#35452,#35453,#35454,#35455,#35456,#35457,
#35458,#35459,#35460,#35461,#35462),.UNSPECIFIED.,.F.,.F.,(4,3,3,3,3,3,
3,3,3,3,3,3,3,3,4),(-16.1267524071512,-15.8263325477199,-15.3317596556036,
-14.8371867634874,-14.3426138713711,-13.8480409792549,-13.3534680871386,
-12.8588951950224,-12.3643223029061,-11.8697494107899,-11.3751765186736,
-10.8806036265574,-10.3860307344412,-9.89145784232491,-9.8435670999716),
 .UNSPECIFIED.);
#730=B_SPLINE_CURVE_WITH_KNOTS('',3,(#35463,#35464,#35465,#35466,#35467,
#35468,#35469,#35470,#35471,#35472,#35473,#35474,#35475,#35476,#35477,#35478,
#35479,#35480,#35481,#35482,#35483,#35484,#35485,#35486,#35487,#35488,#35489,
#35490,#35491,#35492,#35493,#35494,#35495,#35496,#35497,#35498,#35499,#35500,
#35501,#35502,#35503,#35504,#35505),.UNSPECIFIED.,.F.,.F.,(4,3,3,3,3,3,
3,3,3,3,3,3,3,3,4),(13.0854727299532,13.3534680871386,13.8480409792549,
14.3426138713711,14.8371867634874,15.3317596556036,15.8263325477199,16.3209054398361,
16.8154783319523,17.3100512240686,17.8046241161848,18.2991970083011,18.7937699004173,
19.2883427925336,19.3686580371328),.UNSPECIFIED.);
#731=B_SPLINE_CURVE_WITH_KNOTS('',3,(#35510,#35511,#35512,#35513,#35514,
#35515,#35516,#35517,#35518,#35519,#35520,#35521,#35522,#35523,#35524,#35525,
#35526,#35527,#35528,#35529,#35530,#35531,#35532,#35533,#35534,#35535,#35536,
#35537,#35538,#35539,#35540,#35541,#35542,#35543,#35544,#35545,#35546,#35547,
#35548,#35549,#35550,#35551,#35552),.UNSPECIFIED.,.F.,.F.,(4,3,3,3,3,3,
3,3,3,3,3,3,3,3,4),(-22.4099377143308,-22.2557801452311,-21.7612072531148,
-21.2666343609986,-20.7720614688823,-20.2774885767661,-19.7829156846498,
-19.2883427925336,-18.7937699004173,-18.2991970083011,-17.8046241161848,
-17.3100512240686,-16.8154783319523,-16.3209054398361,-16.1267524071512),
 .UNSPECIFIED.);
#732=B_SPLINE_CURVE_WITH_KNOTS('',3,(#35553,#35554,#35555,#35556,#35557,
#35558,#35559,#35560,#35561,#35562,#35563,#35564,#35565,#35566,#35567,#35568,
#35569,#35570,#35571,#35572,#35573,#35574,#35575,#35576,#35577,#35578,#35579,
#35580,#35581,#35582,#35583,#35584,#35585,#35586,#35587,#35588,#35589,#35590,
#35591,#35592),.UNSPECIFIED.,.F.,.F.,(4,3,3,3,3,3,3,3,3,3,3,3,3,4),(19.3686580371328,
19.7829156846498,20.2774885767661,20.7720614688823,21.2666343609986,21.7612072531148,
22.255780145231,22.7503530373473,23.2449259294635,23.7394988215798,24.234071713696,
24.7286446058123,25.2232174979285,25.6518433443124),.UNSPECIFIED.);
#733=B_SPLINE_CURVE_WITH_KNOTS('',3,(#35597,#35598,#35599,#35600,#35601,
#35602,#35603,#35604,#35605,#35606,#35607,#35608,#35609,#35610,#35611,#35612,
#35613,#35614,#35615,#35616,#35617,#35618,#35619,#35620,#35621,#35622,#35623,
#35624,#35625,#35626,#35627,#35628,#35629,#35630,#35631,#35632,#35633,#35634,
#35635,#35636,#35637,#35638,#35639),.UNSPECIFIED.,.F.,.F.,(4,3,3,3,3,3,
3,3,3,3,3,3,3,3,4),(-28.6931230215104,-28.6852277427422,-28.190654850626,
-27.6960819585097,-27.2015090663935,-26.7069361742773,-26.212363282161,
-25.7177903900448,-25.2232174979285,-24.7286446058123,-24.234071713696,
-23.7394988215798,-23.2449259294635,-22.7503530373473,-22.4099377143308),
 .UNSPECIFIED.);
#734=B_SPLINE_CURVE_WITH_KNOTS('',3,(#35640,#35641,#35642,#35643,#35644,
#35645,#35646,#35647,#35648,#35649,#35650,#35651,#35652,#35653,#35654,#35655,
#35656,#35657,#35658,#35659,#35660,#35661,#35662,#35663,#35664,#35665,#35666,
#35667,#35668,#35669,#35670,#35671,#35672,#35673,#35674,#35675,#35676,#35677,
#35678,#35679,#35680,#35681,#35682),.UNSPECIFIED.,.F.,.F.,(4,3,3,3,3,3,
3,3,3,3,3,3,3,3,4),(25.6518433443124,25.7177903900448,26.212363282161,26.7069361742773,
27.2015090663935,27.6960819585097,28.190654850626,28.6852277427422,29.1798006348585,
29.6743735269747,30.168946419091,30.6635193112072,31.1580922033235,31.6526650954397,
31.935028651492),.UNSPECIFIED.);
#735=B_SPLINE_CURVE_WITH_KNOTS('',3,(#35687,#35688,#35689,#35690,#35691,
#35692,#35693,#35694,#35695,#35696,#35697,#35698,#35699,#35700,#35701,#35702,
#35703,#35704,#35705,#35706,#35707,#35708,#35709,#35710,#35711,#35712,#35713,
#35714,#35715,#35716,#35717,#35718,#35719,#35720,#35721,#35722,#35723,#35724,
#35725,#35726),.UNSPECIFIED.,.F.,.F.,(4,3,3,3,3,3,3,3,3,3,3,3,3,4),(-34.97630832869,
-34.6201024481372,-34.1255295560209,-33.6309566639047,-33.1363837717884,
-32.6418108796722,-32.147237987556,-31.6526650954397,-31.1580922033235,
-30.6635193112072,-30.168946419091,-29.6743735269747,-29.1798006348585,
-28.6931230215104),.UNSPECIFIED.);
#736=B_SPLINE_CURVE_WITH_KNOTS('',3,(#35727,#35728,#35729,#35730,#35731,
#35732,#35733,#35734,#35735,#35736,#35737,#35738,#35739,#35740,#35741,#35742,
#35743,#35744,#35745,#35746,#35747,#35748,#35749,#35750,#35751,#35752,#35753,
#35754,#35755,#35756,#35757,#35758,#35759,#35760,#35761,#35762,#35763,#35764,
#35765,#35766,#35767,#35768,#35769),.UNSPECIFIED.,.F.,.F.,(4,3,3,3,3,3,
3,3,3,3,3,3,3,3,4),(31.935028651492,32.147237987556,32.6418108796722,33.1363837717885,
33.6309566639047,34.1255295560209,34.6201024481372,35.1146753402534,35.6092482323697,
36.1038211244859,36.5983940166022,37.0929669087184,37.5875398008347,38.0821126929509,
38.2182139586716),.UNSPECIFIED.);
#737=B_SPLINE_CURVE_WITH_KNOTS('',3,(#35774,#35775,#35776,#35777,#35778,
#35779,#35780,#35781,#35782,#35783,#35784,#35785,#35786,#35787,#35788,#35789,
#35790,#35791,#35792,#35793,#35794,#35795,#35796,#35797,#35798,#35799,#35800,
#35801,#35802,#35803,#35804,#35805,#35806,#35807,#35808,#35809,#35810,#35811,
#35812,#35813,#35814,#35815,#35816),.UNSPECIFIED.,.F.,.F.,(4,3,3,3,3,3,
3,3,3,3,3,3,3,3,4),(-41.2594936358696,-41.0495500456484,-40.5549771535321,
-40.0604042614159,-39.5658313692996,-39.0712584771834,-38.5766855850671,
-38.0821126929509,-37.5875398008347,-37.0929669087184,-36.5983940166022,
-36.1038211244859,-35.6092482323697,-35.1146753402534,-34.97630832869),
 .UNSPECIFIED.);
#738=B_SPLINE_CURVE_WITH_KNOTS('',3,(#35817,#35818,#35819,#35820,#35821,
#35822,#35823,#35824,#35825,#35826,#35827,#35828,#35829,#35830,#35831,#35832,
#35833,#35834,#35835,#35836,#35837,#35838,#35839,#35840,#35841,#35842,#35843,
#35844,#35845,#35846,#35847,#35848,#35849,#35850,#35851,#35852,#35853,#35854,
#35855,#35856),.UNSPECIFIED.,.F.,.F.,(4,3,3,3,3,3,3,3,3,3,3,3,3,4),(38.2182139586716,
38.5766855850671,39.0712584771834,39.5658313692996,40.0604042614159,40.5549771535321,
41.0495500456484,41.5441229377646,42.0386958298809,42.5332687219971,43.0278416141134,
43.5224145062296,44.0169873983459,44.5013992658512),.UNSPECIFIED.);
#739=B_SPLINE_CURVE_WITH_KNOTS('',3,(#35861,#35862,#35863,#35864,#35865,
#35866,#35867,#35868,#35869,#35870,#35871,#35872,#35873,#35874,#35875,#35876,
#35877,#35878,#35879,#35880,#35881,#35882,#35883,#35884,#35885,#35886,#35887,
#35888,#35889,#35890,#35891,#35892,#35893,#35894,#35895,#35896,#35897,#35898,
#35899,#35900,#35901,#35902,#35903),.UNSPECIFIED.,.F.,.F.,(4,3,3,3,3,3,
3,3,3,3,3,3,3,3,4),(-47.5426789430491,-47.4789976431596,-46.9844247510433,
-46.4898518589271,-45.9952789668108,-45.5007060746946,-45.0061331825783,
-44.5115602904621,-44.0169873983458,-43.5224145062296,-43.0278416141134,
-42.5332687219971,-42.0386958298809,-41.5441229377646,-41.2594936358696),
 .UNSPECIFIED.);
#740=B_SPLINE_CURVE_WITH_KNOTS('',3,(#35904,#35905,#35906,#35907,#35908,
#35909,#35910,#35911,#35912,#35913,#35914,#35915,#35916,#35917,#35918,#35919,
#35920,#35921,#35922,#35923,#35924,#35925,#35926,#35927,#35928,#35929,#35930,
#35931,#35932,#35933,#35934,#35935,#35936,#35937,#35938,#35939,#35940,#35941,
#35942,#35943,#35944,#35945,#35946),.UNSPECIFIED.,.F.,.F.,(4,3,3,3,3,3,
3,3,3,3,3,3,3,3,4),(44.5013992658512,44.5115602904621,45.0061331825783,
45.5007060746946,45.9952789668108,46.4898518589271,46.9844247510433,47.4789976431596,
47.9735705352758,48.4681434273921,48.9627163195083,49.4572892116245,49.9518621037408,
50.446434995857,50.7845845730308),.UNSPECIFIED.);
#741=B_SPLINE_CURVE_WITH_KNOTS('',3,(#35953,#35954,#35955,#35956,#35957,
#35958,#35959,#35960,#35961,#35962),.UNSPECIFIED.,.F.,.F.,(4,3,3,4),(-54.4542726622231,
-54.403018132787,-53.9084452406708,-53.8258642502287),.UNSPECIFIED.);
#742=B_SPLINE_CURVE_WITH_KNOTS('',3,(#35968,#35969,#35970,#35971,#35972,
#35973,#35974),.UNSPECIFIED.,.F.,.F.,(4,1,1,1,4),(65.9734457253856,66.0560267158277,
66.5505996079439,67.0451725000601,67.5397453921764),.UNSPECIFIED.);
#743=B_SPLINE_CURVE_WITH_KNOTS('',3,(#35977,#35978,#35979,#35980,#35981,
#35982,#35983,#35984,#35985,#35986,#35987,#35988),.UNSPECIFIED.,.F.,.F.,
(4,1,1,1,1,1,1,1,1,4),(65.9734457253856,66.1298690403281,66.6244419324444,
67.1190148245607,67.6135877166769,68.1081606087931,68.6027335009094,69.0973063930256,
69.5918792851419,69.643133814578),.UNSPECIFIED.);
#744=B_SPLINE_CURVE_WITH_KNOTS('',3,(#35993,#35994,#35995,#35996,#35997,
#35998,#35999,#36000,#36001,#36002,#36003,#36004,#36005,#36006,#36007,#36008),
 .UNSPECIFIED.,.F.,.F.,(4,1,1,1,1,1,1,1,1,1,1,1,1,4),(59.6902604182061,
60.1211520104327,60.615724902549,61.1102977946652,61.6048706867815,62.0994435788977,
62.5940164710139,63.0885893631302,63.5831622552464,64.0777351473627,64.5723080394789,
65.0668809315952,65.5614538237114,65.9734457253856),.UNSPECIFIED.);
#745=B_SPLINE_CURVE_WITH_KNOTS('',3,(#36009,#36010,#36011,#36012,#36013,
#36014,#36015,#36016,#36017,#36018,#36019,#36020,#36021,#36022,#36023,#36024,
#36025),.UNSPECIFIED.,.F.,.F.,(4,1,1,1,1,1,1,1,1,1,1,1,1,1,4),(59.6902604182061,
59.700421442817,60.1949943349332,60.6895672270495,61.1841401191657,61.6787130112819,
62.1732859033982,62.6678587955144,63.1624316876307,63.6570045797469,64.1515774718632,
64.6461503639794,65.1407232560957,65.6352961482119,65.9734457253856),
 .UNSPECIFIED.);
#746=B_SPLINE_CURVE_WITH_KNOTS('',3,(#36030,#36031,#36032,#36033,#36034,
#36035,#36036,#36037,#36038,#36039,#36040,#36041,#36042,#36043,#36044,#36045,
#36046),.UNSPECIFIED.,.F.,.F.,(4,1,1,1,1,1,1,1,1,1,1,1,1,1,4),(53.4070751110264,
53.6917044129215,54.1862773050378,54.680850197154,55.1754230892703,55.6699959813865,
56.1645688735028,56.659141765619,57.1537146577353,57.6482875498515,58.1428604419677,
58.637433334084,59.1320062262002,59.6265791183165,59.6902604182061),
 .UNSPECIFIED.);
#747=B_SPLINE_CURVE_WITH_KNOTS('',3,(#36047,#36048,#36049,#36050,#36051,
#36052,#36053,#36054,#36055,#36056,#36057,#36058,#36059,#36060,#36061,#36062),
 .UNSPECIFIED.,.F.,.F.,(4,1,1,1,1,1,1,1,1,1,1,1,1,4),(53.4070751110264,
53.765546737422,54.2601196295383,54.7546925216545,55.2492654137708,55.743838305887,
56.2384111980032,56.7329840901195,57.2275569822357,57.722129874352,58.2167027664682,
58.7112756585845,59.2058485507007,59.6902604182061),.UNSPECIFIED.);
#748=B_SPLINE_CURVE_WITH_KNOTS('',3,(#36067,#36068,#36069,#36070,#36071,
#36072,#36073,#36074,#36075,#36076,#36077,#36078,#36079,#36080,#36081,#36082,
#36083),.UNSPECIFIED.,.F.,.F.,(4,1,1,1,1,1,1,1,1,1,1,1,1,1,4),(47.1238898038469,
47.2622568154103,47.7568297075266,48.2514025996428,48.7459754917591,49.2405483838753,
49.7351212759916,50.2296941681078,50.7242670602241,51.2188399523403,51.7134128444565,
52.2079857365728,52.702558628689,53.1971315208053,53.4070751110264),
 .UNSPECIFIED.);
#749=B_SPLINE_CURVE_WITH_KNOTS('',3,(#36084,#36085,#36086,#36087,#36088,
#36089,#36090,#36091,#36092,#36093,#36094,#36095,#36096,#36097,#36098,#36099,
#36100),.UNSPECIFIED.,.F.,.F.,(4,1,1,1,1,1,1,1,1,1,1,1,1,1,4),(47.1238898038469,
47.3360991399108,47.8306720320271,48.3252449241433,48.8198178162596,49.3143907083758,
49.8089636004921,50.3035364926083,50.7981093847245,51.2926822768408,51.787255168957,
52.2818280610733,52.7764009531895,53.2709738453058,53.4070751110264),
 .UNSPECIFIED.);
#750=B_SPLINE_CURVE_WITH_KNOTS('',3,(#36105,#36106,#36107,#36108,#36109,
#36110,#36111,#36112,#36113,#36114,#36115,#36116,#36117,#36118,#36119,#36120),
 .UNSPECIFIED.,.F.,.F.,(4,1,1,1,1,1,1,1,1,1,1,1,1,4),(40.8407044966673,
41.3273821100154,41.8219550021316,42.3165278942479,42.8111007863641,43.3056736784804,
43.8002465705966,44.2948194627129,44.7893923548291,45.2839652469454,45.7785381390616,
46.2731110311778,46.7676839232941,47.1238898038469),.UNSPECIFIED.);
#751=B_SPLINE_CURVE_WITH_KNOTS('',3,(#36121,#36122,#36123,#36124,#36125,
#36126,#36127,#36128,#36129,#36130,#36131,#36132,#36133,#36134,#36135,#36136,
#36137),.UNSPECIFIED.,.F.,.F.,(4,1,1,1,1,1,1,1,1,1,1,1,1,1,4),(40.8407044966673,
40.9066515423996,41.4012244345159,41.8957973266321,42.3903702187484,42.8849431108646,
43.3795160029809,43.8740888950971,44.3686617872134,44.8632346793296,45.3578075714458,
45.8523804635621,46.3469533556783,46.8415262477946,47.1238898038469),
 .UNSPECIFIED.);
#752=B_SPLINE_CURVE_WITH_KNOTS('',3,(#36142,#36143,#36144,#36145,#36146,
#36147,#36148,#36149,#36150,#36151,#36152,#36153,#36154,#36155,#36156,#36157,
#36158),.UNSPECIFIED.,.F.,.F.,(4,1,1,1,1,1,1,1,1,1,1,1,1,1,4),(34.5575191894877,
34.8979345125042,35.3925074046204,35.8870802967367,36.3816531888529,36.8762260809692,
37.3707989730854,37.8653718652017,38.3599447573179,38.8545176494342,39.3490905415504,
39.8436634336667,40.3382363257829,40.8328092178991,40.8407044966673),
 .UNSPECIFIED.);
#753=B_SPLINE_CURVE_WITH_KNOTS('',3,(#36159,#36160,#36161,#36162,#36163,
#36164,#36165,#36166,#36167,#36168,#36169,#36170,#36171,#36172,#36173,#36174),
 .UNSPECIFIED.,.F.,.F.,(4,1,1,1,1,1,1,1,1,1,1,1,1,4),(34.5575191894877,
34.9717768370047,35.4663497291209,35.9609226212372,36.4554955133534,36.9500684054697,
37.4446412975859,37.9392141897022,38.4337870818184,38.9283599739347,39.4229328660509,
39.9175057581671,40.4120786502834,40.8407044966673),.UNSPECIFIED.);
#754=B_SPLINE_CURVE_WITH_KNOTS('',3,(#36179,#36180,#36181,#36182,#36183,
#36184,#36185,#36186,#36187,#36188,#36189,#36190,#36191,#36192,#36193,#36194,
#36195),.UNSPECIFIED.,.F.,.F.,(4,1,1,1,1,1,1,1,1,1,1,1,1,1,4),(28.2743338823081,
28.468486914993,28.9630598071093,29.4576326992255,29.9522055913417,30.446778483458,
30.9413513755742,31.4359242676905,31.9304971598067,32.425070051923,32.9196429440392,
33.4142158361555,33.9087887282717,34.403361620388,34.5575191894877),
 .UNSPECIFIED.);
#755=B_SPLINE_CURVE_WITH_KNOTS('',3,(#36196,#36197,#36198,#36199,#36200,
#36201,#36202,#36203,#36204,#36205,#36206,#36207,#36208,#36209,#36210,#36211,
#36212),.UNSPECIFIED.,.F.,.F.,(4,1,1,1,1,1,1,1,1,1,1,1,1,1,4),(28.2743338823081,
28.5423292394935,29.0369021316097,29.531475023726,30.0260479158422,30.5206208079585,
31.0151937000747,31.509766592191,32.0043394843072,32.4989123764235,32.9934852685397,
33.488058160656,33.9826310527722,34.4772039448884,34.5575191894877),
 .UNSPECIFIED.);
#756=B_SPLINE_CURVE_WITH_KNOTS('',3,(#36217,#36218,#36219,#36220,#36221,
#36222,#36223,#36224,#36225,#36226,#36227,#36228,#36229,#36230,#36231,#36232,
#36233),.UNSPECIFIED.,.F.,.F.,(4,1,1,1,1,1,1,1,1,1,1,1,1,1,4),(21.9911485751285,
22.0390393174818,22.5336122095981,23.0281851017143,23.5227579938306,24.0173308859468,
24.511903778063,25.0064766701793,25.5010495622955,25.9956224544118,26.490195346528,
26.9847682386443,27.4793411307605,27.9739140228768,28.2743338823081),
 .UNSPECIFIED.);
#757=B_SPLINE_CURVE_WITH_KNOTS('',3,(#36234,#36235,#36236,#36237,#36238,
#36239,#36240,#36241,#36242,#36243,#36244,#36245,#36246,#36247,#36248,#36249,
#36250),.UNSPECIFIED.,.F.,.F.,(4,1,1,1,1,1,1,1,1,1,1,1,1,1,4),(21.9911485751285,
22.1128816419823,22.6074545340986,23.1020274262148,23.596600318331,24.0911732104473,
24.5857461025635,25.0803189946798,25.574891886796,26.0694647789123,26.5640376710285,
27.0586105631448,27.553183455261,28.0477563473773,28.2743338823081),
 .UNSPECIFIED.);
#758=B_SPLINE_CURVE_WITH_KNOTS('',3,(#36256,#36257,#36258,#36259,#36260),
 .UNSPECIFIED.,.F.,.F.,(4,1,4),(15.1888611523549,15.6834340444711,15.7079632679489),
 .UNSPECIFIED.);
#759=B_SPLINE_CURVE_WITH_KNOTS('',3,(#36263,#36264,#36265,#36266,#36267,
#36268,#36269,#36270,#36271,#36272),.UNSPECIFIED.,.F.,.F.,(4,1,1,1,1,1,
1,4),(13.0854727299533,13.1367272593894,13.6313001515056,14.1258730436219,
14.6204459357381,15.1150188278544,15.6095917199706,15.7079632679489),
 .UNSPECIFIED.);
#760=B_SPLINE_CURVE_WITH_KNOTS('',3,(#36274,#36275,#36276,#36277,#36278,
#36279,#36280,#36281,#36282,#36283,#36284,#36285,#36286,#36287,#36288,#36289),
 .UNSPECIFIED.,.F.,.F.,(4,1,1,1,1,1,1,1,1,1,1,1,1,4),(15.7079632679489,
16.1041646120869,16.5987375042031,17.0933103963194,17.5878832884356,18.0824561805519,
18.5770290726681,19.0716019647843,19.5661748569006,20.0607477490168,20.5553206411331,
21.0498935332493,21.5444664253656,21.9911485751285),.UNSPECIFIED.);
#761=B_SPLINE_CURVE_WITH_KNOTS('',3,(#36290,#36291,#36292,#36293,#36294,
#36295,#36296,#36297,#36298,#36299,#36300,#36301,#36302,#36303,#36304,#36305),
 .UNSPECIFIED.,.F.,.F.,(4,1,1,1,1,1,1,1,1,1,1,1,1,4),(15.7079632679489,
16.1780069365874,16.6725798287036,17.1671527208199,17.6617256129361,18.1562985050523,
18.6508713971686,19.1454442892848,19.6400171814011,20.1345900735173,20.6291629656336,
21.1237358577498,21.6183087498661,21.9911485751285),.UNSPECIFIED.);
#762=B_SPLINE_CURVE_WITH_KNOTS('',3,(#36766,#36767,#36768,#36769,#36770,
#36771,#36772,#36773,#36774,#36775,#36776,#36777,#36778,#36779,#36780,#36781,
#36782,#36783,#36784,#36785,#36786,#36787,#36788,#36789,#36790,#36791,#36792,
#36793,#36794,#36795,#36796),.UNSPECIFIED.,.F.,.F.,(4,3,3,3,3,3,3,3,3,3,
4),(0.,0.0822466706468383,0.162608105240606,0.216579893838171,0.23924274204394,
0.301838371937517,0.36076250940623,0.388067588559334,0.409537377502954,
0.476290104322315,0.53753492181237),.UNSPECIFIED.);
#763=B_SPLINE_CURVE_WITH_KNOTS('',3,(#36797,#36798,#36799,#36800,#36801,
#36802,#36803,#36804,#36805,#36806,#36807,#36808,#36809,#36810,#36811,#36812,
#36813,#36814,#36815,#36816,#36817,#36818,#36819,#36820,#36821,#36822,#36823,
#36824),.UNSPECIFIED.,.F.,.F.,(4,3,3,3,3,3,3,3,3,4),(0.,0.0665230127441691,
0.13429495842692,0.176258819244205,0.195926107024299,0.263526952009386,
0.33682854572103,0.365338415901403,0.449700157257057,0.534061898612711),
 .UNSPECIFIED.);
#764=B_SPLINE_CURVE_WITH_KNOTS('',3,(#36825,#36826,#36827,#36828,#36829,
#36830,#36831,#36832,#36833,#36834,#36835,#36836,#36837,#36838,#36839,#36840,
#36841,#36842,#36843,#36844,#36845,#36846,#36847,#36848,#36849,#36850,#36851,
#36852,#36853,#36854,#36855,#36856,#36857,#36858,#36859,#36860,#36861,#36862,
#36863,#36864),.UNSPECIFIED.,.F.,.F.,(4,3,3,3,3,3,3,3,3,3,3,3,3,4),(-53.8258642502287,
-53.4138723485545,-52.9192994564383,-52.424726564322,-51.9301536722058,
-51.4355807800895,-50.9410078879733,-50.446434995857,-49.9518621037408,
-49.4572892116245,-48.9627163195083,-48.4681434273921,-47.9735705352758,
-47.5426789430491),.UNSPECIFIED.);
#765=B_SPLINE_CURVE_WITH_KNOTS('',3,(#37326,#37327,#37328,#37329,#37330,
#37331,#37332,#37333,#37334,#37335,#37336,#37337,#37338,#37339,#37340,#37341,
#37342,#37343,#37344,#37345,#37346,#37347,#37348,#37349,#37350,#37351,#37352,
#37353),.UNSPECIFIED.,.F.,.F.,(4,3,3,3,3,3,3,3,3,4),(0.,0.0665230199567328,
0.134294967830964,0.176258831509978,0.195926124443112,0.263526952009376,
0.336828549458816,0.365338416771381,0.449700157692121,0.534061898612861),
 .UNSPECIFIED.);
#766=B_SPLINE_CURVE_WITH_KNOTS('',3,(#37354,#37355,#37356,#37357,#37358,
#37359,#37360,#37361,#37362,#37363,#37364,#37365,#37366,#37367,#37368,#37369,
#37370,#37371,#37372,#37373,#37374,#37375,#37376,#37377,#37378,#37379,#37380,
#37381,#37382,#37383,#37384),.UNSPECIFIED.,.F.,.F.,(4,3,3,3,3,3,3,3,3,3,
4),(50.7845845730308,50.9410078879733,51.4355807800895,51.9301536722058,
52.424726564322,52.9192994564383,53.4138723485545,53.9084452406708,54.403018132787,
54.8975910249033,55.3921639170195),.UNSPECIFIED.);
#767=B_SPLINE_CURVE_WITH_KNOTS('',3,(#37385,#37386,#37387,#37388,#37389,
#37390,#37391,#37392,#37393,#37394,#37395,#37396,#37397,#37398,#37399,#37400,
#37401,#37402,#37403,#37404,#37405,#37406,#37407,#37408,#37409,#37410,#37411,
#37412,#37413,#37414,#37415),.UNSPECIFIED.,.F.,.F.,(4,3,3,3,3,3,3,3,3,3,
4),(0.,0.0822466663612967,0.162608100396307,0.216579890867136,0.239242742625966,
0.301838371937549,0.360762509406336,0.388067584071394,0.409537375230468,
0.476290092032249,0.537534921812695),.UNSPECIFIED.);
#768=B_SPLINE_CURVE_WITH_KNOTS('',3,(#37624,#37625,#37626,#37627,#37628,
#37629,#37630,#37631,#37632,#37633,#37634,#37635,#37636,#37637,#37638,#37639,
#37640,#37641,#37642),.UNSPECIFIED.,.F.,.F.,(4,3,3,3,3,3,4),(-3.69871549170445,
-3.49775346748116,-2.99807440069814,-2.49839533391511,-1.99871626713209,
-1.49903720034907,-1.00018350866767),.UNSPECIFIED.);
#769=B_SPLINE_CURVE_WITH_KNOTS('',3,(#37645,#37646,#37647,#37648),
 .UNSPECIFIED.,.F.,.F.,(4,4),(0.,0.443060670554495),.UNSPECIFIED.);
#770=B_SPLINE_CURVE_WITH_KNOTS('',3,(#37653,#37654,#37655,#37656,#37657,
#37658,#37659,#37660,#37661,#37662,#37663,#37664,#37665,#37666,#37667,#37668,
#37669,#37670,#37671,#37672,#37673,#37674,#37675,#37676,#37677,#37678,#37679,
#37680,#37681,#37682,#37683,#37684,#37685,#37686,#37687,#37688,#37689,#37690,
#37691,#37692),.UNSPECIFIED.,.F.,.F.,(4,3,3,3,3,3,3,3,3,3,3,3,3,4),(-9.98190079888403,
-9.49390226887744,-8.99422320209442,-8.4945441353114,-7.99486506852837,
-7.49518600174535,-6.99550693496233,-6.4958278681793,-5.99614880139628,
-5.49646973461325,-4.99679066783023,-4.49711160104721,-3.99743253426419,
-3.69871549170445),.UNSPECIFIED.);
#771=B_SPLINE_CURVE_WITH_KNOTS('',3,(#37693,#37694,#37695,#37696,#37697,
#37698,#37699,#37700,#37701,#37702,#37703,#37704,#37705,#37706,#37707,#37708,
#37709,#37710,#37711,#37712,#37713,#37714,#37715,#37716,#37717,#37718,#37719,
#37720,#37721,#37722,#37723,#37724,#37725,#37726,#37727,#37728,#37729,#37730,
#37731,#37732,#37733,#37734,#37735),.UNSPECIFIED.,.F.,.F.,(4,3,3,3,3,3,
3,3,3,3,3,3,3,3,4),(0.443060670554495,0.49967906678306,0.999358133566079,
1.4990372003491,1.99871626713212,2.49839533391514,2.99807440069816,3.49775346748117,
3.99743253426419,4.49711160104721,4.99679066783023,5.49646973461325,5.99614880139627,
6.49582786817929,6.72624597773408),.UNSPECIFIED.);
#772=B_SPLINE_CURVE_WITH_KNOTS('',3,(#37740,#37741,#37742,#37743,#37744,
#37745,#37746,#37747,#37748,#37749,#37750,#37751,#37752,#37753,#37754,#37755,
#37756,#37757,#37758,#37759,#37760,#37761,#37762,#37763,#37764,#37765,#37766,
#37767,#37768,#37769,#37770,#37771,#37772,#37773,#37774,#37775,#37776,#37777,
#37778,#37779,#37780,#37781,#37782),.UNSPECIFIED.,.F.,.F.,(4,3,3,3,3,3,
3,3,3,3,3,3,3,3,4),(-16.2650861060636,-15.9897301370567,-15.4900510702737,
-14.9903720034907,-14.4906929367077,-13.9910138699247,-13.4913348031416,
-12.9916557363586,-12.4919766695756,-11.9922976027926,-11.4926185360095,
-10.9929394692265,-10.4932604024435,-9.99358133566046,-9.98190079888403),
 .UNSPECIFIED.);
#773=B_SPLINE_CURVE_WITH_KNOTS('',3,(#37783,#37784,#37785,#37786,#37787,
#37788,#37789,#37790,#37791,#37792,#37793,#37794,#37795,#37796,#37797,#37798,
#37799,#37800,#37801,#37802,#37803,#37804,#37805,#37806,#37807,#37808,#37809,
#37810,#37811,#37812,#37813,#37814,#37815,#37816,#37817,#37818,#37819,#37820,
#37821,#37822,#37823,#37824,#37825),.UNSPECIFIED.,.F.,.F.,(4,3,3,3,3,3,
3,3,3,3,3,3,3,3,4),(6.72624597773408,6.99550693496231,7.49518600174534,
7.99486506852837,8.49454413531139,8.99422320209442,9.49390226887745,9.99358133566048,
10.4932604024435,10.9929394692265,11.4926185360096,11.9922976027926,12.4919766695756,
12.9916557363586,13.0094312849137),.UNSPECIFIED.);
#774=B_SPLINE_CURVE_WITH_KNOTS('',3,(#37830,#37831,#37832,#37833,#37834,
#37835,#37836,#37837,#37838,#37839,#37840,#37841,#37842,#37843,#37844,#37845,
#37846,#37847,#37848,#37849,#37850,#37851,#37852,#37853,#37854,#37855,#37856,
#37857,#37858,#37859,#37860,#37861,#37862,#37863,#37864,#37865,#37866,#37867,
#37868,#37869,#37870,#37871,#37872),.UNSPECIFIED.,.F.,.F.,(4,3,3,3,3,3,
3,3,3,3,3,3,3,3,4),(-22.5482714132432,-22.485558005236,-21.985878938453,
-21.48619987167,-20.986520804887,-20.486841738104,-19.9871626713209,-19.4874836045379,
-18.9878045377549,-18.4881254709719,-17.9884464041888,-17.4887673374058,
-16.9890882706228,-16.4894092038398,-16.2650861060636),.UNSPECIFIED.);
#775=B_SPLINE_CURVE_WITH_KNOTS('',3,(#37873,#37874,#37875,#37876,#37877,
#37878,#37879,#37880,#37881,#37882,#37883,#37884,#37885,#37886,#37887,#37888,
#37889,#37890,#37891,#37892,#37893,#37894,#37895,#37896,#37897,#37898,#37899,
#37900,#37901,#37902,#37903,#37904,#37905,#37906,#37907,#37908,#37909,#37910,
#37911,#37912),.UNSPECIFIED.,.F.,.F.,(4,3,3,3,3,3,3,3,3,3,3,3,3,4),(13.0094312849137,
13.4913348031417,13.9910138699247,14.4906929367077,14.9903720034907,15.4900510702737,
15.9897301370568,16.4894092038398,16.9890882706228,17.4887673374058,17.9884464041888,
18.4881254709718,18.9878045377549,19.2926165920933),.UNSPECIFIED.);
#776=B_SPLINE_CURVE_WITH_KNOTS('',3,(#37917,#37918,#37919,#37920,#37921,
#37922,#37923,#37924,#37925,#37926,#37927,#37928,#37929,#37930,#37931,#37932,
#37933,#37934,#37935,#37936,#37937,#37938,#37939,#37940,#37941,#37942,#37943,
#37944,#37945,#37946,#37947,#37948,#37949,#37950,#37951,#37952,#37953,#37954,
#37955,#37956),.UNSPECIFIED.,.F.,.F.,(4,3,3,3,3,3,3,3,3,3,3,3,3,4),(-28.8314567204228,
-28.4817068066323,-27.9820277398493,-27.4823486730663,-26.9826696062833,
-26.4829905395002,-25.9833114727172,-25.4836324059342,-24.9839533391512,
-24.4842742723681,-23.9845952055851,-23.4849161388021,-22.9852370720191,
-22.5482714132432),.UNSPECIFIED.);
#777=B_SPLINE_CURVE_WITH_KNOTS('',3,(#37957,#37958,#37959,#37960,#37961,
#37962,#37963,#37964,#37965,#37966,#37967,#37968,#37969,#37970,#37971,#37972,
#37973,#37974,#37975,#37976,#37977,#37978,#37979,#37980,#37981,#37982,#37983,
#37984,#37985,#37986,#37987,#37988,#37989,#37990,#37991,#37992,#37993,#37994,
#37995,#37996,#37997,#37998,#37999),.UNSPECIFIED.,.F.,.F.,(4,3,3,3,3,3,
3,3,3,3,3,3,3,3,4),(19.2926165920933,19.4874836045379,19.9871626713209,
20.4868417381039,20.986520804887,21.48619987167,21.985878938453,22.4855580052361,
22.9852370720191,23.4849161388021,23.9845952055851,24.4842742723682,24.9839533391512,
25.4836324059342,25.5758018992728),.UNSPECIFIED.);
#778=B_SPLINE_CURVE_WITH_KNOTS('',3,(#38004,#38005,#38006,#38007,#38008,
#38009,#38010,#38011,#38012,#38013,#38014,#38015,#38016,#38017,#38018,#38019,
#38020,#38021,#38022,#38023,#38024,#38025,#38026,#38027,#38028,#38029,#38030,
#38031,#38032,#38033,#38034,#38035,#38036,#38037,#38038,#38039,#38040,#38041,
#38042,#38043,#38044,#38045,#38046),.UNSPECIFIED.,.F.,.F.,(4,3,3,3,3,3,
3,3,3,3,3,3,3,3,4),(-35.1146420276024,-34.9775346748116,-34.4778556080286,
-33.9781765412456,-33.4784974744626,-32.9788184076795,-32.4791393408965,
-31.9794602741135,-31.4797812073305,-30.9801021405474,-30.4804230737644,
-29.9807440069814,-29.4810649401984,-28.9813858734153,-28.8314567204228),
 .UNSPECIFIED.);
#779=B_SPLINE_CURVE_WITH_KNOTS('',3,(#38047,#38048,#38049,#38050,#38051,
#38052,#38053,#38054,#38055,#38056,#38057,#38058,#38059,#38060,#38061,#38062,
#38063,#38064,#38065,#38066,#38067,#38068,#38069,#38070,#38071,#38072,#38073,
#38074,#38075,#38076,#38077,#38078,#38079,#38080,#38081,#38082,#38083,#38084,
#38085,#38086),.UNSPECIFIED.,.F.,.F.,(4,3,3,3,3,3,3,3,3,3,3,3,3,4),(25.5758018992728,
25.9833114727172,26.4829905395003,26.9826696062833,27.4823486730663,27.9820277398493,
28.4817068066324,28.9813858734154,29.4810649401984,29.9807440069814,30.4804230737645,
30.9801021405475,31.4797812073305,31.8589872064524),.UNSPECIFIED.);
#780=B_SPLINE_CURVE_WITH_KNOTS('',3,(#38091,#38092,#38093,#38094,#38095,
#38096,#38097,#38098,#38099,#38100,#38101,#38102,#38103,#38104,#38105,#38106,
#38107,#38108,#38109,#38110,#38111,#38112,#38113,#38114,#38115,#38116,#38117,
#38118,#38119,#38120,#38121,#38122,#38123,#38124,#38125,#38126,#38127,#38128,
#38129,#38130),.UNSPECIFIED.,.F.,.F.,(4,3,3,3,3,3,3,3,3,3,3,3,3,4),(-41.397827334782,
-40.9736834762079,-40.4740044094249,-39.9743253426419,-39.4746462758588,
-38.9749672090758,-38.4752881422928,-37.9756090755098,-37.4759300087267,
-36.9762509419437,-36.4765718751607,-35.9768928083777,-35.4772137415947,
-35.1146420276024),.UNSPECIFIED.);
#781=B_SPLINE_CURVE_WITH_KNOTS('',3,(#38131,#38132,#38133,#38134,#38135,
#38136,#38137,#38138,#38139,#38140,#38141,#38142,#38143,#38144,#38145,#38146,
#38147,#38148,#38149,#38150,#38151,#38152,#38153,#38154,#38155,#38156,#38157,
#38158,#38159,#38160,#38161,#38162,#38163,#38164,#38165,#38166,#38167,#38168,
#38169,#38170,#38171,#38172,#38173),.UNSPECIFIED.,.F.,.F.,(4,3,3,3,3,3,
3,3,3,3,3,3,3,3,4),(31.8589872064524,31.9794602741135,32.4791393408966,
32.9788184076796,33.4784974744626,33.9781765412456,34.4778556080286,34.9775346748117,
35.4772137415947,35.9768928083777,36.4765718751607,36.9762509419437,37.4759300087267,
37.9756090755098,38.142172513632),.UNSPECIFIED.);
#782=B_SPLINE_CURVE_WITH_KNOTS('',3,(#38178,#38179,#38180,#38181,#38182,
#38183,#38184,#38185,#38186,#38187,#38188,#38189,#38190,#38191,#38192,#38193,
#38194,#38195,#38196,#38197,#38198,#38199,#38200,#38201,#38202,#38203,#38204,
#38205,#38206,#38207,#38208,#38209,#38210,#38211,#38212,#38213,#38214,#38215,
#38216,#38217,#38218,#38219,#38220),.UNSPECIFIED.,.F.,.F.,(4,3,3,3,3,3,
3,3,3,3,3,3,3,3,4),(-47.6810126419616,-47.4695113443872,-46.9698322776042,
-46.4701532108212,-45.9704741440381,-45.4707950772551,-44.9711160104721,
-44.4714369436891,-43.971757876906,-43.472078810123,-42.97239974334,-42.472720676557,
-41.973041609774,-41.4733625429909,-41.397827334782),.UNSPECIFIED.);
#783=B_SPLINE_CURVE_WITH_KNOTS('',3,(#38221,#38222,#38223,#38224,#38225,
#38226,#38227,#38228,#38229,#38230,#38231,#38232,#38233,#38234,#38235,#38236,
#38237,#38238,#38239,#38240,#38241,#38242,#38243,#38244,#38245,#38246,#38247,
#38248,#38249,#38250,#38251,#38252,#38253,#38254,#38255,#38256,#38257,#38258,
#38259,#38260),.UNSPECIFIED.,.F.,.F.,(4,3,3,3,3,3,3,3,3,3,3,3,3,4),(38.142172513632,
38.4752881422928,38.9749672090758,39.4746462758589,39.9743253426419,40.4740044094249,
40.973683476208,41.473362542991,41.973041609774,42.472720676557,42.9723997433401,
43.4720788101231,43.9717578769061,44.4253578208116),.UNSPECIFIED.);
#784=B_SPLINE_CURVE_WITH_KNOTS('',3,(#38265,#38266,#38267,#38268,#38269,
#38270,#38271,#38272,#38273,#38274,#38275,#38276,#38277,#38278,#38279,#38280,
#38281,#38282,#38283,#38284,#38285,#38286,#38287,#38288,#38289,#38290,#38291,
#38292),.UNSPECIFIED.,.F.,.F.,(4,3,3,3,3,3,3,3,3,4),(-53.9641979491412,
-52.9659810790005,-51.9666229454344,-50.9672648118684,-49.9679066783023,
-49.4682276115193,-48.9685485447363,-48.4688694779533,-47.9691904111702,
-47.6810126419616),.UNSPECIFIED.);
#785=B_SPLINE_CURVE_WITH_KNOTS('',3,(#38293,#38294,#38295,#38296,#38297,
#38298,#38299,#38300,#38301,#38302,#38303,#38304,#38305,#38306,#38307,#38308,
#38309,#38310,#38311,#38312,#38313,#38314,#38315,#38316,#38317,#38318,#38319,
#38320,#38321,#38322,#38323,#38324,#38325,#38326,#38327,#38328,#38329,#38330,
#38331,#38332),.UNSPECIFIED.,.F.,.F.,(4,3,3,3,3,3,3,3,3,3,3,3,3,4),(44.4253578208116,
44.4714369436892,44.9711160104722,45.4707950772552,45.9704741440382,46.4701532108212,
46.9698322776042,47.4695113443873,47.9691904111703,48.4688694779533,48.9685485447363,
49.4682276115193,49.9679066783024,50.7085431279912),.UNSPECIFIED.);
#786=B_SPLINE_CURVE_WITH_KNOTS('',3,(#38337,#38338,#38339,#38340,#38341,
#38342,#38343,#38344,#38345,#38346,#38347,#38348,#38349,#38350,#38351,#38352,
#38353,#38354,#38355,#38356,#38357,#38358),.UNSPECIFIED.,.F.,.F.,(4,3,3,
3,3,3,3,4),(-60.2473832563207,-59.9614880139628,-58.9621298803968,-57.9627717468307,
-56.9634136132647,-55.9640554796986,-54.9646973461326,-53.9641979491412),
 .UNSPECIFIED.);
#787=B_SPLINE_CURVE_WITH_KNOTS('',3,(#38359,#38360,#38361,#38362,#38363,
#38364,#38365,#38366,#38367,#38368,#38369,#38370,#38371,#38372,#38373,#38374,
#38375,#38376,#38377,#38378,#38379,#38380,#38381,#38382,#38383),
 .UNSPECIFIED.,.F.,.F.,(4,3,3,3,3,3,3,3,4),(50.7085431279912,50.9672648118684,
51.9666229454345,52.9659810790005,53.9653392125666,54.9646973461326,55.9640554796987,
56.9634136132647,56.9917284351708),.UNSPECIFIED.);
#788=B_SPLINE_CURVE_WITH_KNOTS('',3,(#38388,#38389,#38390,#38391,#38392,
#38393,#38394,#38395,#38396,#38397,#38398,#38399,#38400,#38401,#38402,#38403,
#38404,#38405,#38406,#38407,#38408,#38409),.UNSPECIFIED.,.F.,.F.,(4,3,3,
3,3,3,3,4),(-66.5305685635003,-65.9576368153591,-64.958278681793,-63.958920548227,
-62.9595624146609,-61.9602042810949,-60.9608461475288,-60.2473832563207),
 .UNSPECIFIED.);
#789=B_SPLINE_CURVE_WITH_KNOTS('',3,(#38410,#38411,#38412,#38413,#38414,
#38415,#38416,#38417,#38418,#38419,#38420,#38421,#38422,#38423,#38424,#38425,
#38426,#38427,#38428,#38429,#38430,#38431),.UNSPECIFIED.,.F.,.F.,(4,3,3,
3,3,3,3,4),(56.9917284351708,57.9627717468308,58.9621298803968,59.9614880139629,
60.9608461475289,61.960204281095,62.959562414661,63.2749137423504),
 .UNSPECIFIED.);
#790=B_SPLINE_CURVE_WITH_KNOTS('',3,(#38436,#38437,#38438,#38439,#38440,
#38441,#38442,#38443,#38444,#38445,#38446,#38447,#38448,#38449,#38450,#38451,
#38452,#38453,#38454,#38455,#38456,#38457),.UNSPECIFIED.,.F.,.F.,(4,3,3,
3,3,3,3,4),(-72.8137538706799,-71.9537856167554,-70.9544274831893,-69.9550693496233,
-68.9557112160572,-67.9563530824912,-66.9569949489251,-66.5305685635003),
 .UNSPECIFIED.);
#791=B_SPLINE_CURVE_WITH_KNOTS('',3,(#38458,#38459,#38460,#38461,#38462,
#38463,#38464,#38465,#38466,#38467,#38468,#38469,#38470,#38471,#38472,#38473,
#38474,#38475,#38476,#38477,#38478,#38479),.UNSPECIFIED.,.F.,.F.,(4,3,3,
3,3,3,3,4),(63.2749137423504,63.958920548227,64.9582786817931,65.9576368153591,
66.9569949489252,67.9563530824912,68.9557112160573,69.55809904953),
 .UNSPECIFIED.);
#792=B_SPLINE_CURVE_WITH_KNOTS('',3,(#38484,#38485,#38486,#38487,#38488,
#38489,#38490,#38491,#38492,#38493,#38494,#38495,#38496,#38497,#38498,#38499,
#38500,#38501,#38502,#38503,#38504,#38505,#38506,#38507,#38508),
 .UNSPECIFIED.,.F.,.F.,(4,3,3,3,3,3,3,3,4),(-79.0969391778595,-78.9492925517177,
-77.9499344181516,-76.9505762845856,-75.9512181510195,-74.9518600174535,
-73.9525018838875,-72.9531437503214,-72.8137538706799),.UNSPECIFIED.);
#793=B_SPLINE_CURVE_WITH_KNOTS('',3,(#38509,#38510,#38511,#38512,#38513,
#38514,#38515,#38516,#38517,#38518,#38519,#38520,#38521,#38522,#38523,#38524,
#38525,#38526,#38527,#38528,#38529,#38530),.UNSPECIFIED.,.F.,.F.,(4,3,3,
3,3,3,3,4),(69.55809904953,69.9550693496233,70.9544274831893,71.9537856167554,
72.9531437503215,73.9525018838875,74.9518600174536,75.8412843567096),
 .UNSPECIFIED.);
#794=B_SPLINE_CURVE_WITH_KNOTS('',3,(#38535,#38536,#38537,#38538,#38539,
#38540,#38541,#38542,#38543,#38544,#38545,#38546,#38547,#38548,#38549,#38550,
#38551,#38552,#38553,#38554,#38555,#38556),.UNSPECIFIED.,.F.,.F.,(4,3,3,
3,3,3,3,4),(-85.3801244850391,-84.945441353114,-83.9460832195479,-82.9467250859819,
-81.9473669524158,-80.9480088188498,-79.9486506852837,-79.0969391778595),
 .UNSPECIFIED.);
#795=B_SPLINE_CURVE_WITH_KNOTS('',3,(#38557,#38558,#38559,#38560,#38561,
#38562,#38563,#38564,#38565,#38566,#38567,#38568,#38569,#38570,#38571,#38572,
#38573,#38574,#38575,#38576,#38577,#38578,#38579,#38580,#38581),
 .UNSPECIFIED.,.F.,.F.,(4,3,3,3,3,3,3,3,4),(75.8412843567096,75.9512181510196,
76.9505762845857,77.9499344181517,78.9492925517178,79.9486506852838,80.9480088188499,
81.9473669524159,82.1244696638892),.UNSPECIFIED.);
#796=B_SPLINE_CURVE_WITH_KNOTS('',3,(#38586,#38587,#38588,#38589,#38590,
#38591,#38592,#38593,#38594,#38595,#38596,#38597,#38598,#38599,#38600,#38601,
#38602,#38603,#38604,#38605,#38606,#38607),.UNSPECIFIED.,.F.,.F.,(4,3,3,
3,3,3,3,4),(-91.6633097922187,-90.9415901545102,-89.9422320209442,-88.9428738873782,
-87.9435157538121,-86.944157620246,-85.94479948668,-85.3801244850391),
 .UNSPECIFIED.);
#797=B_SPLINE_CURVE_WITH_KNOTS('',3,(#38608,#38609,#38610,#38611,#38612,
#38613,#38614,#38615,#38616,#38617,#38618,#38619,#38620,#38621,#38622,#38623,
#38624,#38625,#38626,#38627,#38628,#38629),.UNSPECIFIED.,.F.,.F.,(4,3,3,
3,3,3,3,4),(82.1244696638892,82.946725085982,83.946083219548,84.9454413531141,
85.9447994866801,86.9441576202461,87.9435157538122,88.4076549710687),
 .UNSPECIFIED.);
#798=B_SPLINE_CURVE_WITH_KNOTS('',3,(#38634,#38635,#38636,#38637,#38638,
#38639,#38640,#38641,#38642,#38643,#38644,#38645,#38646,#38647,#38648,#38649,
#38650,#38651,#38652,#38653,#38654,#38655,#38656,#38657,#38658),
 .UNSPECIFIED.,.F.,.F.,(4,3,3,3,3,3,3,3,4),(-97.9464950993983,-97.9370970894726,
-96.9377389559065,-95.9383808223405,-94.9390226887744,-93.9396645552084,
-92.9403064216423,-91.9409482880763,-91.6633097922187),.UNSPECIFIED.);
#799=B_SPLINE_CURVE_WITH_KNOTS('',3,(#38659,#38660,#38661,#38662,#38663,
#38664,#38665,#38666,#38667,#38668,#38669,#38670,#38671,#38672,#38673,#38674,
#38675,#38676,#38677,#38678,#38679,#38680),.UNSPECIFIED.,.F.,.F.,(4,3,3,
3,3,3,3,4),(88.4076549710687,88.9428738873782,89.9422320209442,90.9415901545103,
91.9409482880763,92.9403064216424,93.9396645552084,94.6908402782483),
 .UNSPECIFIED.);
#800=B_SPLINE_CURVE_WITH_KNOTS('',3,(#38685,#38686,#38687,#38688,#38689,
#38690,#38691,#38692,#38693,#38694,#38695,#38696,#38697,#38698,#38699,#38700,
#38701,#38702,#38703,#38704,#38705,#38706),.UNSPECIFIED.,.F.,.F.,(4,3,3,
3,3,3,3,4),(-104.229680406578,-103.933245890869,-102.933887757303,-101.934529623737,
-100.935171490171,-99.9358133566047,-98.9364552230386,-97.9464950993983),
 .UNSPECIFIED.);
#801=B_SPLINE_CURVE_WITH_KNOTS('',3,(#38707,#38708,#38709,#38710,#38711,
#38712,#38713,#38714,#38715,#38716,#38717,#38718,#38719,#38720,#38721,#38722,
#38723,#38724,#38725,#38726,#38727,#38728,#38729,#38730,#38731),
 .UNSPECIFIED.,.F.,.F.,(4,3,3,3,3,3,3,3,4),(94.6908402782483,94.9390226887745,
95.9383808223405,96.9377389559065,97.9370970894726,98.9364552230386,99.9358133566047,
100.935171490171,100.974025585428),.UNSPECIFIED.);
#802=B_SPLINE_CURVE_WITH_KNOTS('',3,(#38736,#38737,#38738,#38739,#38740,
#38741,#38742,#38743,#38744,#38745,#38746,#38747,#38748,#38749,#38750,#38751,
#38752,#38753,#38754,#38755,#38756,#38757),.UNSPECIFIED.,.F.,.F.,(4,3,3,
3,3,3,3,4),(-110.512865713757,-109.929394692265,-108.930036558699,-107.930678425133,
-106.931320291567,-105.931962158001,-104.932604024435,-104.229680406578),
 .UNSPECIFIED.);
#803=B_SPLINE_CURVE_WITH_KNOTS('',3,(#38758,#38759,#38760,#38761,#38762,
#38763,#38764,#38765,#38766,#38767,#38768,#38769,#38770,#38771,#38772,#38773,
#38774,#38775,#38776,#38777,#38778,#38779),.UNSPECIFIED.,.F.,.F.,(4,3,3,
3,3,3,3,4),(100.974025585428,101.934529623737,102.933887757303,103.933245890869,
104.932604024435,105.931962158001,106.931320291567,107.257210892608),
 .UNSPECIFIED.);
#804=B_SPLINE_CURVE_WITH_KNOTS('',3,(#38784,#38785,#38786,#38787,#38788,
#38789,#38790,#38791,#38792,#38793,#38794,#38795,#38796,#38797,#38798,#38799,
#38800,#38801,#38802,#38803,#38804,#38805),.UNSPECIFIED.,.F.,.F.,(4,3,3,
3,3,3,3,4),(-116.796051020937,-115.925543493661,-114.926185360095,-113.926827226529,
-112.927469092963,-111.928110959397,-110.928752825831,-110.512865713757),
 .UNSPECIFIED.);
#805=B_SPLINE_CURVE_WITH_KNOTS('',3,(#38806,#38807,#38808,#38809,#38810,
#38811,#38812,#38813,#38814,#38815,#38816,#38817,#38818,#38819,#38820,#38821,
#38822,#38823,#38824,#38825,#38826,#38827),.UNSPECIFIED.,.F.,.F.,(4,3,3,
3,3,3,3,4),(107.257210892608,107.930678425133,108.930036558699,109.929394692265,
110.928752825831,111.928110959397,112.927469092963,113.540396199787),
 .UNSPECIFIED.);
#806=B_SPLINE_CURVE_WITH_KNOTS('',3,(#38832,#38833,#38834,#38835,#38836,
#38837,#38838,#38839,#38840,#38841,#38842,#38843,#38844,#38845,#38846,#38847,
#38848,#38849,#38850,#38851,#38852,#38853,#38854,#38855,#38856),
 .UNSPECIFIED.,.F.,.F.,(4,3,3,3,3,3,3,3,4),(-123.079236328117,-122.921050428624,
-121.921692295058,-120.922334161492,-119.922976027926,-118.92361789436,
-117.924259760793,-116.924901627227,-116.796051020937),.UNSPECIFIED.);
#807=B_SPLINE_CURVE_WITH_KNOTS('',3,(#38857,#38858,#38859,#38860,#38861,
#38862,#38863,#38864,#38865,#38866,#38867,#38868,#38869,#38870,#38871,#38872,
#38873,#38874,#38875,#38876,#38877,#38878),.UNSPECIFIED.,.F.,.F.,(4,3,3,
3,3,3,3,4),(113.540396199787,113.926827226529,114.926185360095,115.925543493661,
116.924901627228,117.924259760794,118.92361789436,119.823581506967),
 .UNSPECIFIED.);
#808=B_SPLINE_CURVE_WITH_KNOTS('',3,(#38883,#38884,#38885,#38886,#38887,
#38888,#38889,#38890,#38891,#38892,#38893,#38894,#38895,#38896,#38897,#38898,
#38899,#38900,#38901,#38902,#38903,#38904),.UNSPECIFIED.,.F.,.F.,(4,3,3,
3,3,3,3,4),(-129.362421635296,-128.91719923002,-127.917841096454,-126.918482962888,
-125.919124829322,-124.919766695756,-123.92040856219,-123.079236328117),
 .UNSPECIFIED.);
#809=B_SPLINE_CURVE_WITH_KNOTS('',3,(#38905,#38906,#38907,#38908,#38909,
#38910,#38911,#38912,#38913,#38914,#38915,#38916,#38917,#38918,#38919,#38920,
#38921,#38922,#38923,#38924,#38925,#38926,#38927,#38928,#38929),
 .UNSPECIFIED.,.F.,.F.,(4,3,3,3,3,3,3,3,4),(119.823581506967,119.922976027926,
120.922334161492,121.921692295058,122.921050428624,123.92040856219,124.919766695756,
125.919124829322,126.106766814146),.UNSPECIFIED.);
#810=B_SPLINE_CURVE_WITH_KNOTS('',3,(#38934,#38935,#38936,#38937,#38938,
#38939,#38940,#38941,#38942,#38943,#38944,#38945,#38946,#38947,#38948,#38949,
#38950,#38951,#38952,#38953,#38954,#38955),.UNSPECIFIED.,.F.,.F.,(4,3,3,
3,3,3,3,4),(-135.645606942476,-134.913348031416,-133.91398989785,-132.914631764284,
-131.915273630718,-130.915915497152,-129.916557363586,-129.362421635296),
 .UNSPECIFIED.);
#811=B_SPLINE_CURVE_WITH_KNOTS('',3,(#38956,#38957,#38958,#38959,#38960,
#38961,#38962,#38963,#38964,#38965,#38966,#38967,#38968,#38969,#38970,#38971,
#38972,#38973,#38974,#38975,#38976,#38977),.UNSPECIFIED.,.F.,.F.,(4,3,3,
3,3,3,3,4),(126.106766814146,126.918482962888,127.917841096454,128.91719923002,
129.916557363586,130.915915497152,131.915273630718,132.389952121326),
 .UNSPECIFIED.);
#812=B_SPLINE_CURVE_WITH_KNOTS('',3,(#38982,#38983,#38984,#38985,#38986,
#38987,#38988,#38989,#38990,#38991,#38992,#38993,#38994,#38995,#38996,#38997,
#38998,#38999,#39000,#39001,#39002,#39003,#39004,#39005,#39006),
 .UNSPECIFIED.,.F.,.F.,(4,3,3,3,3,3,3,3,4),(-141.928792249655,-141.908854966379,
-140.909496832813,-139.910138699247,-138.91078056568,-137.911422432114,
-136.912064298548,-135.912706164982,-135.645606942476),.UNSPECIFIED.);
#813=B_SPLINE_CURVE_WITH_KNOTS('',3,(#39007,#39008,#39009,#39010,#39011,
#39012,#39013,#39014,#39015,#39016,#39017,#39018,#39019,#39020,#39021,#39022,
#39023,#39024,#39025,#39026,#39027,#39028),.UNSPECIFIED.,.F.,.F.,(4,3,3,
3,3,3,3,4),(132.389952121326,132.914631764284,133.91398989785,134.913348031416,
135.912706164982,136.912064298549,137.911422432115,138.673137428505),
 .UNSPECIFIED.);
#814=B_SPLINE_CURVE_WITH_KNOTS('',3,(#39033,#39034,#39035,#39036,#39037,
#39038,#39039,#39040,#39041,#39042,#39043,#39044,#39045,#39046,#39047,#39048,
#39049,#39050,#39051,#39052,#39053,#39054),.UNSPECIFIED.,.F.,.F.,(4,3,3,
3,3,3,3,4),(-148.211977556835,-147.905003767775,-146.905645634209,-145.906287500643,
-144.906929367077,-143.907571233511,-142.908213099945,-141.928792249655),
 .UNSPECIFIED.);
#815=B_SPLINE_CURVE_WITH_KNOTS('',3,(#39055,#39056,#39057,#39058,#39059,
#39060,#39061,#39062,#39063,#39064,#39065,#39066,#39067,#39068,#39069,#39070,
#39071,#39072,#39073,#39074,#39075,#39076,#39077,#39078,#39079),
 .UNSPECIFIED.,.F.,.F.,(4,3,3,3,3,3,3,3,4),(138.673137428505,138.910780565681,
139.910138699247,140.909496832813,141.908854966379,142.908213099945,143.907571233511,
144.906929367077,144.956322735685),.UNSPECIFIED.);
#816=B_SPLINE_CURVE_WITH_KNOTS('',3,(#39084,#39085,#39086,#39087,#39088,
#39089,#39090,#39091,#39092,#39093,#39094,#39095,#39096,#39097,#39098,#39099,
#39100,#39101,#39102,#39103,#39104,#39105),.UNSPECIFIED.,.F.,.F.,(4,3,3,
3,3,3,3,4),(-154.495162864015,-153.901152569171,-152.901794435605,-151.902436302039,
-150.903078168473,-149.903720034907,-148.904361901341,-148.211977556835),
 .UNSPECIFIED.);
#817=B_SPLINE_CURVE_WITH_KNOTS('',3,(#39106,#39107,#39108,#39109,#39110,
#39111,#39112,#39113,#39114,#39115,#39116,#39117,#39118,#39119,#39120,#39121,
#39122,#39123,#39124,#39125,#39126,#39127),.UNSPECIFIED.,.F.,.F.,(4,3,3,
3,3,3,3,4),(144.956322735685,145.906287500643,146.905645634209,147.905003767775,
148.904361901341,149.903720034907,150.903078168473,151.239508042865),
 .UNSPECIFIED.);
#818=B_SPLINE_CURVE_WITH_KNOTS('',3,(#39132,#39133,#39134,#39135,#39136,
#39137,#39138,#39139,#39140,#39141,#39142,#39143,#39144,#39145,#39146,#39147,
#39148,#39149,#39150,#39151,#39152,#39153),.UNSPECIFIED.,.F.,.F.,(4,3,3,
3,3,3,3,4),(-160.778348171194,-159.897301370567,-158.897943237001,-157.898585103435,
-156.899226969869,-155.899868836303,-154.900510702737,-154.495162864015),
 .UNSPECIFIED.);
#819=B_SPLINE_CURVE_WITH_KNOTS('',3,(#39154,#39155,#39156,#39157,#39158,
#39159,#39160,#39161,#39162,#39163,#39164,#39165,#39166,#39167,#39168,#39169,
#39170,#39171,#39172,#39173,#39174,#39175),.UNSPECIFIED.,.F.,.F.,(4,3,3,
3,3,3,3,4),(151.239508042865,151.902436302039,152.901794435605,153.901152569171,
154.900510702737,155.899868836303,156.899226969869,157.522693350044),
 .UNSPECIFIED.);
#820=B_SPLINE_CURVE_WITH_KNOTS('',3,(#39180,#39181,#39182,#39183,#39184,
#39185,#39186,#39187,#39188,#39189,#39190,#39191,#39192,#39193,#39194,#39195,
#39196,#39197,#39198,#39199,#39200,#39201,#39202,#39203,#39204),
 .UNSPECIFIED.,.F.,.F.,(4,3,3,3,3,3,3,3,4),(-167.061533478374,-166.89280830553,
-165.893450171964,-164.894092038398,-163.894733904832,-162.895375771266,
-161.8960176377,-160.896659504134,-160.778348171194),.UNSPECIFIED.);
#821=B_SPLINE_CURVE_WITH_KNOTS('',3,(#39205,#39206,#39207,#39208,#39209,
#39210,#39211,#39212,#39213,#39214,#39215,#39216,#39217,#39218,#39219,#39220,
#39221,#39222,#39223,#39224,#39225,#39226),.UNSPECIFIED.,.F.,.F.,(4,3,3,
3,3,3,3,4),(157.522693350044,157.898585103435,158.897943237002,159.897301370568,
160.896659504134,161.8960176377,162.895375771266,163.805878657224),
 .UNSPECIFIED.);
#822=B_SPLINE_CURVE_WITH_KNOTS('',3,(#39231,#39232,#39233,#39234,#39235,
#39236,#39237,#39238,#39239,#39240,#39241,#39242,#39243,#39244,#39245,#39246,
#39247,#39248,#39249,#39250,#39251,#39252),.UNSPECIFIED.,.F.,.F.,(4,3,3,
3,3,3,3,4),(-173.344718785553,-172.888957106926,-171.88959897336,-170.890240839794,
-169.890882706228,-168.891524572662,-167.892166439096,-167.061533478374),
 .UNSPECIFIED.);
#823=B_SPLINE_CURVE_WITH_KNOTS('',3,(#39253,#39254,#39255,#39256,#39257,
#39258,#39259,#39260,#39261,#39262,#39263,#39264,#39265,#39266,#39267,#39268,
#39269,#39270,#39271,#39272,#39273,#39274,#39275,#39276,#39277),
 .UNSPECIFIED.,.F.,.F.,(4,3,3,3,3,3,3,3,4),(163.805878657224,163.894733904832,
164.894092038398,165.893450171964,166.89280830553,167.892166439096,168.891524572662,
169.890882706228,170.089063964403),.UNSPECIFIED.);
#824=B_SPLINE_CURVE_WITH_KNOTS('',3,(#39282,#39283,#39284,#39285,#39286,
#39287,#39288,#39289,#39290,#39291,#39292,#39293,#39294,#39295,#39296,#39297,
#39298,#39299,#39300,#39301,#39302,#39303),.UNSPECIFIED.,.F.,.F.,(4,3,3,
3,3,3,3,4),(-179.627904092733,-178.885105908322,-177.885747774756,-176.88638964119,
-175.887031507624,-174.887673374058,-173.888315240492,-173.344718785553),
 .UNSPECIFIED.);
#825=B_SPLINE_CURVE_WITH_KNOTS('',3,(#39304,#39305,#39306,#39307,#39308,
#39309,#39310,#39311,#39312,#39313,#39314,#39315,#39316,#39317,#39318,#39319,
#39320,#39321,#39322,#39323,#39324,#39325),.UNSPECIFIED.,.F.,.F.,(4,3,3,
3,3,3,3,4),(170.089063964403,170.890240839794,171.88959897336,172.888957106926,
173.888315240492,174.887673374058,175.887031507624,176.372249271583),
 .UNSPECIFIED.);
#826=B_SPLINE_CURVE_WITH_KNOTS('',3,(#39330,#39331,#39332,#39333,#39334,
#39335,#39336,#39337,#39338,#39339,#39340,#39341,#39342,#39343,#39344,#39345,
#39346,#39347,#39348,#39349,#39350,#39351,#39352,#39353,#39354),
 .UNSPECIFIED.,.F.,.F.,(4,3,3,3,3,3,3,3,4),(-185.911089399912,-185.880612843285,
-184.881254709719,-183.881896576153,-182.882538442587,-181.88318030902,
-180.883822175454,-179.884464041888,-179.627904092733),.UNSPECIFIED.);
#827=B_SPLINE_CURVE_WITH_KNOTS('',3,(#39355,#39356,#39357,#39358,#39359,
#39360,#39361,#39362,#39363,#39364,#39365,#39366,#39367,#39368,#39369,#39370,
#39371,#39372,#39373,#39374,#39375,#39376),.UNSPECIFIED.,.F.,.F.,(4,3,3,
3,3,3,3,4),(176.372249271583,176.88638964119,177.885747774756,178.885105908322,
179.884464041889,180.883822175455,181.883180309021,182.655434578762),
 .UNSPECIFIED.);
#828=B_SPLINE_CURVE_WITH_KNOTS('',3,(#39381,#39382,#39383,#39384,#39385,
#39386,#39387,#39388,#39389,#39390,#39391,#39392,#39393,#39394,#39395,#39396,
#39397,#39398,#39399,#39400,#39401,#39402),.UNSPECIFIED.,.F.,.F.,(4,3,3,
3,3,3,3,4),(-192.194274707092,-191.876761644681,-190.877403511115,-189.878045377549,
-188.878687243983,-187.879329110417,-186.879970976851,-185.911089399912),
 .UNSPECIFIED.);
#829=B_SPLINE_CURVE_WITH_KNOTS('',3,(#39403,#39404,#39405,#39406,#39407,
#39408,#39409,#39410,#39411,#39412,#39413,#39414,#39415,#39416,#39417,#39418,
#39419,#39420,#39421,#39422,#39423,#39424,#39425,#39426,#39427),
 .UNSPECIFIED.,.F.,.F.,(4,3,3,3,3,3,3,3,4),(182.655434578762,182.882538442587,
183.881896576153,184.881254709719,185.880612843285,186.879970976851,187.879329110417,
188.878687243983,188.938619885942),.UNSPECIFIED.);
#830=B_SPLINE_CURVE_WITH_KNOTS('',3,(#39432,#39433,#39434,#39435,#39436,
#39437,#39438,#39439,#39440,#39441,#39442,#39443,#39444,#39445,#39446,#39447,
#39448,#39449,#39450,#39451,#39452,#39453),.UNSPECIFIED.,.F.,.F.,(4,3,3,
3,3,3,3,4),(-198.477460014271,-197.872910446077,-196.873552312511,-195.874194178945,
-194.874836045379,-193.875477911813,-192.876119778247,-192.194274707092),
 .UNSPECIFIED.);
#831=B_SPLINE_CURVE_WITH_KNOTS('',3,(#39454,#39455,#39456,#39457,#39458,
#39459,#39460,#39461,#39462,#39463,#39464,#39465,#39466,#39467,#39468,#39469,
#39470,#39471,#39472,#39473,#39474,#39475),.UNSPECIFIED.,.F.,.F.,(4,3,3,
3,3,3,3,4),(188.938619885942,189.878045377549,190.877403511115,191.876761644681,
192.876119778247,193.875477911813,194.874836045379,195.221805193122),
 .UNSPECIFIED.);
#832=B_SPLINE_CURVE_WITH_KNOTS('',3,(#39480,#39481,#39482,#39483,#39484,
#39485,#39486,#39487,#39488,#39489,#39490,#39491,#39492,#39493,#39494,#39495,
#39496,#39497,#39498,#39499,#39500,#39501),.UNSPECIFIED.,.F.,.F.,(4,3,3,
3,3,3,3,4),(-204.760645321451,-203.869059247473,-202.869701113907,-201.870342980341,
-200.870984846775,-199.871626713209,-198.872268579643,-198.477460014271),
 .UNSPECIFIED.);
#833=B_SPLINE_CURVE_WITH_KNOTS('',3,(#39502,#39503,#39504,#39505,#39506,
#39507,#39508,#39509,#39510,#39511,#39512,#39513,#39514,#39515,#39516,#39517,
#39518,#39519,#39520,#39521,#39522,#39523),.UNSPECIFIED.,.F.,.F.,(4,3,3,
3,3,3,3,4),(195.221805193122,195.874194178945,196.873552312511,197.872910446077,
198.872268579643,199.871626713209,200.870984846776,201.504990500301),
 .UNSPECIFIED.);
#834=B_SPLINE_CURVE_WITH_KNOTS('',3,(#39528,#39529,#39530,#39531,#39532,
#39533,#39534,#39535,#39536,#39537,#39538,#39539,#39540,#39541,#39542,#39543,
#39544,#39545,#39546,#39547,#39548,#39549,#39550,#39551,#39552),
 .UNSPECIFIED.,.F.,.F.,(4,3,3,3,3,3,3,3,4),(-211.043830628631,-210.864566182436,
-209.86520804887,-208.865849915304,-207.866491781738,-206.867133648172,
-205.867775514606,-204.86841738104,-204.760645321451),.UNSPECIFIED.);
#835=B_SPLINE_CURVE_WITH_KNOTS('',3,(#39553,#39554,#39555,#39556,#39557,
#39558,#39559,#39560,#39561,#39562,#39563,#39564,#39565,#39566,#39567,#39568,
#39569,#39570,#39571,#39572,#39573,#39574),.UNSPECIFIED.,.F.,.F.,(4,3,3,
3,3,3,3,4),(201.504990500301,201.870342980342,202.869701113908,203.869059247474,
204.86841738104,205.867775514606,206.867133648172,207.788175807481),
 .UNSPECIFIED.);
#836=B_SPLINE_CURVE_WITH_KNOTS('',3,(#39579,#39580,#39581,#39582,#39583,
#39584,#39585,#39586,#39587,#39588,#39589,#39590,#39591,#39592,#39593,#39594,
#39595,#39596,#39597,#39598,#39599,#39600),.UNSPECIFIED.,.F.,.F.,(4,3,3,
3,3,3,3,4),(-217.32701593581,-216.860714983832,-215.861356850266,-214.8619987167,
-213.862640583134,-212.863282449568,-211.863924316002,-211.043830628631),
 .UNSPECIFIED.);
#837=B_SPLINE_CURVE_WITH_KNOTS('',3,(#39601,#39602,#39603,#39604,#39605,
#39606,#39607,#39608,#39609,#39610,#39611,#39612,#39613,#39614,#39615,#39616,
#39617,#39618,#39619,#39620,#39621,#39622,#39623,#39624,#39625),
 .UNSPECIFIED.,.F.,.F.,(4,3,3,3,3,3,3,3,4),(207.788175807481,207.866491781738,
208.865849915304,209.86520804887,210.864566182436,211.863924316002,212.863282449568,
213.862640583134,214.07136111466),.UNSPECIFIED.);
#838=B_SPLINE_CURVE_WITH_KNOTS('',3,(#39630,#39631,#39632,#39633,#39634,
#39635,#39636,#39637,#39638,#39639,#39640,#39641,#39642,#39643,#39644,#39645,
#39646,#39647,#39648,#39649,#39650,#39651),.UNSPECIFIED.,.F.,.F.,(4,3,3,
3,3,3,3,4),(-223.61020124299,-222.856863785228,-221.857505651662,-220.858147518096,
-219.85878938453,-218.859431250964,-217.860073117398,-217.32701593581),
 .UNSPECIFIED.);
#839=B_SPLINE_CURVE_WITH_KNOTS('',3,(#39652,#39653,#39654,#39655,#39656,
#39657,#39658,#39659,#39660,#39661,#39662,#39663,#39664,#39665,#39666,#39667,
#39668,#39669,#39670,#39671,#39672,#39673),.UNSPECIFIED.,.F.,.F.,(4,3,3,
3,3,3,3,4),(214.07136111466,214.8619987167,215.861356850266,216.860714983832,
217.860073117398,218.859431250964,219.85878938453,220.35454642184),
 .UNSPECIFIED.);
#840=B_SPLINE_CURVE_WITH_KNOTS('',3,(#39678,#39679,#39680,#39681,#39682,
#39683,#39684,#39685,#39686,#39687,#39688,#39689,#39690,#39691,#39692,#39693,
#39694,#39695,#39696,#39697,#39698,#39699,#39700,#39701,#39702),
 .UNSPECIFIED.,.F.,.F.,(4,3,3,3,3,3,3,3,4),(-229.893386550169,-229.852370720191,
-228.853012586625,-227.853654453059,-226.854296319493,-225.854938185927,
-224.85558005236,-223.856221918794,-223.61020124299),.UNSPECIFIED.);
#841=B_SPLINE_CURVE_WITH_KNOTS('',3,(#39703,#39704,#39705,#39706,#39707,
#39708,#39709,#39710,#39711,#39712,#39713,#39714,#39715,#39716,#39717,#39718,
#39719,#39720,#39721,#39722,#39723,#39724),.UNSPECIFIED.,.F.,.F.,(4,3,3,
3,3,3,3,4),(220.35454642184,220.858147518096,221.857505651663,222.856863785229,
223.856221918795,224.855580052361,225.854938185927,226.637731729019),
 .UNSPECIFIED.);
#842=B_SPLINE_CURVE_WITH_KNOTS('',3,(#39729,#39730,#39731,#39732,#39733,
#39734,#39735,#39736,#39737,#39738,#39739,#39740,#39741,#39742,#39743,#39744,
#39745,#39746,#39747,#39748,#39749,#39750),.UNSPECIFIED.,.F.,.F.,(4,3,3,
3,3,3,3,4),(-236.176571857349,-235.848519521587,-234.849161388021,-233.849803254455,
-232.850445120889,-231.851086987323,-230.851728853757,-229.893386550169),
 .UNSPECIFIED.);
#843=B_SPLINE_CURVE_WITH_KNOTS('',3,(#39751,#39752,#39753,#39754,#39755,
#39756,#39757,#39758,#39759,#39760,#39761,#39762,#39763,#39764,#39765,#39766,
#39767,#39768,#39769,#39770,#39771,#39772,#39773,#39774,#39775),
 .UNSPECIFIED.,.F.,.F.,(4,3,3,3,3,3,3,3,4),(226.637731729019,226.854296319493,
227.853654453059,228.853012586625,229.852370720191,230.851728853757,231.851086987323,
232.850445120889,232.920917036199),.UNSPECIFIED.);
#844=B_SPLINE_CURVE_WITH_KNOTS('',3,(#39780,#39781,#39782,#39783,#39784,
#39785,#39786,#39787,#39788,#39789,#39790,#39791,#39792,#39793,#39794,#39795,
#39796,#39797,#39798,#39799,#39800,#39801),.UNSPECIFIED.,.F.,.F.,(4,3,3,
3,3,3,3,4),(-242.459757164528,-241.844668322983,-240.845310189417,-239.845952055851,
-238.846593922285,-237.847235788719,-236.847877655153,-236.176571857349),
 .UNSPECIFIED.);
#845=B_SPLINE_CURVE_WITH_KNOTS('',3,(#39802,#39803,#39804,#39805,#39806,
#39807,#39808,#39809,#39810,#39811,#39812,#39813,#39814,#39815,#39816,#39817,
#39818,#39819,#39820,#39821,#39822,#39823),.UNSPECIFIED.,.F.,.F.,(4,3,3,
3,3,3,3,4),(232.920917036199,233.849803254455,234.849161388021,235.848519521587,
236.847877655153,237.847235788719,238.846593922285,239.204102343378),
 .UNSPECIFIED.);
#846=B_SPLINE_CURVE_WITH_KNOTS('',3,(#39828,#39829,#39830,#39831,#39832,
#39833,#39834,#39835,#39836,#39837,#39838,#39839,#39840,#39841,#39842,#39843,
#39844,#39845,#39846,#39847,#39848,#39849),.UNSPECIFIED.,.F.,.F.,(4,3,3,
3,3,3,3,4),(-248.742942471708,-247.84081712438,-246.841458990814,-245.842100857247,
-244.842742723681,-243.843384590115,-242.844026456549,-242.459757164528),
 .UNSPECIFIED.);
#847=B_SPLINE_CURVE_WITH_KNOTS('',3,(#39850,#39851,#39852,#39853,#39854,
#39855,#39856,#39857,#39858,#39859,#39860,#39861,#39862,#39863,#39864,#39865,
#39866,#39867,#39868,#39869,#39870,#39871),.UNSPECIFIED.,.F.,.F.,(4,3,3,
3,3,3,3,4),(239.204102343378,239.845952055851,240.845310189417,241.844668322983,
242.84402645655,243.843384590116,244.842742723682,245.487287650558),
 .UNSPECIFIED.);
#848=B_SPLINE_CURVE_WITH_KNOTS('',3,(#39876,#39877,#39878,#39879,#39880,
#39881,#39882,#39883,#39884,#39885,#39886,#39887,#39888,#39889,#39890,#39891,
#39892,#39893,#39894,#39895,#39896,#39897,#39898,#39899,#39900),
 .UNSPECIFIED.,.F.,.F.,(4,3,3,3,3,3,3,3,4),(-255.026127778888,-254.836324059342,
-253.836965925776,-252.83760779221,-251.838249658644,-250.838891525078,
-249.839533391512,-248.840175257946,-248.742942471708),.UNSPECIFIED.);
#849=B_SPLINE_CURVE_WITH_KNOTS('',3,(#39901,#39902,#39903,#39904,#39905,
#39906,#39907,#39908,#39909,#39910,#39911,#39912,#39913,#39914,#39915,#39916,
#39917,#39918,#39919,#39920,#39921,#39922),.UNSPECIFIED.,.F.,.F.,(4,3,3,
3,3,3,3,4),(245.487287650558,245.842100857248,246.841458990814,247.84081712438,
248.840175257946,249.839533391512,250.838891525078,251.770472957738),
 .UNSPECIFIED.);
#850=B_SPLINE_CURVE_WITH_KNOTS('',3,(#39927,#39928,#39929,#39930,#39931,
#39932,#39933,#39934,#39935,#39936,#39937,#39938,#39939,#39940,#39941,#39942,
#39943,#39944,#39945,#39946,#39947,#39948),.UNSPECIFIED.,.F.,.F.,(4,3,3,
3,3,3,3,4),(-261.309313086067,-260.832472860738,-259.833114727172,-258.833756593606,
-257.83439846004,-256.835040326474,-255.835682192908,-255.026127778888),
 .UNSPECIFIED.);
#851=B_SPLINE_CURVE_WITH_KNOTS('',3,(#39949,#39950,#39951,#39952,#39953,
#39954,#39955,#39956,#39957,#39958,#39959,#39960,#39961,#39962,#39963,#39964,
#39965,#39966,#39967,#39968,#39969,#39970,#39971,#39972,#39973),
 .UNSPECIFIED.,.F.,.F.,(4,3,3,3,3,3,3,3,4),(251.770472957738,251.838249658644,
252.83760779221,253.836965925776,254.836324059342,255.835682192908,256.835040326474,
257.83439846004,258.053658264917),.UNSPECIFIED.);
#852=B_SPLINE_CURVE_WITH_KNOTS('',3,(#39978,#39979,#39980,#39981,#39982,
#39983,#39984,#39985,#39986,#39987,#39988,#39989,#39990,#39991,#39992,#39993,
#39994,#39995,#39996,#39997,#39998,#39999),.UNSPECIFIED.,.F.,.F.,(4,3,3,
3,3,3,3,4),(-267.592498393247,-266.828621662134,-265.829263528568,-264.829905395002,
-263.830547261436,-262.83118912787,-261.831830994304,-261.309313086067),
 .UNSPECIFIED.);
#853=B_SPLINE_CURVE_WITH_KNOTS('',3,(#40000,#40001,#40002,#40003,#40004,
#40005,#40006,#40007,#40008,#40009,#40010,#40011,#40012,#40013,#40014,#40015,
#40016,#40017,#40018,#40019,#40020,#40021),.UNSPECIFIED.,.F.,.F.,(4,3,3,
3,3,3,3,4),(258.053658264917,258.833756593606,259.833114727172,260.832472860738,
261.831830994304,262.83118912787,263.830547261436,264.336843572097),
 .UNSPECIFIED.);
#854=B_SPLINE_CURVE_WITH_KNOTS('',3,(#40026,#40027,#40028,#40029,#40030,
#40031,#40032,#40033,#40034,#40035,#40036,#40037,#40038,#40039,#40040,#40041,
#40042,#40043,#40044,#40045,#40046,#40047,#40048,#40049,#40050),
 .UNSPECIFIED.,.F.,.F.,(4,3,3,3,3,3,3,3,4),(-273.875683700426,-273.824128597097,
-272.824770463531,-271.825412329965,-270.826054196399,-269.826696062833,
-268.827337929266,-267.8279797957,-267.592498393247),.UNSPECIFIED.);
#855=B_SPLINE_CURVE_WITH_KNOTS('',3,(#40051,#40052,#40053,#40054,#40055,
#40056,#40057,#40058,#40059,#40060,#40061,#40062,#40063,#40064,#40065,#40066,
#40067,#40068,#40069,#40070,#40071,#40072),.UNSPECIFIED.,.F.,.F.,(4,3,3,
3,3,3,3,4),(264.336843572097,264.829905395003,265.829263528569,266.828621662135,
267.827979795701,268.827337929267,269.826696062833,270.620028879276),
 .UNSPECIFIED.);
#856=B_SPLINE_CURVE_WITH_KNOTS('',3,(#40077,#40078,#40079,#40080,#40081,
#40082,#40083,#40084,#40085,#40086,#40087,#40088,#40089,#40090,#40091,#40092,
#40093,#40094,#40095,#40096,#40097,#40098),.UNSPECIFIED.,.F.,.F.,(4,3,3,
3,3,3,3,4),(-280.158869007606,-279.820277398493,-278.820919264927,-277.821561131361,
-276.822202997795,-275.822844864229,-274.823486730663,-273.875683700426),
 .UNSPECIFIED.);
#857=B_SPLINE_CURVE_WITH_KNOTS('',3,(#40099,#40100,#40101,#40102,#40103,
#40104,#40105,#40106,#40107,#40108,#40109,#40110,#40111,#40112,#40113,#40114,
#40115,#40116,#40117,#40118,#40119,#40120,#40121,#40122,#40123),
 .UNSPECIFIED.,.F.,.F.,(4,3,3,3,3,3,3,3,4),(270.620028879276,270.826054196399,
271.825412329965,272.824770463531,273.824128597097,274.823486730663,275.822844864229,
276.822202997795,276.903214186456),.UNSPECIFIED.);
#858=B_SPLINE_CURVE_WITH_KNOTS('',3,(#40128,#40129,#40130,#40131,#40132,
#40133,#40134,#40135,#40136,#40137,#40138,#40139,#40140,#40141,#40142,#40143,
#40144,#40145,#40146,#40147,#40148,#40149),.UNSPECIFIED.,.F.,.F.,(4,3,3,
3,3,3,3,4),(-286.442054314785,-285.816426199889,-284.817068066323,-283.817709932757,
-282.818351799191,-281.818993665625,-280.819635532059,-280.158869007606),
 .UNSPECIFIED.);
#859=B_SPLINE_CURVE_WITH_KNOTS('',3,(#40150,#40151,#40152,#40153,#40154,
#40155,#40156,#40157,#40158,#40159,#40160,#40161,#40162,#40163,#40164,#40165,
#40166,#40167,#40168,#40169,#40170,#40171),.UNSPECIFIED.,.F.,.F.,(4,3,3,
3,3,3,3,4),(276.903214186456,277.821561131361,278.820919264927,279.820277398493,
280.819635532059,281.818993665625,282.818351799191,283.186399493635),
 .UNSPECIFIED.);
#860=B_SPLINE_CURVE_WITH_KNOTS('',3,(#40176,#40177,#40178,#40179,#40180,
#40181,#40182,#40183,#40184,#40185,#40186,#40187,#40188,#40189,#40190,#40191,
#40192,#40193,#40194,#40195,#40196,#40197),.UNSPECIFIED.,.F.,.F.,(4,3,3,
3,3,3,3,4),(-292.725239621965,-291.812575001286,-290.81321686772,-289.813858734153,
-288.814500600587,-287.815142467021,-286.815784333455,-286.442054314785),
 .UNSPECIFIED.);
#861=B_SPLINE_CURVE_WITH_KNOTS('',3,(#40198,#40199,#40200,#40201,#40202,
#40203,#40204,#40205,#40206,#40207,#40208,#40209,#40210,#40211,#40212,#40213,
#40214,#40215,#40216,#40217,#40218,#40219),.UNSPECIFIED.,.F.,.F.,(4,3,3,
3,3,3,3,4),(283.186399493635,283.817709932757,284.817068066323,285.81642619989,
286.815784333456,287.815142467022,288.814500600588,289.469584800815),
 .UNSPECIFIED.);
#862=B_SPLINE_CURVE_WITH_KNOTS('',3,(#40224,#40225,#40226,#40227,#40228,
#40229,#40230,#40231,#40232,#40233,#40234,#40235,#40236,#40237,#40238,#40239,
#40240,#40241,#40242,#40243,#40244,#40245,#40246,#40247,#40248),
 .UNSPECIFIED.,.F.,.F.,(4,3,3,3,3,3,3,3,4),(-299.008424929145,-298.808081936248,
-297.808723802682,-296.809365669116,-295.81000753555,-294.810649401984,
-293.811291268418,-292.811933134852,-292.725239621965),.UNSPECIFIED.);
#863=B_SPLINE_CURVE_WITH_KNOTS('',3,(#40249,#40250,#40251,#40252,#40253,
#40254,#40255,#40256,#40257,#40258,#40259,#40260,#40261,#40262,#40263,#40264,
#40265,#40266,#40267,#40268,#40269,#40270),.UNSPECIFIED.,.F.,.F.,(4,3,3,
3,3,3,3,4),(289.469584800815,289.813858734154,290.81321686772,291.812575001286,
292.811933134852,293.811291268418,294.810649401984,295.752770107995),
 .UNSPECIFIED.);
#864=B_SPLINE_CURVE_WITH_KNOTS('',3,(#40275,#40276,#40277,#40278,#40279,
#40280,#40281,#40282,#40283,#40284,#40285,#40286,#40287,#40288,#40289,#40290,
#40291,#40292,#40293,#40294,#40295,#40296),.UNSPECIFIED.,.F.,.F.,(4,3,3,
3,3,3,3,4),(-305.291610236324,-304.804230737644,-303.804872604078,-302.805514470512,
-301.806156336946,-300.80679820338,-299.807440069814,-299.008424929145),
 .UNSPECIFIED.);
#865=B_SPLINE_CURVE_WITH_KNOTS('',3,(#40297,#40298,#40299,#40300,#40301,
#40302,#40303,#40304,#40305,#40306,#40307,#40308,#40309,#40310,#40311,#40312,
#40313,#40314,#40315,#40316,#40317,#40318,#40319,#40320,#40321),
 .UNSPECIFIED.,.F.,.F.,(4,3,3,3,3,3,3,3,4),(295.752770107995,295.81000753555,
296.809365669116,297.808723802682,298.808081936248,299.807440069814,300.80679820338,
301.806156336946,302.035955415174),.UNSPECIFIED.);
#866=B_SPLINE_CURVE_WITH_KNOTS('',3,(#40326,#40327,#40328,#40329,#40330,
#40331,#40332,#40333,#40334,#40335,#40336,#40337,#40338,#40339,#40340,#40341,
#40342,#40343,#40344,#40345,#40346,#40347),.UNSPECIFIED.,.F.,.F.,(4,3,3,
3,3,3,3,4),(-311.574795543504,-310.80037953904,-309.801021405475,-308.801663271908,
-307.802305138342,-306.802947004776,-305.80358887121,-305.291610236324),
 .UNSPECIFIED.);
#867=B_SPLINE_CURVE_WITH_KNOTS('',3,(#40348,#40349,#40350,#40351,#40352,
#40353,#40354,#40355,#40356,#40357,#40358,#40359,#40360,#40361,#40362,#40363,
#40364,#40365,#40366,#40367,#40368,#40369),.UNSPECIFIED.,.F.,.F.,(4,3,3,
3,3,3,3,4),(302.035955415174,302.805514470512,303.804872604078,304.804230737644,
305.80358887121,306.802947004777,307.802305138343,308.319140722354),
 .UNSPECIFIED.);
#868=B_SPLINE_CURVE_WITH_KNOTS('',3,(#40374,#40375,#40376,#40377,#40378,
#40379,#40380,#40381,#40382,#40383,#40384,#40385,#40386,#40387,#40388,#40389,
#40390,#40391,#40392,#40393,#40394,#40395,#40396,#40397,#40398),
 .UNSPECIFIED.,.F.,.F.,(4,3,3,3,3,3,3,3,4),(-317.857980850683,-317.795886474003,
-316.796528340437,-315.797170206871,-314.797812073305,-313.798453939739,
-312.799095806173,-311.799737672607,-311.574795543504),.UNSPECIFIED.);
#869=B_SPLINE_CURVE_WITH_KNOTS('',3,(#40399,#40400,#40401,#40402,#40403,
#40404,#40405,#40406,#40407,#40408,#40409,#40410,#40411,#40412,#40413,#40414,
#40415,#40416,#40417,#40418,#40419,#40420),.UNSPECIFIED.,.F.,.F.,(4,3,3,
3,3,3,3,4),(308.319140722354,308.801663271909,309.801021405475,310.800379539041,
311.799737672607,312.799095806173,313.798453939739,314.602326029533),
 .UNSPECIFIED.);
#870=B_SPLINE_CURVE_WITH_KNOTS('',3,(#40425,#40426,#40427,#40428,#40429,
#40430,#40431,#40432,#40433,#40434,#40435,#40436,#40437,#40438,#40439,#40440,
#40441,#40442,#40443,#40444,#40445,#40446),.UNSPECIFIED.,.F.,.F.,(4,3,3,
3,3,3,3,4),(-324.141166157863,-323.792035275399,-322.792677141833,-321.793319008267,
-320.793960874701,-319.794602741135,-318.795244607569,-317.857980850683),
 .UNSPECIFIED.);
#871=B_SPLINE_CURVE_WITH_KNOTS('',3,(#40447,#40448,#40449,#40450,#40451,
#40452,#40453,#40454,#40455,#40456,#40457,#40458,#40459,#40460,#40461,#40462,
#40463,#40464,#40465,#40466,#40467,#40468,#40469,#40470,#40471),
 .UNSPECIFIED.,.F.,.F.,(4,3,3,3,3,3,3,3,4),(314.602326029533,314.797812073305,
315.797170206871,316.796528340437,317.795886474003,318.795244607569,319.794602741135,
320.793960874701,320.885511336713),.UNSPECIFIED.);
#872=B_SPLINE_CURVE_WITH_KNOTS('',3,(#40476,#40477,#40478,#40479,#40480,
#40481,#40482,#40483,#40484,#40485,#40486,#40487,#40488,#40489,#40490,#40491,
#40492,#40493,#40494,#40495,#40496,#40497),.UNSPECIFIED.,.F.,.F.,(4,3,3,
3,3,3,3,4),(-330.424351465042,-329.788184076795,-328.788825943229,-327.789467809663,
-326.790109676097,-325.790751542531,-324.791393408965,-324.141166157863),
 .UNSPECIFIED.);
#873=B_SPLINE_CURVE_WITH_KNOTS('',3,(#40498,#40499,#40500,#40501,#40502,
#40503,#40504,#40505,#40506,#40507,#40508,#40509,#40510,#40511,#40512,#40513,
#40514,#40515,#40516,#40517,#40518,#40519),.UNSPECIFIED.,.F.,.F.,(4,3,3,
3,3,3,3,4),(320.885511336713,321.793319008267,322.792677141833,323.792035275399,
324.791393408965,325.790751542531,326.790109676097,327.168696643892),
 .UNSPECIFIED.);
#874=B_SPLINE_CURVE_WITH_KNOTS('',3,(#40524,#40525,#40526,#40527,#40528,
#40529,#40530,#40531,#40532,#40533,#40534,#40535,#40536,#40537,#40538,#40539,
#40540,#40541,#40542,#40543,#40544,#40545),.UNSPECIFIED.,.F.,.F.,(4,3,3,
3,3,3,3,4),(-336.707536772222,-335.784332878192,-334.784974744626,-333.78561661106,
-332.786258477494,-331.786900343927,-330.787542210361,-330.424351465042),
 .UNSPECIFIED.);
#875=B_SPLINE_CURVE_WITH_KNOTS('',3,(#40546,#40547,#40548,#40549,#40550,
#40551,#40552,#40553,#40554,#40555,#40556,#40557,#40558,#40559,#40560,#40561,
#40562,#40563,#40564,#40565,#40566,#40567),.UNSPECIFIED.,.F.,.F.,(4,3,3,
3,3,3,3,4),(327.168696643892,327.789467809663,328.78882594323,329.788184076796,
330.787542210362,331.786900343928,332.786258477494,333.451881951072),
 .UNSPECIFIED.);
#876=B_SPLINE_CURVE_WITH_KNOTS('',3,(#40572,#40573,#40574,#40575,#40576,
#40577,#40578,#40579,#40580,#40581,#40582,#40583,#40584,#40585,#40586,#40587,
#40588,#40589,#40590,#40591,#40592,#40593,#40594,#40595,#40596),
 .UNSPECIFIED.,.F.,.F.,(4,3,3,3,3,3,3,3,4),(-342.990722079402,-342.779839813154,
-341.780481679588,-340.781123546022,-339.781765412456,-338.78240727889,
-337.783049145324,-336.783691011758,-336.707536772222),.UNSPECIFIED.);
#877=B_SPLINE_CURVE_WITH_KNOTS('',3,(#40597,#40598,#40599,#40600,#40601,
#40602,#40603,#40604,#40605,#40606,#40607,#40608,#40609,#40610,#40611,#40612,
#40613,#40614,#40615,#40616,#40617,#40618),.UNSPECIFIED.,.F.,.F.,(4,3,3,
3,3,3,3,4),(333.451881951072,333.78561661106,334.784974744626,335.784332878192,
336.783691011758,337.783049145324,338.78240727889,339.735067258252),
 .UNSPECIFIED.);
#878=B_SPLINE_CURVE_WITH_KNOTS('',3,(#40623,#40624,#40625,#40626,#40627,
#40628,#40629,#40630,#40631,#40632,#40633,#40634,#40635,#40636,#40637,#40638,
#40639,#40640,#40641,#40642,#40643,#40644,#40645,#40646,#40647,#40648,#40649,
#40650,#40651,#40652,#40653,#40654,#40655,#40656),.UNSPECIFIED.,.F.,.F.,
(4,3,3,3,3,3,3,3,3,3,3,4),(-349.273907386581,-348.77598861455,-348.276309547767,
-347.776630480984,-347.276951414201,-346.777272347418,-346.277593280635,
-345.777914213852,-345.278235147069,-344.778556080286,-343.77919794672,
-342.990722079402),.UNSPECIFIED.);
#879=B_SPLINE_CURVE_WITH_KNOTS('',3,(#40657,#40658,#40659,#40660,#40661,
#40662,#40663,#40664,#40665,#40666,#40667,#40668,#40669,#40670,#40671,#40672,
#40673,#40674,#40675,#40676,#40677,#40678,#40679,#40680,#40681,#40682,#40683,
#40684),.UNSPECIFIED.,.F.,.F.,(4,3,3,3,3,3,3,3,3,4),(339.735067258252,339.781765412456,
340.781123546022,341.780481679588,342.779839813154,343.77919794672,344.778556080286,
345.278235147069,345.777914213852,346.018252565431),.UNSPECIFIED.);
#880=B_SPLINE_CURVE_WITH_KNOTS('',3,(#40689,#40690,#40691,#40692,#40693,
#40694,#40695,#40696,#40697,#40698,#40699,#40700,#40701,#40702,#40703,#40704,
#40705,#40706,#40707,#40708,#40709,#40710,#40711,#40712,#40713,#40714,#40715,
#40716,#40717,#40718,#40719,#40720,#40721,#40722,#40723,#40724,#40725,#40726,
#40727,#40728,#40729,#40730,#40731),.UNSPECIFIED.,.F.,.F.,(4,3,3,3,3,3,
3,3,3,3,3,3,3,3,4),(-355.557092693761,-355.27181648273,-354.772137415947,
-354.272458349164,-353.77277928238,-353.273100215597,-352.773421148814,
-352.273742082031,-351.774063015248,-351.274383948465,-350.774704881682,
-350.275025814899,-349.775346748116,-349.275667681333,-349.273907386581),
 .UNSPECIFIED.);
#881=B_SPLINE_CURVE_WITH_KNOTS('',3,(#40732,#40733,#40734,#40735,#40736,
#40737,#40738,#40739,#40740,#40741,#40742,#40743,#40744,#40745,#40746,#40747,
#40748,#40749,#40750,#40751,#40752,#40753,#40754,#40755,#40756,#40757,#40758,
#40759,#40760,#40761,#40762,#40763,#40764,#40765,#40766,#40767,#40768,#40769,
#40770,#40771,#40772,#40773,#40774),.UNSPECIFIED.,.F.,.F.,(4,3,3,3,3,3,
3,3,3,3,3,3,3,3,4),(346.018252565431,346.277593280635,346.777272347418,
347.276951414201,347.776630480984,348.276309547767,348.77598861455,349.275667681334,
349.775346748116,350.2750258149,350.774704881683,351.274383948466,351.774063015249,
352.273742082032,352.301437872611),.UNSPECIFIED.);
#882=B_SPLINE_CURVE_WITH_KNOTS('',3,(#40779,#40780,#40781,#40782,#40783,
#40784,#40785,#40786,#40787,#40788,#40789,#40790,#40791,#40792,#40793,#40794,
#40795,#40796,#40797,#40798,#40799,#40800,#40801,#40802,#40803,#40804,#40805,
#40806,#40807,#40808,#40809,#40810,#40811,#40812,#40813,#40814,#40815,#40816,
#40817,#40818,#40819,#40820,#40821),.UNSPECIFIED.,.F.,.F.,(4,3,3,3,3,3,
3,3,3,3,3,3,3,3,4),(-361.84027800094,-361.767644350909,-361.267965284126,
-360.768286217343,-360.26860715056,-359.768928083777,-359.269249016994,
-358.769569950211,-358.269890883428,-357.770211816645,-357.270532749862,
-356.770853683079,-356.271174616296,-355.771495549513,-355.557092693761),
 .UNSPECIFIED.);
#883=B_SPLINE_CURVE_WITH_KNOTS('',3,(#40822,#40823,#40824,#40825,#40826,
#40827,#40828,#40829,#40830,#40831,#40832,#40833,#40834,#40835,#40836,#40837,
#40838,#40839,#40840,#40841,#40842,#40843,#40844,#40845,#40846,#40847,#40848,
#40849,#40850,#40851,#40852,#40853,#40854,#40855,#40856,#40857,#40858,#40859,
#40860,#40861),.UNSPECIFIED.,.F.,.F.,(4,3,3,3,3,3,3,3,3,3,3,3,3,4),(352.301437872611,
352.773421148815,353.273100215598,353.772779282381,354.272458349164,354.772137415947,
355.27181648273,355.771495549513,356.271174616296,356.770853683079,357.270532749862,
357.770211816645,358.269890883428,358.58462317979),.UNSPECIFIED.);
#884=B_SPLINE_CURVE_WITH_KNOTS('',3,(#40866,#40867,#40868,#40869,#40870,
#40871,#40872,#40873,#40874,#40875,#40876,#40877,#40878,#40879,#40880,#40881,
#40882,#40883,#40884,#40885,#40886,#40887,#40888,#40889,#40890,#40891,#40892,
#40893,#40894,#40895,#40896,#40897,#40898,#40899,#40900,#40901,#40902,#40903,
#40904,#40905),.UNSPECIFIED.,.F.,.F.,(4,3,3,3,3,3,3,3,3,3,3,3,3,4),(-368.12346330812,
-367.763793152305,-367.264114085522,-366.764435018739,-366.264755951956,
-365.765076885173,-365.26539781839,-364.765718751607,-364.266039684824,
-363.766360618041,-363.266681551258,-362.767002484475,-362.267323417692,
-361.84027800094),.UNSPECIFIED.);
#885=B_SPLINE_CURVE_WITH_KNOTS('',3,(#40906,#40907,#40908,#40909,#40910,
#40911,#40912,#40913,#40914,#40915,#40916,#40917,#40918,#40919,#40920,#40921,
#40922,#40923,#40924,#40925,#40926,#40927,#40928,#40929,#40930,#40931,#40932,
#40933,#40934,#40935,#40936,#40937,#40938,#40939,#40940,#40941,#40942,#40943,
#40944,#40945,#40946,#40947,#40948),.UNSPECIFIED.,.F.,.F.,(4,3,3,3,3,3,
3,3,3,3,3,3,3,3,4),(358.58462317979,358.769569950211,359.269249016994,359.768928083777,
360.26860715056,360.768286217343,361.267965284126,361.767644350909,362.267323417692,
362.767002484475,363.266681551258,363.766360618041,364.266039684824,364.765718751607,
364.86780848697),.UNSPECIFIED.);
#886=B_SPLINE_CURVE_WITH_KNOTS('',3,(#40953,#40954,#40955,#40956,#40957,
#40958,#40959,#40960,#40961,#40962,#40963,#40964,#40965,#40966,#40967,#40968,
#40969,#40970,#40971,#40972,#40973,#40974,#40975,#40976,#40977,#40978,#40979,
#40980,#40981,#40982,#40983,#40984,#40985,#40986,#40987,#40988,#40989,#40990,
#40991,#40992,#40993,#40994,#40995),.UNSPECIFIED.,.F.,.F.,(4,3,3,3,3,3,
3,3,3,3,3,3,3,3,4),(-374.406648615299,-374.259621020484,-373.759941953701,
-373.260262886918,-372.760583820135,-372.260904753352,-371.761225686569,
-371.261546619786,-370.761867553003,-370.26218848622,-369.762509419437,
-369.262830352654,-368.763151285871,-368.263472219088,-368.12346330812),
 .UNSPECIFIED.);
#887=B_SPLINE_CURVE_WITH_KNOTS('',3,(#40996,#40997,#40998,#40999,#41000,
#41001,#41002,#41003,#41004,#41005,#41006,#41007,#41008,#41009,#41010,#41011,
#41012,#41013,#41014,#41015,#41016,#41017,#41018,#41019,#41020,#41021,#41022,
#41023,#41024,#41025,#41026,#41027,#41028,#41029,#41030,#41031,#41032,#41033,
#41034,#41035),.UNSPECIFIED.,.F.,.F.,(4,3,3,3,3,3,3,3,3,3,3,3,3,4),(364.86780848697,
365.26539781839,365.765076885173,366.264755951956,366.764435018739,367.264114085522,
367.763793152305,368.263472219088,368.763151285871,369.262830352654,369.762509419437,
370.26218848622,370.761867553004,371.150993794149),.UNSPECIFIED.);
#888=B_SPLINE_CURVE_WITH_KNOTS('',3,(#41040,#41041,#41042,#41043,#41044,
#41045,#41046,#41047,#41048,#41049,#41050,#41051,#41052,#41053,#41054,#41055,
#41056,#41057,#41058,#41059,#41060,#41061,#41062,#41063,#41064,#41065,#41066,
#41067,#41068,#41069,#41070,#41071,#41072,#41073,#41074,#41075,#41076,#41077,
#41078,#41079),.UNSPECIFIED.,.F.,.F.,(4,3,3,3,3,3,3,3,3,3,3,3,3,4),(-380.689833922479,
-380.255769821881,-379.756090755098,-379.256411688315,-378.756732621532,
-378.257053554749,-377.757374487966,-377.257695421183,-376.7580163544,-376.258337287616,
-375.758658220834,-375.25897915405,-374.759300087267,-374.406648615299),
 .UNSPECIFIED.);
#889=B_SPLINE_CURVE_WITH_KNOTS('',3,(#41080,#41081,#41082,#41083,#41084,
#41085,#41086,#41087,#41088,#41089,#41090,#41091,#41092,#41093,#41094,#41095,
#41096,#41097,#41098,#41099,#41100,#41101,#41102,#41103,#41104,#41105,#41106,
#41107,#41108,#41109,#41110,#41111,#41112,#41113,#41114,#41115,#41116,#41117,
#41118,#41119,#41120,#41121,#41122),.UNSPECIFIED.,.F.,.F.,(4,3,3,3,3,3,
3,3,3,3,3,3,3,3,4),(371.150993794149,371.261546619787,371.76122568657,372.260904753353,
372.760583820136,373.260262886919,373.759941953702,374.259621020485,374.759300087268,
375.258979154051,375.758658220834,376.258337287617,376.7580163544,377.257695421183,
377.434179101329),.UNSPECIFIED.);
#890=B_SPLINE_CURVE_WITH_KNOTS('',3,(#41127,#41128,#41129,#41130,#41131,
#41132,#41133,#41134,#41135,#41136,#41137,#41138,#41139,#41140,#41141,#41142,
#41143,#41144,#41145,#41146,#41147,#41148,#41149,#41150,#41151,#41152,#41153,
#41154,#41155,#41156,#41157,#41158,#41159,#41160,#41161,#41162,#41163,#41164,
#41165,#41166,#41167,#41168,#41169),.UNSPECIFIED.,.F.,.F.,(4,3,3,3,3,3,
3,3,3,3,3,3,3,3,4),(-386.973019229658,-386.75159769006,-386.251918623277,
-385.752239556494,-385.252560489711,-384.752881422928,-384.253202356145,
-383.753523289362,-383.253844222579,-382.754165155796,-382.254486089013,
-381.75480702223,-381.255127955447,-380.755448888664,-380.689833922479),
 .UNSPECIFIED.);
#891=B_SPLINE_CURVE_WITH_KNOTS('',3,(#41170,#41171,#41172,#41173,#41174,
#41175,#41176,#41177,#41178,#41179,#41180,#41181,#41182,#41183,#41184,#41185,
#41186,#41187,#41188,#41189,#41190,#41191,#41192,#41193,#41194,#41195,#41196,
#41197,#41198,#41199,#41200,#41201,#41202,#41203,#41204,#41205,#41206,#41207,
#41208,#41209),.UNSPECIFIED.,.F.,.F.,(4,3,3,3,3,3,3,3,3,3,3,3,3,4),(377.434179101329,
377.757374487966,378.257053554749,378.756732621532,379.256411688315,379.756090755098,
380.255769821881,380.755448888664,381.255127955447,381.75480702223,382.254486089013,
382.754165155796,383.253844222579,383.717364408508),.UNSPECIFIED.);
#892=B_SPLINE_CURVE_WITH_KNOTS('',3,(#41214,#41215,#41216,#41217,#41218,
#41219,#41220,#41221,#41222,#41223,#41224,#41225,#41226,#41227,#41228,#41229,
#41230,#41231,#41232,#41233,#41234,#41235,#41236,#41237,#41238,#41239,#41240,
#41241,#41242,#41243,#41244,#41245,#41246,#41247,#41248,#41249,#41250,#41251,
#41252,#41253,#41254,#41255,#41256),.UNSPECIFIED.,.F.,.F.,(4,3,3,3,3,3,
3,3,3,3,3,3,3,3,4),(-393.256204536838,-393.247425558239,-392.747746491456,
-392.248067424673,-391.74838835789,-391.248709291107,-390.749030224324,
-390.249351157541,-389.749672090758,-389.249993023975,-388.750313957192,
-388.250634890409,-387.750955823626,-387.251276756843,-386.973019229658),
 .UNSPECIFIED.);
#893=B_SPLINE_CURVE_WITH_KNOTS('',3,(#41257,#41258,#41259,#41260,#41261,
#41262,#41263,#41264,#41265,#41266,#41267,#41268,#41269,#41270,#41271,#41272,
#41273,#41274,#41275,#41276,#41277,#41278,#41279,#41280,#41281,#41282,#41283,
#41284,#41285,#41286,#41287,#41288,#41289,#41290,#41291,#41292,#41293,#41294,
#41295,#41296,#41297,#41298,#41299),.UNSPECIFIED.,.F.,.F.,(4,3,3,3,3,3,
3,3,3,3,3,3,3,3,4),(383.717364408508,383.753523289362,384.253202356145,
384.752881422928,385.252560489711,385.752239556494,386.251918623277,386.75159769006,
387.251276756843,387.750955823626,388.250634890409,388.750313957192,389.249993023975,
389.749672090758,390.000549715688),.UNSPECIFIED.);
#894=B_SPLINE_CURVE_WITH_KNOTS('',3,(#41305,#41306,#41307,#41308),
 .UNSPECIFIED.,.F.,.F.,(4,4),(405.265452313083,405.755527026166),
 .UNSPECIFIED.);
#895=B_SPLINE_CURVE_WITH_KNOTS('',3,(#41314,#41315,#41316,#41317,#41318,
#41319,#41320,#41321,#41322,#41323,#41324,#41325,#41326,#41327,#41328,#41329,
#41330),.UNSPECIFIED.,.F.,.F.,(4,1,1,1,1,1,1,1,1,1,1,1,1,1,4),(398.982267005903,
399.260524533088,399.760203599871,400.259882666654,400.759561733437,401.25924080022,
401.758919867003,402.258598933787,402.75827800057,403.257957067353,403.757636134136,
404.257315200919,404.756994267702,405.256673334485,405.265452313083),
 .UNSPECIFIED.);
#896=B_SPLINE_CURVE_WITH_KNOTS('',3,(#41333,#41334,#41335,#41336,#41337,
#41338,#41339,#41340,#41341,#41342,#41343,#41344,#41345),.UNSPECIFIED.,
 .F.,.F.,(4,1,1,1,1,1,1,1,1,1,4),(398.982267005904,399.231068447758,399.730747514541,
400.230426581324,400.730105648107,401.22978471489,401.729463781673,402.229142848456,
402.728821915239,403.228500982022,403.728180048805),.UNSPECIFIED.);
#897=B_SPLINE_CURVE_WITH_KNOTS('',3,(#41350,#41351,#41352,#41353,#41354,
#41355,#41356,#41357,#41358,#41359,#41360,#41361,#41362,#41363,#41364,#41365,
#41366),.UNSPECIFIED.,.F.,.F.,(4,1,1,1,1,1,1,1,1,1,1,1,1,1,4),(392.699081698724,
392.764696664909,393.264375731692,393.764054798475,394.263733865258,394.763412932041,
395.263091998824,395.762771065607,396.26245013239,396.762129199173,397.261808265956,
397.761487332739,398.261166399522,398.760845466305,398.982267005903),
 .UNSPECIFIED.);
#898=B_SPLINE_CURVE_WITH_KNOTS('',3,(#41367,#41368,#41369,#41370,#41371,
#41372,#41373,#41374,#41375,#41376,#41377,#41378,#41379,#41380,#41381,#41382,
#41383),.UNSPECIFIED.,.F.,.F.,(4,1,1,1,1,1,1,1,1,1,1,1,1,1,4),(392.699081698724,
392.735240579579,393.234919646362,393.734598713145,394.234277779928,394.733956846711,
395.233635913494,395.733314980277,396.23299404706,396.732673113843,397.232352180626,
397.732031247409,398.231710314192,398.731389380975,398.982267005904),
 .UNSPECIFIED.);
#899=B_SPLINE_CURVE_WITH_KNOTS('',3,(#41388,#41389,#41390,#41391,#41392,
#41393,#41394,#41395,#41396,#41397,#41398,#41399,#41400,#41401,#41402,#41403),
 .UNSPECIFIED.,.F.,.F.,(4,1,1,1,1,1,1,1,1,1,1,1,1,4),(386.415896391544,
386.768547863513,387.268226930296,387.767905997079,388.267585063862,388.767264130645,
389.266943197428,389.766622264211,390.266301330994,390.765980397777,391.26565946456,
391.765338531343,392.265017598126,392.699081698724),.UNSPECIFIED.);
#900=B_SPLINE_CURVE_WITH_KNOTS('',3,(#41404,#41405,#41406,#41407,#41408,
#41409,#41410,#41411,#41412,#41413,#41414,#41415,#41416,#41417,#41418,#41419),
 .UNSPECIFIED.,.F.,.F.,(4,1,1,1,1,1,1,1,1,1,1,1,1,4),(386.415896391545,
386.739091778183,387.238770844966,387.738449911749,388.238128978532,388.737808045315,
389.237487112098,389.737166178881,390.236845245664,390.736524312447,391.23620337923,
391.735882446013,392.235561512796,392.699081698724),.UNSPECIFIED.);
#901=B_SPLINE_CURVE_WITH_KNOTS('',3,(#41424,#41425,#41426,#41427,#41428,
#41429,#41430,#41431,#41432,#41433,#41434,#41435,#41436,#41437,#41438,#41439,
#41440),.UNSPECIFIED.,.F.,.F.,(4,1,1,1,1,1,1,1,1,1,1,1,1,1,4),(380.132711084365,
380.272719995333,380.772399062117,381.2720781289,381.771757195683,382.271436262466,
382.771115329249,383.270794396032,383.770473462815,384.270152529598,384.769831596381,
385.269510663164,385.769189729947,386.26886879673,386.415896391544),
 .UNSPECIFIED.);
#902=B_SPLINE_CURVE_WITH_KNOTS('',3,(#41441,#41442,#41443,#41444,#41445,
#41446,#41447,#41448,#41449,#41450,#41451,#41452,#41453,#41454,#41455,#41456,
#41457),.UNSPECIFIED.,.F.,.F.,(4,1,1,1,1,1,1,1,1,1,1,1,1,1,4),(380.132711084365,
380.243263910003,380.742942976786,381.242622043569,381.742301110352,382.241980177135,
382.741659243918,383.241338310702,383.741017377485,384.240696444268,384.740375511051,
385.240054577834,385.739733644617,386.2394127114,386.415896391545),
 .UNSPECIFIED.);
#903=B_SPLINE_CURVE_WITH_KNOTS('',3,(#41462,#41463,#41464,#41465,#41466,
#41467,#41468,#41469,#41470,#41471,#41472,#41473,#41474,#41475,#41476,#41477),
 .UNSPECIFIED.,.F.,.F.,(4,1,1,1,1,1,1,1,1,1,1,1,1,4),(373.849525777185,
374.276571193937,374.77625026072,375.275929327503,375.775608394286,376.275287461069,
376.774966527852,377.274645594635,377.774324661418,378.274003728201,378.773682794984,
379.273361861767,379.77304092855,380.132711084365),.UNSPECIFIED.);
#904=B_SPLINE_CURVE_WITH_KNOTS('',3,(#41478,#41479,#41480,#41481,#41482,
#41483,#41484,#41485,#41486,#41487,#41488,#41489,#41490,#41491,#41492,#41493),
 .UNSPECIFIED.,.F.,.F.,(4,1,1,1,1,1,1,1,1,1,1,1,1,4),(373.849525777185,
374.247115108607,374.74679417539,375.246473242173,375.746152308956,376.245831375739,
376.745510442522,377.245189509305,377.744868576088,378.244547642871,378.744226709654,
379.243905776437,379.74358484322,380.132711084365),.UNSPECIFIED.);
#905=B_SPLINE_CURVE_WITH_KNOTS('',3,(#41498,#41499,#41500,#41501,#41502,
#41503,#41504,#41505,#41506,#41507,#41508,#41509,#41510,#41511,#41512,#41513,
#41514),.UNSPECIFIED.,.F.,.F.,(4,1,1,1,1,1,1,1,1,1,1,1,1,1,4),(367.566340470006,
367.780743325758,368.280422392541,368.780101459324,369.279780526107,369.77945959289,
370.279138659673,370.778817726456,371.278496793239,371.778175860022,372.277854926805,
372.777533993588,373.277213060371,373.776892127154,373.849525777185),
 .UNSPECIFIED.);
#906=B_SPLINE_CURVE_WITH_KNOTS('',3,(#41515,#41516,#41517,#41518,#41519,
#41520,#41521,#41522,#41523,#41524,#41525,#41526,#41527,#41528,#41529,#41530,
#41531),.UNSPECIFIED.,.F.,.F.,(4,1,1,1,1,1,1,1,1,1,1,1,1,1,4),(367.566340470006,
367.751287240428,368.250966307211,368.750645373994,369.250324440777,369.75000350756,
370.249682574343,370.749361641126,371.249040707909,371.748719774692,372.248398841475,
372.748077908258,373.247756975041,373.747436041824,373.849525777185),
 .UNSPECIFIED.);
#907=B_SPLINE_CURVE_WITH_KNOTS('',3,(#41536,#41537,#41538,#41539,#41540,
#41541,#41542,#41543,#41544,#41545,#41546,#41547,#41548,#41549,#41550,#41551,
#41552),.UNSPECIFIED.,.F.,.F.,(4,1,1,1,1,1,1,1,1,1,1,1,1,1,4),(361.283155162826,
361.284915457579,361.784594524362,362.284273591145,362.783952657928,363.283631724711,
363.783310791494,364.282989858277,364.78266892506,365.282347991843,365.782027058626,
366.281706125409,366.781385192192,367.281064258975,367.566340470006),
 .UNSPECIFIED.);
#908=B_SPLINE_CURVE_WITH_KNOTS('',3,(#41553,#41554,#41555,#41556,#41557,
#41558,#41559,#41560,#41561,#41562,#41563,#41564,#41565,#41566,#41567,#41568),
 .UNSPECIFIED.,.F.,.F.,(4,1,1,1,1,1,1,1,1,1,1,1,1,4),(361.283155162826,
361.755138439031,362.254817505815,362.754496572598,363.254175639381,363.753854706164,
364.253533772947,364.75321283973,365.252891906513,365.752570973296,366.252250040079,
366.751929106862,367.251608173645,367.566340470006),.UNSPECIFIED.);
#909=B_SPLINE_CURVE_WITH_KNOTS('',3,(#41573,#41574,#41575,#41576,#41577,
#41578,#41579,#41580,#41581,#41582,#41583,#41584,#41585,#41586),
 .UNSPECIFIED.,.F.,.F.,(4,1,1,1,1,1,1,1,1,1,1,4),(354.999969855646,355.788445722965,
356.787803856531,357.287482923314,357.787161990097,358.28684105688,358.786520123663,
359.286199190446,359.78587825723,360.285557324013,360.785236390796,361.283155162826),
 .UNSPECIFIED.);
#910=B_SPLINE_CURVE_WITH_KNOTS('',3,(#41587,#41588,#41589,#41590,#41591,
#41592,#41593,#41594,#41595,#41596,#41597,#41598,#41599,#41600,#41601,#41602,
#41603),.UNSPECIFIED.,.F.,.F.,(4,1,1,1,1,1,1,1,1,1,1,1,1,1,4),(354.999969855647,
355.259310570852,355.758989637635,356.258668704418,356.758347771201,357.258026837984,
357.757705904767,358.25738497155,358.757064038333,359.256743105116,359.756422171899,
360.256101238682,360.755780305465,361.255459372248,361.283155162826),
 .UNSPECIFIED.);
#911=B_SPLINE_CURVE_WITH_KNOTS('',3,(#41608,#41609,#41610,#41611,#41612,
#41613,#41614,#41615,#41616,#41617,#41618),.UNSPECIFIED.,.F.,.F.,(4,1,1,
1,1,1,1,1,4),(348.716784548467,348.792938788003,349.792296921569,350.791655055135,
351.791013188701,352.790371322267,353.789729455833,354.789087589399,354.999969855646),
 .UNSPECIFIED.);
#912=B_SPLINE_CURVE_WITH_KNOTS('',3,(#41619,#41620,#41621,#41622,#41623,
#41624,#41625,#41626,#41627,#41628,#41629,#41630),.UNSPECIFIED.,.F.,.F.,
(4,1,1,1,1,1,1,1,1,4),(348.716784548467,348.763482702673,349.762840836239,
350.762198969805,351.761557103371,352.760915236937,353.760273370503,354.259952437286,
354.759631504069,354.999969855647),.UNSPECIFIED.);
#913=B_SPLINE_CURVE_WITH_KNOTS('',3,(#41635,#41636,#41637,#41638,#41639,
#41640,#41641,#41642,#41643,#41644),.UNSPECIFIED.,.F.,.F.,(4,1,1,1,1,1,
1,4),(342.433599241287,342.796789986607,343.796148120173,344.795506253739,
345.794864387305,346.794222520871,347.793580654437,348.716784548467),
 .UNSPECIFIED.);
#914=B_SPLINE_CURVE_WITH_KNOTS('',3,(#41645,#41646,#41647,#41648,#41649,
#41650,#41651,#41652,#41653,#41654),.UNSPECIFIED.,.F.,.F.,(4,1,1,1,1,1,
1,4),(342.433599241288,342.767333901277,343.766692034843,344.766050168409,
345.765408301975,346.764766435541,347.764124569107,348.716784548467),
 .UNSPECIFIED.);
#915=B_SPLINE_CURVE_WITH_KNOTS('',3,(#41659,#41660,#41661,#41662,#41663,
#41664,#41665,#41666,#41667,#41668),.UNSPECIFIED.,.F.,.F.,(4,1,1,1,1,1,
1,4),(336.150413934108,336.80064118521,337.799999318776,338.799357452343,
339.798715585909,340.798073719475,341.797431853041,342.433599241287),
 .UNSPECIFIED.);
#916=B_SPLINE_CURVE_WITH_KNOTS('',3,(#41669,#41670,#41671,#41672,#41673,
#41674,#41675,#41676,#41677,#41678),.UNSPECIFIED.,.F.,.F.,(4,1,1,1,1,1,
1,4),(336.150413934108,336.77118509988,337.770543233446,338.769901367012,
339.769259500578,340.768617634145,341.767975767711,342.433599241288),
 .UNSPECIFIED.);
#917=B_SPLINE_CURVE_WITH_KNOTS('',3,(#41683,#41684,#41685,#41686,#41687,
#41688,#41689,#41690,#41691,#41692),.UNSPECIFIED.,.F.,.F.,(4,1,1,1,1,1,
1,4),(329.867228626928,330.804492383814,331.80385051738,332.803208650946,
333.802566784512,334.801924918078,335.801283051644,336.150413934108),
 .UNSPECIFIED.);
#918=B_SPLINE_CURVE_WITH_KNOTS('',3,(#41693,#41694,#41695,#41696,#41697,
#41698,#41699,#41700,#41701,#41702),.UNSPECIFIED.,.F.,.F.,(4,1,1,1,1,1,
1,4),(329.867228626928,330.775036298484,331.77439443205,332.773752565616,
333.773110699182,334.772468832748,335.771826966314,336.150413934108),
 .UNSPECIFIED.);
#919=B_SPLINE_CURVE_WITH_KNOTS('',3,(#41707,#41708,#41709,#41710,#41711,
#41712,#41713,#41714,#41715,#41716,#41717),.UNSPECIFIED.,.F.,.F.,(4,1,1,
1,1,1,1,1,4),(323.584043319749,323.808985448852,324.808343582418,325.807701715984,
326.80705984955,327.806417983116,328.805776116682,329.805134250248,329.867228626928),
 .UNSPECIFIED.);
#920=B_SPLINE_CURVE_WITH_KNOTS('',3,(#41718,#41719,#41720,#41721,#41722,
#41723,#41724,#41725,#41726,#41727,#41728),.UNSPECIFIED.,.F.,.F.,(4,1,1,
1,1,1,1,1,4),(323.584043319749,323.779529363522,324.778887497088,325.778245630654,
326.77760376422,327.776961897786,328.776320031352,329.775678164918,329.867228626928),
 .UNSPECIFIED.);
#921=B_SPLINE_CURVE_WITH_KNOTS('',3,(#41733,#41734,#41735,#41736,#41737,
#41738,#41739,#41740,#41741,#41742),.UNSPECIFIED.,.F.,.F.,(4,1,1,1,1,1,
1,4),(317.300858012569,317.812836647456,318.812194781022,319.811552914588,
320.810911048154,321.81026918172,322.809627315286,323.584043319749),
 .UNSPECIFIED.);
#922=B_SPLINE_CURVE_WITH_KNOTS('',3,(#41743,#41744,#41745,#41746,#41747,
#41748,#41749,#41750,#41751,#41752),.UNSPECIFIED.,.F.,.F.,(4,1,1,1,1,1,
1,4),(317.300858012569,317.783380562125,318.782738695691,319.782096829258,
320.781454962824,321.78081309639,322.780171229956,323.584043319749),
 .UNSPECIFIED.);
#923=B_SPLINE_CURVE_WITH_KNOTS('',3,(#41757,#41758,#41759,#41760,#41761,
#41762,#41763,#41764,#41765,#41766),.UNSPECIFIED.,.F.,.F.,(4,1,1,1,1,1,
1,4),(311.017672705389,311.816687846059,312.816045979625,313.815404113191,
314.814762246757,315.814120380323,316.81347851389,317.300858012569),
 .UNSPECIFIED.);
#924=B_SPLINE_CURVE_WITH_KNOTS('',3,(#41767,#41768,#41769,#41770,#41771,
#41772,#41773,#41774,#41775,#41776),.UNSPECIFIED.,.F.,.F.,(4,1,1,1,1,1,
1,4),(311.01767270539,311.787231760729,312.786589894295,313.785948027861,
314.785306161427,315.784664294993,316.784022428559,317.300858012569),
 .UNSPECIFIED.);
#925=B_SPLINE_CURVE_WITH_KNOTS('',3,(#41781,#41782,#41783,#41784,#41785,
#41786,#41787,#41788,#41789,#41790,#41791),.UNSPECIFIED.,.F.,.F.,(4,1,1,
1,1,1,1,1,4),(304.73448739821,304.821180911097,305.820539044663,306.819897178229,
307.819255311795,308.818613445361,309.817971578927,310.817329712493,311.017672705389),
 .UNSPECIFIED.);
#926=B_SPLINE_CURVE_WITH_KNOTS('',3,(#41792,#41793,#41794,#41795,#41796,
#41797,#41798,#41799,#41800,#41801,#41802),.UNSPECIFIED.,.F.,.F.,(4,1,1,
1,1,1,1,1,4),(304.73448739821,304.791724825767,305.791082959333,306.790441092899,
307.789799226465,308.789157360031,309.788515493597,310.787873627163,311.01767270539),
 .UNSPECIFIED.);
#927=B_SPLINE_CURVE_WITH_KNOTS('',3,(#41807,#41808,#41809,#41810,#41811,
#41812,#41813,#41814,#41815,#41816),.UNSPECIFIED.,.F.,.F.,(4,1,1,1,1,1,
1,4),(298.45130209103,298.825032109701,299.824390243267,300.823748376833,
301.823106510399,302.822464643965,303.821822777531,304.73448739821),
 .UNSPECIFIED.);
#928=B_SPLINE_CURVE_WITH_KNOTS('',3,(#41817,#41818,#41819,#41820,#41821,
#41822,#41823,#41824,#41825,#41826),.UNSPECIFIED.,.F.,.F.,(4,1,1,1,1,1,
1,4),(298.451302091031,298.795576024371,299.794934157937,300.794292291503,
301.793650425069,302.793008558635,303.792366692201,304.73448739821),
 .UNSPECIFIED.);
#929=B_SPLINE_CURVE_WITH_KNOTS('',3,(#41831,#41832,#41833,#41834,#41835,
#41836,#41837,#41838,#41839,#41840),.UNSPECIFIED.,.F.,.F.,(4,1,1,1,1,1,
1,4),(292.168116783851,292.828883308304,293.82824144187,294.827599575437,
295.826957709003,296.826315842569,297.825673976135,298.45130209103),
 .UNSPECIFIED.);
#930=B_SPLINE_CURVE_WITH_KNOTS('',3,(#41841,#41842,#41843,#41844,#41845,
#41846,#41847,#41848,#41849,#41850),.UNSPECIFIED.,.F.,.F.,(4,1,1,1,1,1,
1,4),(292.168116783851,292.799427222974,293.79878535654,294.798143490106,
295.797501623672,296.796859757238,297.796217890804,298.451302091031),
 .UNSPECIFIED.);
#931=B_SPLINE_CURVE_WITH_KNOTS('',3,(#41855,#41856,#41857,#41858,#41859,
#41860,#41861,#41862,#41863,#41864),.UNSPECIFIED.,.F.,.F.,(4,1,1,1,1,1,
1,4),(285.884931476671,286.832734506908,287.832092640474,288.83145077404,
289.830808907606,290.830167041172,291.829525174738,292.168116783851),
 .UNSPECIFIED.);
#932=B_SPLINE_CURVE_WITH_KNOTS('',3,(#41865,#41866,#41867,#41868,#41869,
#41870,#41871,#41872,#41873,#41874),.UNSPECIFIED.,.F.,.F.,(4,1,1,1,1,1,
1,4),(285.884931476672,286.803278421578,287.802636555144,288.80199468871,
289.801352822276,290.800710955842,291.800069089408,292.168116783851),
 .UNSPECIFIED.);
#933=B_SPLINE_CURVE_WITH_KNOTS('',3,(#41879,#41880,#41881,#41882,#41883,
#41884,#41885,#41886,#41887,#41888,#41889),.UNSPECIFIED.,.F.,.F.,(4,1,1,
1,1,1,1,1,4),(279.601746169492,279.837227571946,280.836585705512,281.835943839078,
282.835301972644,283.83466010621,284.834018239776,285.833376373342,285.884931476671),
 .UNSPECIFIED.);
#934=B_SPLINE_CURVE_WITH_KNOTS('',3,(#41890,#41891,#41892,#41893,#41894,
#41895,#41896,#41897,#41898,#41899,#41900),.UNSPECIFIED.,.F.,.F.,(4,1,1,
1,1,1,1,1,4),(279.601746169492,279.807771486616,280.807129620182,281.806487753748,
282.805845887314,283.80520402088,284.804562154446,285.803920288012,285.884931476672),
 .UNSPECIFIED.);
#935=B_SPLINE_CURVE_WITH_KNOTS('',3,(#41905,#41906,#41907,#41908,#41909,
#41910,#41911,#41912,#41913,#41914),.UNSPECIFIED.,.F.,.F.,(4,1,1,1,1,1,
1,4),(273.318560862312,273.84107877055,274.840436904116,275.839795037682,
276.839153171248,277.838511304814,278.83786943838,279.601746169492),
 .UNSPECIFIED.);
#936=B_SPLINE_CURVE_WITH_KNOTS('',3,(#41915,#41916,#41917,#41918,#41919,
#41920,#41921,#41922,#41923,#41924),.UNSPECIFIED.,.F.,.F.,(4,1,1,1,1,1,
1,4),(273.318560862312,273.811622685219,274.810980818785,275.810338952351,
276.809697085917,277.809055219484,278.80841335305,279.601746169492),
 .UNSPECIFIED.);
#937=B_SPLINE_CURVE_WITH_KNOTS('',3,(#41929,#41930,#41931,#41932,#41933,
#41934,#41935,#41936,#41937,#41938),.UNSPECIFIED.,.F.,.F.,(4,1,1,1,1,1,
1,4),(267.035375555133,267.844929969153,268.844288102719,269.843646236285,
270.843004369851,271.842362503417,272.841720636983,273.318560862312),
 .UNSPECIFIED.);
#938=B_SPLINE_CURVE_WITH_KNOTS('',3,(#41939,#41940,#41941,#41942,#41943,
#41944,#41945,#41946,#41947,#41948),.UNSPECIFIED.,.F.,.F.,(4,1,1,1,1,1,
1,4),(267.035375555133,267.815473883823,268.814832017389,269.814190150955,
270.813548284521,271.812906418087,272.812264551653,273.318560862312),
 .UNSPECIFIED.);
#939=B_SPLINE_CURVE_WITH_KNOTS('',3,(#41953,#41954,#41955,#41956,#41957,
#41958,#41959,#41960,#41961,#41962,#41963),.UNSPECIFIED.,.F.,.F.,(4,1,1,
1,1,1,1,1,4),(260.752190247953,260.849423034191,261.848781167757,262.848139301323,
263.847497434889,264.846855568455,265.846213702021,266.845571835587,267.035375555133),
 .UNSPECIFIED.);
#940=B_SPLINE_CURVE_WITH_KNOTS('',3,(#41964,#41965,#41966,#41967,#41968,
#41969,#41970,#41971,#41972,#41973,#41974),.UNSPECIFIED.,.F.,.F.,(4,1,1,
1,1,1,1,1,4),(260.752190247953,260.819966948861,261.819325082427,262.818683215993,
263.818041349559,264.817399483125,265.816757616691,266.816115750257,267.035375555133),
 .UNSPECIFIED.);
#941=B_SPLINE_CURVE_WITH_KNOTS('',3,(#41979,#41980,#41981,#41982,#41983,
#41984,#41985,#41986,#41987,#41988),.UNSPECIFIED.,.F.,.F.,(4,1,1,1,1,1,
1,4),(254.469004940773,254.853274232795,255.852632366361,256.851990499927,
257.851348633493,258.850706767059,259.850064900625,260.752190247953),
 .UNSPECIFIED.);
#942=B_SPLINE_CURVE_WITH_KNOTS('',3,(#41989,#41990,#41991,#41992,#41993,
#41994,#41995,#41996,#41997,#41998),.UNSPECIFIED.,.F.,.F.,(4,1,1,1,1,1,
1,4),(254.469004940774,254.823818147464,255.82317628103,256.822534414597,
257.821892548163,258.821250681729,259.820608815295,260.752190247953),
 .UNSPECIFIED.);
#943=B_SPLINE_CURVE_WITH_KNOTS('',3,(#42003,#42004,#42005,#42006,#42007,
#42008,#42009,#42010,#42011,#42012),.UNSPECIFIED.,.F.,.F.,(4,1,1,1,1,1,
1,4),(248.185819633594,248.857125431398,249.856483564964,250.85584169853,
251.855199832097,252.854557965663,253.853916099229,254.469004940773),
 .UNSPECIFIED.);
#944=B_SPLINE_CURVE_WITH_KNOTS('',3,(#42013,#42014,#42015,#42016,#42017,
#42018,#42019,#42020,#42021,#42022),.UNSPECIFIED.,.F.,.F.,(4,1,1,1,1,1,
1,4),(248.185819633594,248.827669346068,249.827027479634,250.8263856132,
251.825743746766,252.825101880332,253.824460013898,254.469004940774),
 .UNSPECIFIED.);
#945=B_SPLINE_CURVE_WITH_KNOTS('',3,(#42027,#42028,#42029,#42030,#42031,
#42032,#42033,#42034,#42035,#42036),.UNSPECIFIED.,.F.,.F.,(4,1,1,1,1,1,
1,4),(241.902634326414,242.860976630002,243.860334763568,244.859692897134,
245.8590510307,246.858409164266,247.857767297832,248.185819633594),
 .UNSPECIFIED.);
#946=B_SPLINE_CURVE_WITH_KNOTS('',3,(#42037,#42038,#42039,#42040,#42041,
#42042,#42043,#42044,#42045,#42046),.UNSPECIFIED.,.F.,.F.,(4,1,1,1,1,1,
1,4),(241.902634326415,242.831520544672,243.830878678238,244.830236811804,
245.82959494537,246.828953078936,247.828311212502,248.185819633594),
 .UNSPECIFIED.);
#947=B_SPLINE_CURVE_WITH_KNOTS('',3,(#42051,#42052,#42053,#42054,#42055,
#42056,#42057,#42058,#42059,#42060,#42061),.UNSPECIFIED.,.F.,.F.,(4,1,1,
1,1,1,1,1,4),(235.619449019235,235.86546969504,236.864827828606,237.864185962172,
238.863544095738,239.862902229304,240.86226036287,241.861618496436,241.902634326414),
 .UNSPECIFIED.);
#948=B_SPLINE_CURVE_WITH_KNOTS('',3,(#42062,#42063,#42064,#42065,#42066,
#42067,#42068,#42069,#42070,#42071,#42072),.UNSPECIFIED.,.F.,.F.,(4,1,1,
1,1,1,1,1,4),(235.619449019235,235.83601360971,236.835371743276,237.834729876842,
238.834088010408,239.833446143974,240.83280427754,241.832162411106,241.902634326415),
 .UNSPECIFIED.);
#949=B_SPLINE_CURVE_WITH_KNOTS('',3,(#42077,#42078,#42079,#42080,#42081,
#42082,#42083,#42084,#42085,#42086),.UNSPECIFIED.,.F.,.F.,(4,1,1,1,1,1,
1,4),(229.336263712055,229.869320893643,230.86867902721,231.868037160776,
232.867395294342,233.866753427908,234.866111561474,235.619449019235),
 .UNSPECIFIED.);
#950=B_SPLINE_CURVE_WITH_KNOTS('',3,(#42087,#42088,#42089,#42090,#42091,
#42092,#42093,#42094,#42095,#42096),.UNSPECIFIED.,.F.,.F.,(4,1,1,1,1,1,
1,4),(229.336263712055,229.839864808313,230.839222941879,231.838581075445,
232.837939209011,233.837297342577,234.836655476144,235.619449019235),
 .UNSPECIFIED.);
#951=B_SPLINE_CURVE_WITH_KNOTS('',3,(#42101,#42102,#42103,#42104,#42105,
#42106,#42107,#42108,#42109,#42110),.UNSPECIFIED.,.F.,.F.,(4,1,1,1,1,1,
1,4),(223.053078404876,223.873172092247,224.872530225813,225.871888359379,
226.871246492945,227.870604626511,228.869962760077,229.336263712055),
 .UNSPECIFIED.);
#952=B_SPLINE_CURVE_WITH_KNOTS('',3,(#42111,#42112,#42113,#42114,#42115,
#42116,#42117,#42118,#42119,#42120),.UNSPECIFIED.,.F.,.F.,(4,1,1,1,1,1,
1,4),(223.053078404876,223.843716006917,224.843074140483,225.842432274049,
226.841790407615,227.841148541181,228.840506674747,229.336263712055),
 .UNSPECIFIED.);
#953=B_SPLINE_CURVE_WITH_KNOTS('',3,(#42125,#42126,#42127,#42128,#42129,
#42130,#42131,#42132,#42133,#42134,#42135),.UNSPECIFIED.,.F.,.F.,(4,1,1,
1,1,1,1,1,4),(216.769893097696,216.877665157285,217.877023290851,218.876381424417,
219.875739557983,220.875097691549,221.874455825115,222.873813958681,223.053078404876),
 .UNSPECIFIED.);
#954=B_SPLINE_CURVE_WITH_KNOTS('',3,(#42136,#42137,#42138,#42139,#42140,
#42141,#42142,#42143,#42144,#42145,#42146),.UNSPECIFIED.,.F.,.F.,(4,1,1,
1,1,1,1,1,4),(216.769893097696,216.848209071955,217.847567205521,218.846925339087,
219.846283472653,220.845641606219,221.844999739785,222.844357873351,223.053078404876),
 .UNSPECIFIED.);
#955=B_SPLINE_CURVE_WITH_KNOTS('',3,(#42151,#42152,#42153,#42154,#42155,
#42156,#42157,#42158,#42159,#42160),.UNSPECIFIED.,.F.,.F.,(4,1,1,1,1,1,
1,4),(210.486707790516,210.881516355889,211.880874489455,212.880232623021,
213.879590756587,214.878948890153,215.878307023719,216.769893097696),
 .UNSPECIFIED.);
#956=B_SPLINE_CURVE_WITH_KNOTS('',3,(#42161,#42162,#42163,#42164,#42165,
#42166,#42167,#42168,#42169,#42170),.UNSPECIFIED.,.F.,.F.,(4,1,1,1,1,1,
1,4),(210.486707790517,210.852060270558,211.851418404124,212.85077653769,
213.850134671257,214.849492804823,215.848850938389,216.769893097696),
 .UNSPECIFIED.);
#957=B_SPLINE_CURVE_WITH_KNOTS('',3,(#42175,#42176,#42177,#42178,#42179,
#42180,#42181,#42182,#42183,#42184),.UNSPECIFIED.,.F.,.F.,(4,1,1,1,1,1,
1,4),(204.203522483337,204.885367554492,205.884725688058,206.884083821624,
207.88344195519,208.882800088756,209.882158222323,210.486707790516),
 .UNSPECIFIED.);
#958=B_SPLINE_CURVE_WITH_KNOTS('',3,(#42185,#42186,#42187,#42188,#42189,
#42190,#42191,#42192,#42193,#42194),.UNSPECIFIED.,.F.,.F.,(4,1,1,1,1,1,
1,4),(204.203522483337,204.855911469162,205.855269602728,206.854627736294,
207.85398586986,208.853344003426,209.852702136992,210.486707790517),
 .UNSPECIFIED.);
#959=B_SPLINE_CURVE_WITH_KNOTS('',3,(#42199,#42200,#42201,#42202,#42203,
#42204,#42205,#42206,#42207,#42208),.UNSPECIFIED.,.F.,.F.,(4,1,1,1,1,1,
1,4),(197.920337176157,198.889218753096,199.888576886662,200.887935020228,
201.887293153794,202.88665128736,203.886009420926,204.203522483337),
 .UNSPECIFIED.);
#960=B_SPLINE_CURVE_WITH_KNOTS('',3,(#42209,#42210,#42211,#42212,#42213,
#42214,#42215,#42216,#42217,#42218),.UNSPECIFIED.,.F.,.F.,(4,1,1,1,1,1,
1,4),(197.920337176158,198.859762667766,199.859120801332,200.858478934898,
201.857837068464,202.85719520203,203.856553335596,204.203522483337),
 .UNSPECIFIED.);
#961=B_SPLINE_CURVE_WITH_KNOTS('',3,(#42223,#42224,#42225,#42226,#42227,
#42228,#42229,#42230,#42231,#42232,#42233),.UNSPECIFIED.,.F.,.F.,(4,1,1,
1,1,1,1,1,4),(191.637151868978,191.893711818134,192.8930699517,193.892428085266,
194.891786218832,195.891144352398,196.890502485964,197.88986061953,197.920337176157),
 .UNSPECIFIED.);
#962=B_SPLINE_CURVE_WITH_KNOTS('',3,(#42234,#42235,#42236,#42237,#42238,
#42239,#42240,#42241,#42242,#42243,#42244),.UNSPECIFIED.,.F.,.F.,(4,1,1,
1,1,1,1,1,4),(191.637151868978,191.864255732803,192.86361386637,193.862971999936,
194.862330133502,195.861688267068,196.861046400634,197.8604045342,197.920337176158),
 .UNSPECIFIED.);
#963=B_SPLINE_CURVE_WITH_KNOTS('',3,(#42249,#42250,#42251,#42252,#42253,
#42254,#42255,#42256,#42257,#42258),.UNSPECIFIED.,.F.,.F.,(4,1,1,1,1,1,
1,4),(185.353966561798,185.897563016737,186.896921150303,187.89627928387,
188.895637417436,189.894995551002,190.894353684568,191.637151868978),
 .UNSPECIFIED.);
#964=B_SPLINE_CURVE_WITH_KNOTS('',3,(#42259,#42260,#42261,#42262,#42263,
#42264,#42265,#42266,#42267,#42268),.UNSPECIFIED.,.F.,.F.,(4,1,1,1,1,1,
1,4),(185.353966561799,185.868106931407,186.867465064973,187.866823198539,
188.866181332105,189.865539465671,190.864897599237,191.637151868978),
 .UNSPECIFIED.);
#965=B_SPLINE_CURVE_WITH_KNOTS('',3,(#42273,#42274,#42275,#42276,#42277,
#42278,#42279,#42280,#42281,#42282),.UNSPECIFIED.,.F.,.F.,(4,1,1,1,1,1,
1,4),(179.070781254619,179.901414215341,180.900772348907,181.900130482473,
182.899488616039,183.898846749605,184.898204883171,185.353966561798),
 .UNSPECIFIED.);
#966=B_SPLINE_CURVE_WITH_KNOTS('',3,(#42283,#42284,#42285,#42286,#42287,
#42288,#42289,#42290,#42291,#42292),.UNSPECIFIED.,.F.,.F.,(4,1,1,1,1,1,
1,4),(179.070781254619,179.871958130011,180.871316263577,181.870674397143,
182.870032530709,183.869390664275,184.868748797841,185.353966561799),
 .UNSPECIFIED.);
#967=B_SPLINE_CURVE_WITH_KNOTS('',3,(#42297,#42298,#42299,#42300,#42301,
#42302,#42303,#42304,#42305,#42306,#42307),.UNSPECIFIED.,.F.,.F.,(4,1,1,
1,1,1,1,1,4),(172.787595947439,172.905907280379,173.905265413945,174.904623547511,
175.903981681077,176.903339814643,177.902697948209,178.902056081775,179.070781254619),
 .UNSPECIFIED.);
#968=B_SPLINE_CURVE_WITH_KNOTS('',3,(#42308,#42309,#42310,#42311,#42312,
#42313,#42314,#42315,#42316,#42317,#42318),.UNSPECIFIED.,.F.,.F.,(4,1,1,
1,1,1,1,1,4),(172.787595947439,172.876451195049,173.875809328615,174.875167462181,
175.874525595747,176.873883729313,177.873241862879,178.872599996445,179.070781254619),
 .UNSPECIFIED.);
#969=B_SPLINE_CURVE_WITH_KNOTS('',3,(#42323,#42324,#42325,#42326,#42327,
#42328,#42329,#42330,#42331,#42332),.UNSPECIFIED.,.F.,.F.,(4,1,1,1,1,1,
1,4),(166.504410640259,166.909758478983,167.909116612549,168.908474746115,
169.907832879681,170.907191013247,171.906549146813,172.787595947439),
 .UNSPECIFIED.);
#970=B_SPLINE_CURVE_WITH_KNOTS('',3,(#42333,#42334,#42335,#42336,#42337,
#42338,#42339,#42340,#42341,#42342),.UNSPECIFIED.,.F.,.F.,(4,1,1,1,1,1,
1,4),(166.50441064026,166.880302393652,167.879660527218,168.879018660784,
169.87837679435,170.877734927916,171.877093061483,172.787595947439),
 .UNSPECIFIED.);
#971=B_SPLINE_CURVE_WITH_KNOTS('',3,(#42347,#42348,#42349,#42350,#42351,
#42352,#42353,#42354,#42355,#42356),.UNSPECIFIED.,.F.,.F.,(4,1,1,1,1,1,
1,4),(160.22122533308,160.913609677586,161.912967811152,162.912325944718,
163.911684078284,164.91104221185,165.910400345416,166.504410640259),
 .UNSPECIFIED.);
#972=B_SPLINE_CURVE_WITH_KNOTS('',3,(#42357,#42358,#42359,#42360,#42361,
#42362,#42363,#42364,#42365,#42366),.UNSPECIFIED.,.F.,.F.,(4,1,1,1,1,1,
1,4),(160.22122533308,160.884153592256,161.883511725822,162.882869859388,
163.882227992954,164.88158612652,165.880944260086,166.50441064026),
 .UNSPECIFIED.);
#973=B_SPLINE_CURVE_WITH_KNOTS('',3,(#42371,#42372,#42373,#42374,#42375,
#42376,#42377,#42378,#42379,#42380),.UNSPECIFIED.,.F.,.F.,(4,1,1,1,1,1,
1,4),(153.9380400259,154.91746087619,155.916819009756,156.916177143322,
157.915535276888,158.914893410454,159.91425154402,160.22122533308),
 .UNSPECIFIED.);
#974=B_SPLINE_CURVE_WITH_KNOTS('',3,(#42381,#42382,#42383,#42384,#42385,
#42386,#42387,#42388,#42389,#42390),.UNSPECIFIED.,.F.,.F.,(4,1,1,1,1,1,
1,4),(153.938040025901,154.88800479086,155.887362924426,156.886721057992,
157.886079191558,158.885437325124,159.88479545869,160.22122533308),
 .UNSPECIFIED.);
#975=B_SPLINE_CURVE_WITH_KNOTS('',3,(#42395,#42396,#42397,#42398,#42399,
#42400,#42401,#42402,#42403,#42404,#42405),.UNSPECIFIED.,.F.,.F.,(4,1,1,
1,1,1,1,1,4),(147.654854718721,147.921953941228,148.921312074794,149.92067020836,
150.920028341926,151.919386475492,152.918744609058,153.918102742624,153.9380400259),
 .UNSPECIFIED.);
#976=B_SPLINE_CURVE_WITH_KNOTS('',3,(#42406,#42407,#42408,#42409,#42410,
#42411,#42412,#42413,#42414,#42415,#42416),.UNSPECIFIED.,.F.,.F.,(4,1,1,
1,1,1,1,1,4),(147.654854718721,147.892497855897,148.891855989463,149.891214123029,
150.890572256596,151.889930390162,152.889288523728,153.888646657294,153.938040025901),
 .UNSPECIFIED.);
#977=B_SPLINE_CURVE_WITH_KNOTS('',3,(#42421,#42422,#42423,#42424,#42425,
#42426,#42427,#42428,#42429,#42430),.UNSPECIFIED.,.F.,.F.,(4,1,1,1,1,1,
1,4),(141.371669411541,141.925805139831,142.925163273397,143.924521406963,
144.92387954053,145.923237674096,146.922595807662,147.654854718721),
 .UNSPECIFIED.);
#978=B_SPLINE_CURVE_WITH_KNOTS('',3,(#42431,#42432,#42433,#42434,#42435,
#42436,#42437,#42438,#42439,#42440),.UNSPECIFIED.,.F.,.F.,(4,1,1,1,1,1,
1,4),(141.371669411542,141.896349054501,142.895707188067,143.895065321633,
144.894423455199,145.893781588765,146.893139722331,147.654854718721),
 .UNSPECIFIED.);
#979=B_SPLINE_CURVE_WITH_KNOTS('',3,(#42445,#42446,#42447,#42448,#42449,
#42450,#42451,#42452,#42453,#42454),.UNSPECIFIED.,.F.,.F.,(4,1,1,1,1,1,
1,4),(135.088484104362,135.929656338435,136.929014472001,137.928372605567,
138.927730739133,139.927088872699,140.926447006265,141.371669411541),
 .UNSPECIFIED.);
#980=B_SPLINE_CURVE_WITH_KNOTS('',3,(#42455,#42456,#42457,#42458,#42459,
#42460,#42461,#42462,#42463,#42464),.UNSPECIFIED.,.F.,.F.,(4,1,1,1,1,1,
1,4),(135.088484104362,135.900200253105,136.899558386671,137.898916520237,
138.898274653803,139.897632787369,140.896990920935,141.371669411542),
 .UNSPECIFIED.);
#981=B_SPLINE_CURVE_WITH_KNOTS('',3,(#42469,#42470,#42471,#42472,#42473,
#42474,#42475,#42476,#42477,#42478,#42479),.UNSPECIFIED.,.F.,.F.,(4,1,1,
1,1,1,1,1,4),(128.805298797182,128.934149403473,129.933507537039,130.932865670605,
131.932223804171,132.931581937737,133.930940071303,134.930298204869,135.088484104362),
 .UNSPECIFIED.);
#982=B_SPLINE_CURVE_WITH_KNOTS('',3,(#42480,#42481,#42482,#42483,#42484,
#42485,#42486,#42487,#42488,#42489,#42490),.UNSPECIFIED.,.F.,.F.,(4,1,1,
1,1,1,1,1,4),(128.805298797182,128.904693318142,129.904051451709,130.903409585275,
131.902767718841,132.902125852407,133.901483985973,134.900842119539,135.088484104362),
 .UNSPECIFIED.);
#983=B_SPLINE_CURVE_WITH_KNOTS('',3,(#42495,#42496,#42497,#42498,#42499,
#42500,#42501,#42502,#42503,#42504),.UNSPECIFIED.,.F.,.F.,(4,1,1,1,1,1,
1,4),(122.522113490002,122.938000602077,123.937358735643,124.936716869209,
125.936075002775,126.935433136341,127.934791269907,128.805298797182),
 .UNSPECIFIED.);
#984=B_SPLINE_CURVE_WITH_KNOTS('',3,(#42505,#42506,#42507,#42508,#42509,
#42510,#42511,#42512,#42513,#42514),.UNSPECIFIED.,.F.,.F.,(4,1,1,1,1,1,
1,4),(122.522113490003,122.908544516746,123.907902650312,124.907260783878,
125.906618917444,126.90597705101,127.905335184576,128.805298797182),
 .UNSPECIFIED.);
#985=B_SPLINE_CURVE_WITH_KNOTS('',3,(#42519,#42520,#42521,#42522,#42523,
#42524,#42525,#42526,#42527,#42528),.UNSPECIFIED.,.F.,.F.,(4,1,1,1,1,1,
1,4),(116.238928182823,116.94185180068,117.941209934246,118.940568067812,
119.939926201378,120.939284334944,121.93864246851,122.522113490002),
 .UNSPECIFIED.);
#986=B_SPLINE_CURVE_WITH_KNOTS('',3,(#42529,#42530,#42531,#42532,#42533,
#42534,#42535,#42536,#42537,#42538),.UNSPECIFIED.,.F.,.F.,(4,1,1,1,1,1,
1,4),(116.238928182823,116.91239571535,117.911753848916,118.911111982482,
119.910470116048,120.909828249614,121.90918638318,122.522113490003),
 .UNSPECIFIED.);
#987=B_SPLINE_CURVE_WITH_KNOTS('',3,(#42543,#42544,#42545,#42546,#42547,
#42548,#42549,#42550,#42551,#42552),.UNSPECIFIED.,.F.,.F.,(4,1,1,1,1,1,
1,4),(109.955742875643,110.945702999284,111.94506113285,112.944419266416,
113.943777399982,114.943135533548,115.942493667114,116.238928182823),
 .UNSPECIFIED.);
#988=B_SPLINE_CURVE_WITH_KNOTS('',3,(#42553,#42554,#42555,#42556,#42557,
#42558,#42559,#42560,#42561,#42562),.UNSPECIFIED.,.F.,.F.,(4,1,1,1,1,1,
1,4),(109.955742875644,110.916246913954,111.91560504752,112.914963181086,
113.914321314652,114.913679448218,115.913037581784,116.238928182823),
 .UNSPECIFIED.);
#989=B_SPLINE_CURVE_WITH_KNOTS('',3,(#42567,#42568,#42569,#42570,#42571,
#42572,#42573,#42574,#42575,#42576,#42577),.UNSPECIFIED.,.F.,.F.,(4,1,1,
1,1,1,1,1,4),(103.672557568464,103.950196064322,104.949554197888,105.948912331454,
106.94827046502,107.947628598586,108.946986732152,109.946344865718,109.955742875643),
 .UNSPECIFIED.);
#990=B_SPLINE_CURVE_WITH_KNOTS('',3,(#42578,#42579,#42580,#42581,#42582,
#42583,#42584,#42585,#42586,#42587,#42588),.UNSPECIFIED.,.F.,.F.,(4,1,1,
1,1,1,1,1,4),(103.672557568464,103.920739978991,104.920098112557,105.919456246123,
106.918814379689,107.918172513255,108.917530646822,109.916888780388,109.955742875644),
 .UNSPECIFIED.);
#991=B_SPLINE_CURVE_WITH_KNOTS('',3,(#42593,#42594,#42595,#42596,#42597,
#42598,#42599,#42600,#42601,#42602),.UNSPECIFIED.,.F.,.F.,(4,1,1,1,1,1,
1,4),(97.3893722612841,97.9540472629253,98.9534053964914,99.9527635300574,
100.952121663623,101.95147979719,102.950837930756,103.672557568464),
 .UNSPECIFIED.);
#992=B_SPLINE_CURVE_WITH_KNOTS('',3,(#42603,#42604,#42605,#42606,#42607,
#42608,#42609,#42610,#42611,#42612),.UNSPECIFIED.,.F.,.F.,(4,1,1,1,1,1,
1,4),(97.3893722612845,97.924591177595,98.9239493111611,99.9233074447271,
100.922665578293,101.922023711859,102.921381845425,103.672557568464),
 .UNSPECIFIED.);
#993=B_SPLINE_CURVE_WITH_KNOTS('',3,(#42617,#42618,#42619,#42620,#42621,
#42622,#42623,#42624,#42625,#42626),.UNSPECIFIED.,.F.,.F.,(4,1,1,1,1,1,
1,4),(91.1061869541045,91.9578984615291,92.9572565950951,93.9566147286612,
94.9559728622272,95.9553309957932,96.9546891293593,97.3893722612841),
 .UNSPECIFIED.);
#994=B_SPLINE_CURVE_WITH_KNOTS('',3,(#42627,#42628,#42629,#42630,#42631,
#42632,#42633,#42634,#42635,#42636),.UNSPECIFIED.,.F.,.F.,(4,1,1,1,1,1,
1,4),(91.1061869541048,91.9284423761987,92.9278005097648,93.9271586433308,
94.9265167768969,95.9258749104629,96.925233044029,97.3893722612845),
 .UNSPECIFIED.);
#995=B_SPLINE_CURVE_WITH_KNOTS('',3,(#42641,#42642,#42643,#42644,#42645,
#42646,#42647,#42648,#42649,#42650,#42651),.UNSPECIFIED.,.F.,.F.,(4,1,1,
1,1,1,1,1,4),(84.8230016469249,84.9623915265667,85.9617496601328,86.9611077936988,
87.9604659272649,88.9598240608309,89.959182194397,90.958540327963,91.1061869541045),
 .UNSPECIFIED.);
#996=B_SPLINE_CURVE_WITH_KNOTS('',3,(#42652,#42653,#42654,#42655,#42656,
#42657,#42658,#42659,#42660,#42661,#42662),.UNSPECIFIED.,.F.,.F.,(4,1,1,
1,1,1,1,1,4),(84.8230016469253,84.9329354412364,85.9322935748025,86.9316517083685,
87.9310098419346,88.9303679755006,89.9297261090666,90.9290842426327,91.1061869541048),
 .UNSPECIFIED.);
#997=B_SPLINE_CURVE_WITH_KNOTS('',3,(#42667,#42668,#42669,#42670,#42671,
#42672,#42673,#42674,#42675,#42676),.UNSPECIFIED.,.F.,.F.,(4,1,1,1,1,1,
1,4),(78.5398163397454,78.9662427251705,79.9656008587365,80.9649589923026,
81.9643171258686,82.9636752594347,83.9630333930007,84.8230016469249),
 .UNSPECIFIED.);
#998=B_SPLINE_CURVE_WITH_KNOTS('',3,(#42677,#42678,#42679,#42680,#42681,
#42682,#42683,#42684,#42685,#42686),.UNSPECIFIED.,.F.,.F.,(4,1,1,1,1,1,
1,4),(78.5398163397457,78.9367866398401,79.9361447734062,80.9355029069722,
81.9348610405383,82.9342191741043,83.9335773076704,84.8230016469253),
 .UNSPECIFIED.);
#999=B_SPLINE_CURVE_WITH_KNOTS('',3,(#42691,#42692,#42693,#42694,#42695,
#42696,#42697,#42698,#42699,#42700),.UNSPECIFIED.,.F.,.F.,(4,1,1,1,1,1,
1,4),(72.2566310325658,72.9700939237742,73.9694520573402,74.9688101909063,
75.9681683244723,76.9675264580384,77.9668845916044,78.5398163397454),
 .UNSPECIFIED.);
#1000=B_SPLINE_CURVE_WITH_KNOTS('',3,(#42701,#42702,#42703,#42704,#42705,
#42706,#42707,#42708,#42709,#42710),.UNSPECIFIED.,.F.,.F.,(4,1,1,1,1,1,
1,4),(72.2566310325661,72.9406378384438,73.9399959720099,74.9393541055759,
75.938712239142,76.938070372708,77.9374285062741,78.5398163397457),
 .UNSPECIFIED.);
#1001=B_SPLINE_CURVE_WITH_KNOTS('',3,(#42715,#42716,#42717,#42718,#42719,
#42720,#42721,#42722,#42723,#42724,#42725),.UNSPECIFIED.,.F.,.F.,(4,1,1,
1,1,1,1,1,4),(65.9734457253862,65.9745869888119,66.9739451223779,67.9733032559439,
68.97266138951,69.972019523076,70.9713776566421,71.9707357902081,72.2566310325658),
 .UNSPECIFIED.);
#1002=B_SPLINE_CURVE_WITH_KNOTS('',3,(#42726,#42727,#42728,#42729,#42730,
#42731,#42732,#42733,#42734,#42735),.UNSPECIFIED.,.F.,.F.,(4,1,1,1,1,1,
1,4),(65.9734457253865,66.9444890370476,67.9438471706136,68.9432053041797,
69.9425634377457,70.9419215713118,71.9412797048778,72.2566310325661),
 .UNSPECIFIED.);
#1003=B_SPLINE_CURVE_WITH_KNOTS('',3,(#42740,#42741,#42742,#42743,#42744,
#42745,#42746,#42747,#42748,#42749,#42750,#42751),.UNSPECIFIED.,.F.,.F.,
(4,1,1,1,1,1,1,1,1,4),(59.6902604182066,59.9784381874156,60.4781172541986,
60.9777963209816,61.4774753877646,61.9771544545477,62.9765125881137,63.9758707216798,
64.9752288552458,65.9734457253862),.UNSPECIFIED.);
#1004=B_SPLINE_CURVE_WITH_KNOTS('',3,(#42752,#42753,#42754,#42755,#42756,
#42757,#42758,#42759,#42760,#42761,#42762),.UNSPECIFIED.,.F.,.F.,(4,1,1,
1,1,1,1,1,4),(59.6902604182069,59.9489821020852,60.9483402356513,61.9476983692173,
62.9470565027834,63.9464146363494,64.9457727699155,65.9451309034815,65.9734457253865),
 .UNSPECIFIED.);
#1005=B_SPLINE_CURVE_WITH_KNOTS('',3,(#42767,#42768,#42769,#42770,#42771,
#42772,#42773,#42774,#42775,#42776,#42777,#42778,#42779,#42780,#42781,#42782,
#42783),.UNSPECIFIED.,.F.,.F.,(4,1,1,1,1,1,1,1,1,1,1,1,1,1,4),(53.407075111027,
53.4826103192363,53.9822893860193,54.4819684528023,54.9816475195853,55.4813265863684,
55.9810056531514,56.4806847199344,56.9803637867174,57.4800428535005,57.9797219202835,
58.4794009870665,58.9790800538495,59.4787591206325,59.6902604182066),
 .UNSPECIFIED.);
#1006=B_SPLINE_CURVE_WITH_KNOTS('',3,(#42784,#42785,#42786,#42787,#42788,
#42789,#42790,#42791,#42792,#42793,#42794,#42795,#42796,#42797,#42798,#42799),
 .UNSPECIFIED.,.F.,.F.,(4,1,1,1,1,1,1,1,1,1,1,1,1,4),(53.4070751110273,
53.4531542339059,53.9528333006889,54.452512367472,54.952191434255,55.451870501038,
55.951549567821,56.4512286346041,56.9509077013871,57.4505867681701,57.9502658349531,
58.4499449017362,58.9496239685192,59.6902604182069),.UNSPECIFIED.);
#1007=B_SPLINE_CURVE_WITH_KNOTS('',3,(#42804,#42805,#42806,#42807,#42808,
#42809,#42810,#42811,#42812,#42813,#42814,#42815,#42816,#42817,#42818,#42819),
 .UNSPECIFIED.,.F.,.F.,(4,1,1,1,1,1,1,1,1,1,1,1,1,4),(47.1238898038474,
47.48646151784,47.986140584623,48.485819651406,48.9854987181891,49.4851777849721,
49.9848568517551,50.4845359185381,50.9842149853212,51.4838940521042,51.9835731188872,
52.4832521856702,52.9829312524532,53.407075111027),.UNSPECIFIED.);
#1008=B_SPLINE_CURVE_WITH_KNOTS('',3,(#42820,#42821,#42822,#42823,#42824,
#42825,#42826,#42827,#42828,#42829,#42830,#42831,#42832,#42833,#42834,#42835),
 .UNSPECIFIED.,.F.,.F.,(4,1,1,1,1,1,1,1,1,1,1,1,1,4),(47.1238898038477,
47.4570054325096,47.9566844992927,48.4563635660757,48.9560426328587,49.4557216996417,
49.9554007664248,50.4550798332078,50.9547588999908,51.4544379667738,51.9541170335568,
52.4537961003399,52.9534751671229,53.4070751110273),.UNSPECIFIED.);
#1009=B_SPLINE_CURVE_WITH_KNOTS('',3,(#42840,#42841,#42842,#42843,#42844,
#42845,#42846,#42847,#42848,#42849,#42850,#42851,#42852,#42853,#42854,#42855,
#42856),.UNSPECIFIED.,.F.,.F.,(4,1,1,1,1,1,1,1,1,1,1,1,1,1,4),(40.8407044966678,
40.9906336496607,41.4903127164437,41.9899917832267,42.4896708500098,42.9893499167928,
43.4890289835758,43.9887080503588,44.4883871171419,44.9880661839249,45.4877452507079,
45.9874243174909,46.4871033842739,46.986782451057,47.1238898038474),
 .UNSPECIFIED.);
#1010=B_SPLINE_CURVE_WITH_KNOTS('',3,(#42857,#42858,#42859,#42860,#42861,
#42862,#42863,#42864,#42865,#42866,#42867,#42868,#42869,#42870,#42871,#42872,
#42873),.UNSPECIFIED.,.F.,.F.,(4,1,1,1,1,1,1,1,1,1,1,1,1,1,4),(40.8407044966681,
40.9611775643303,41.4608566311134,41.9605356978964,42.4602147646794,42.9598938314624,
43.4595728982454,43.9592519650285,44.4589310318115,44.9586100985945,45.4582891653775,
45.9579682321606,46.4576472989436,46.9573263657266,47.1238898038477),
 .UNSPECIFIED.);
#1011=B_SPLINE_CURVE_WITH_KNOTS('',3,(#42878,#42879,#42880,#42881,#42882,
#42883,#42884,#42885,#42886,#42887,#42888,#42889,#42890,#42891,#42892,#42893),
 .UNSPECIFIED.,.F.,.F.,(4,1,1,1,1,1,1,1,1,1,1,1,1,4),(34.5575191894882,
34.9944848482644,35.4941639150474,35.9938429818305,36.4935220486135,36.9932011153965,
37.4928801821795,37.9925592489626,38.4922383157456,38.9919173825286,39.4915964493116,
39.9912755160946,40.4909545828777,40.8407044966678),.UNSPECIFIED.);
#1012=B_SPLINE_CURVE_WITH_KNOTS('',3,(#42894,#42895,#42896,#42897,#42898,
#42899,#42900,#42901,#42902,#42903,#42904,#42905,#42906,#42907,#42908,#42909),
 .UNSPECIFIED.,.F.,.F.,(4,1,1,1,1,1,1,1,1,1,1,1,1,4),(34.5575191894886,
34.965028762934,35.4647078297171,35.9643868965001,36.4640659632831,36.9637450300661,
37.4634240968492,37.9631031636322,38.4627822304152,38.9624612971982,39.4621403639813,
39.9618194307643,40.4614984975473,40.8407044966681),.UNSPECIFIED.);
#1013=B_SPLINE_CURVE_WITH_KNOTS('',3,(#42914,#42915,#42916,#42917,#42918,
#42919,#42920,#42921,#42922,#42923,#42924,#42925,#42926,#42927,#42928,#42929,
#42930),.UNSPECIFIED.,.F.,.F.,(4,1,1,1,1,1,1,1,1,1,1,1,1,1,4),(28.2743338823086,
28.4986569800851,28.9983360468681,29.4980151136512,29.9976941804342,30.4973732472172,
30.9970523140002,31.4967313807832,31.9964104475663,32.4960895143493,32.9957685811323,
33.4954476479153,33.9951267146984,34.4948057814814,34.5575191894882),
 .UNSPECIFIED.);
#1014=B_SPLINE_CURVE_WITH_KNOTS('',3,(#42931,#42932,#42933,#42934,#42935,
#42936,#42937,#42938,#42939,#42940,#42941,#42942,#42943,#42944,#42945,#42946,
#42947),.UNSPECIFIED.,.F.,.F.,(4,1,1,1,1,1,1,1,1,1,1,1,1,1,4),(28.2743338823089,
28.4692008947547,28.9688799615378,29.4685590283208,29.9682380951038,30.4679171618868,
30.9675962286699,31.4672752954529,31.9669543622359,32.4666334290189,32.966312495802,
33.465991562585,33.965670629368,34.465349696151,34.5575191894886),
 .UNSPECIFIED.);
#1015=B_SPLINE_CURVE_WITH_KNOTS('',3,(#42952,#42953,#42954,#42955,#42956,
#42957,#42958,#42959,#42960,#42961,#42962,#42963,#42964,#42965,#42966,#42967,
#42968),.UNSPECIFIED.,.F.,.F.,(4,1,1,1,1,1,1,1,1,1,1,1,1,1,4),(21.991148575129,
22.0028291119058,22.5025081786888,23.0021872454719,23.5018663122549,24.0015453790379,
24.5012244458209,25.0009035126039,25.500582579387,26.00026164617,26.499940712953,
26.999619779736,27.4992988465191,27.9989779133021,28.2743338823086),
 .UNSPECIFIED.);
#1016=B_SPLINE_CURVE_WITH_KNOTS('',3,(#42969,#42970,#42971,#42972,#42973,
#42974,#42975,#42976,#42977,#42978,#42979,#42980,#42981,#42982,#42983,#42984),
 .UNSPECIFIED.,.F.,.F.,(4,1,1,1,1,1,1,1,1,1,1,1,1,4),(21.9911485751294,
22.4730520933585,22.9727311601415,23.4724102269245,23.9720892937075,24.4717683604905,
24.9714474272736,25.4711264940566,25.9708055608396,26.4704846276226,26.9701636944057,
27.4698427611887,27.9695218279717,28.2743338823089),.UNSPECIFIED.);
#1017=B_SPLINE_CURVE_WITH_KNOTS('',3,(#42989,#42990,#42991,#42992,#42993,
#42994,#42995,#42996,#42997,#42998,#42999,#43000,#43001,#43002,#43003,#43004),
 .UNSPECIFIED.,.F.,.F.,(4,1,1,1,1,1,1,1,1,1,1,1,1,4),(15.7079632679495,
16.0066803105095,16.5063593772925,17.0060384440756,17.5057175108586,18.0053965776416,
18.5050756444246,19.0047547112077,19.5044337779907,20.0041128447737,20.5037919115567,
21.0034709783398,21.5031500451228,21.991148575129),.UNSPECIFIED.);
#1018=B_SPLINE_CURVE_WITH_KNOTS('',3,(#43005,#43006,#43007,#43008,#43009,
#43010,#43011,#43012,#43013,#43014,#43015,#43016,#43017,#43018,#43019,#43020,
#43021),.UNSPECIFIED.,.F.,.F.,(4,1,1,1,1,1,1,1,1,1,1,1,1,1,4),(15.7079632679498,
15.9772242251791,16.4769032919622,16.9765823587452,17.4762614255282,17.9759404923112,
18.4756195590943,18.9752986258773,19.4749776926603,19.9746567594433,20.4743358262264,
20.9740148930094,21.4736939597924,21.9733730265754,21.9911485751294),
 .UNSPECIFIED.);
#1019=B_SPLINE_CURVE_WITH_KNOTS('',3,(#43026,#43027,#43028,#43029,#43030,
#43031,#43032,#43033,#43034,#43035,#43036,#43037,#43038,#43039,#43040,#43041,
#43042,#43043,#43044,#43045,#43046,#43047,#43048,#43049,#43050,#43051,#43052,
#43053,#43054,#43055,#43056,#43057,#43058,#43059,#43060,#43061,#43062),
 .UNSPECIFIED.,.F.,.F.,(4,3,3,3,3,3,3,3,3,3,3,3,4),(0.,0.000373494560508806,
0.0620760815771024,0.112839239637108,0.153038169722591,0.175804963675793,
0.247183842626883,0.319084136954533,0.344742425233931,0.363606980156396,
0.439518700737557,0.51795432283266,0.534785019937482),.UNSPECIFIED.);
#1020=B_SPLINE_CURVE_WITH_KNOTS('',3,(#43064,#43065,#43066,#43067,#43068,
#43069,#43070,#43071,#43072,#43073,#43074,#43075,#43076,#43077,#43078,#43079,
#43080,#43081,#43082,#43083,#43084,#43085,#43086,#43087,#43088,#43089,#43090,
#43091,#43092,#43093,#43094,#43095,#43096,#43097,#43098,#43099,#43100),
 .UNSPECIFIED.,.F.,.F.,(4,3,3,3,3,3,3,3,3,3,3,3,4),(0.,0.000511892384038064,
0.078754853834616,0.155070466132989,0.20164291816609,0.227017770490094,
0.290460834304131,0.352619921814331,0.383703668213755,0.403796492255862,
0.466621120797767,0.52704524650008,0.539097184344933),.UNSPECIFIED.);
#1021=B_SPLINE_CURVE_WITH_KNOTS('',3,(#45100,#45101,#45102,#45103,#45104,
#45105,#45106,#45107,#45108,#45109,#45110,#45111,#45112,#45113,#45114,#45115,
#45116,#45117,#45118,#45119,#45120,#45121,#45122,#45123,#45124,#45125,#45126,
#45127,#45128,#45129,#45130,#45131,#45132,#45133,#45134,#45135,#45136,#45137,
#45138,#45139),.UNSPECIFIED.,.F.,.F.,(4,3,3,3,3,3,3,3,3,3,3,3,3,4),(-0.53478501993692,
-0.534277081309421,-0.456439695901019,-0.38064245929011,-0.348102919117109,
-0.328886681298388,-0.258595553176405,-0.246742105655551,-0.185056579241663,
-0.163339235199672,-0.143463957830519,-0.0808484674142256,-0.0206857924044652,
0.),.UNSPECIFIED.);
#1022=B_SPLINE_CURVE_WITH_KNOTS('',3,(#45140,#45141,#45142,#45143,#45144,
#45145,#45146,#45147,#45148,#45149,#45150,#45151,#45152,#45153,#45154,#45155,
#45156,#45157,#45158,#45159,#45160,#45161,#45162,#45163,#45164),
 .UNSPECIFIED.,.F.,.F.,(4,3,3,3,3,3,3,3,4),(390.000549715688,390.249351157541,
390.749030224325,391.248709291108,391.748388357891,392.248067424674,392.747746491457,
393.24742555824,393.746279249921),.UNSPECIFIED.);
#1023=B_SPLINE_CURVE_WITH_KNOTS('',3,(#45165,#45166,#45167,#45168,#45169,
#45170,#45171,#45172,#45173,#45174,#45175,#45176,#45177,#45178,#45179),
 .UNSPECIFIED.,.F.,.F.,(4,1,1,1,1,1,1,1,1,1,1,1,4),(9.98190079888485,10.4807544905659,
10.9804335573489,11.4801126241319,11.979791690915,12.479470757698,12.979149824481,
13.478828891264,13.9785079580471,14.4781870248301,14.9778660916131,15.4775451583961,
15.7079632679498),.UNSPECIFIED.);
#1024=B_SPLINE_CURVE_WITH_KNOTS('',3,(#45181,#45182,#45183,#45184,#45185,
#45186,#45187,#45188,#45189,#45190,#45191),.UNSPECIFIED.,.F.,.F.,(4,1,1,
1,1,1,1,1,4),(12.0092477762453,12.5089268430284,13.0086059098114,13.5082849765944,
14.0079640433774,14.5076431101605,15.0073221769435,15.5070012437265,15.7079632679495),
 .UNSPECIFIED.);
#1025=B_SPLINE_CURVE_WITH_KNOTS('',3,(#47185,#47186,#47187,#47188,#47189,
#47190,#47191,#47192,#47193,#47194,#47195,#47196,#47197,#47198,#47199,#47200,
#47201,#47202,#47203,#47204,#47205,#47206,#47207,#47208,#47209,#47210,#47211,
#47212,#47213,#47214,#47215,#47216,#47217,#47218,#47219,#47220,#47221,#47222,
#47223,#47224),.UNSPECIFIED.,.F.,.F.,(4,3,3,3,3,3,3,3,3,3,3,3,3,4),(-0.539097184344981,
-0.538720824057998,-0.476544551511477,-0.429912347101587,-0.401091234701428,
-0.381803774975435,-0.313681369269712,-0.290015733871917,-0.24230273417063,
-0.214804629165427,-0.192593514291413,-0.116696500404398,-0.0381316372362206,
0.),.UNSPECIFIED.);
#1026=B_SPLINE_CURVE_WITH_KNOTS('',3,(#47225,#47226,#47227,#47228,#47229,
#47230,#47231,#47232,#47233,#47234),.UNSPECIFIED.,.F.,.F.,(4,3,3,4),(-394.746462758588,
-394.246783691805,-393.747104625022,-393.256204536838),.UNSPECIFIED.);
#1027=B_SPLINE_CURVE_WITH_KNOTS('',3,(#47301,#47302,#47303,#47304,#47305,
#47306,#47307,#47308),.UNSPECIFIED.,.F.,.F.,(4,2,2,4),(0.756005737987019,
0.793568827564653,0.872922520054208,0.952276212543762),.UNSPECIFIED.);
#1028=B_SPLINE_CURVE_WITH_KNOTS('',3,(#47311,#47312,#47313,#47314,#47315,
#47316,#47317,#47318,#47319,#47320,#47321,#47322,#47323,#47324),
 .UNSPECIFIED.,.F.,.F.,(4,2,2,2,2,2,4),(0.121154929624509,0.158718019202145,
0.238071711691699,0.317425404181254,0.396779096670809,0.476132789160363,
0.513695878738001),.UNSPECIFIED.);
#1029=B_SPLINE_CURVE_WITH_KNOTS('',3,(#47325,#47326,#47327,#47328,#47329,
#47330,#47331,#47332),.UNSPECIFIED.,.F.,.F.,(4,2,2,4),(0.952276212543762,
1.03162990503332,1.11098359752287,1.14854668710052),.UNSPECIFIED.);
#1030=B_SPLINE_CURVE_WITH_KNOTS('',3,(#47336,#47337,#47338,#47339,#47340,
#47341,#47342,#47343,#47344,#47345),.UNSPECIFIED.,.F.,.F.,(4,2,2,2,4),(0.,
0.0792165807733642,0.158433161546728,0.237648697074572,0.316864232602417),
 .UNSPECIFIED.);
#1031=B_SPLINE_CURVE_WITH_KNOTS('',3,(#47346,#47347,#47348,#47349,#47350,
#47351,#47352,#47353,#47354,#47355,#47356,#47357,#47358,#47359,#47360,#47361,
#47362,#47363,#47364,#47365,#47366,#47367,#47368,#47369,#47370,#47371),
 .UNSPECIFIED.,.F.,.F.,(4,2,2,2,2,2,2,2,2,2,2,2,4),(0.316864232602417,0.396079768130261,
0.475295303658105,0.554511884431469,0.633728465204833,0.712945045978197,
0.792161626751562,0.871377162279406,0.95059269780725,1.02980823333509,1.10902376886294,
1.1882403496363,1.26745693040967),.UNSPECIFIED.);
#1032=B_SPLINE_CURVE_WITH_KNOTS('',3,(#47403,#47404,#47405,#47406,#47407,
#47408),.UNSPECIFIED.,.F.,.F.,(4,2,4),(0.803821788694078,0.872950991853625,
0.952307212900975),.UNSPECIFIED.);
#1033=B_SPLINE_CURVE_WITH_KNOTS('',3,(#47411,#47412,#47413,#47414,#47415,
#47416,#47417,#47418,#47419,#47420),.UNSPECIFIED.,.F.,.F.,(4,2,2,2,4),(0.168950313426762,
0.238079516586309,0.317435737633658,0.396791958681008,0.465921161840561),
 .UNSPECIFIED.);
#1034=B_SPLINE_CURVE_WITH_KNOTS('',3,(#47421,#47422,#47423,#47424,#47425,
#47426),.UNSPECIFIED.,.F.,.F.,(4,2,4),(0.952307212900975,1.03166343394832,
1.10079263710787),.UNSPECIFIED.);
#1035=B_SPLINE_CURVE_WITH_KNOTS('',3,(#47430,#47431,#47432,#47433,#47434,
#47435,#47436,#47437,#47438,#47439),.UNSPECIFIED.,.F.,.F.,(4,2,2,2,4),(0.,
0.0792165807733642,0.158433161546728,0.237648697074572,0.316864232602417),
 .UNSPECIFIED.);
#1036=B_SPLINE_CURVE_WITH_KNOTS('',3,(#47440,#47441,#47442,#47443,#47444,
#47445,#47446,#47447,#47448,#47449,#47450,#47451,#47452,#47453,#47454,#47455,
#47456,#47457,#47458,#47459,#47460,#47461,#47462,#47463,#47464,#47465),
 .UNSPECIFIED.,.F.,.F.,(4,2,2,2,2,2,2,2,2,2,2,2,4),(0.316864232602417,0.396079768130261,
0.475295303658105,0.554511884431469,0.633728465204833,0.712945045978197,
0.792161626751562,0.871377162279406,0.95059269780725,1.02980823333509,1.10902376886294,
1.1882403496363,1.26745693040967),.UNSPECIFIED.);
#1037=B_SPLINE_CURVE_WITH_KNOTS('',3,(#48636,#48637,#48638,#48639,#48640,
#48641,#48642,#48643,#48644,#48645,#48646,#48647,#48648,#48649,#48650,#48651,
#48652,#48653,#48654,#48655,#48656,#48657),.UNSPECIFIED.,.F.,.F.,(4,2,2,
2,2,2,2,2,2,2,4),(0.0591825211272536,0.157966726598481,0.236950089897721,
0.315933453196962,0.391576304923761,0.46721915665056,0.54286200837736,0.618504860104159,
0.697488223403399,0.77647158670264,0.875255792173867),.UNSPECIFIED.);
#1038=B_SPLINE_CURVE_WITH_KNOTS('',3,(#48661,#48662,#48663,#48664,#48665,
#48666,#48667,#48668,#48669,#48670,#48671,#48672,#48673,#48674,#48675,#48676,
#48677,#48678,#48679,#48680,#48681,#48682),.UNSPECIFIED.,.F.,.F.,(4,2,2,
2,2,2,2,2,2,2,4),(0.0581119756758434,0.106553146291161,0.213106292582322,
0.30849933801665,0.386091982889075,0.4636846277615,0.541277272633925,0.61886991750635,
0.714262962940678,0.820816109231839,0.869257279847157),.UNSPECIFIED.);
#1039=B_SPLINE_CURVE_WITH_KNOTS('',3,(#48688,#48689,#48690,#48691,#48692,
#48693,#48694,#48695,#48696,#48697,#48698,#48699,#48700,#48701,#48702,#48703,
#48704,#48705,#48706,#48707,#48708,#48709),.UNSPECIFIED.,.F.,.F.,(4,2,2,
2,2,2,2,2,2,2,4),(0.0581119756758434,0.106553146291161,0.213106292582322,
0.30849933801665,0.386091982889075,0.4636846277615,0.541277272633925,0.61886991750635,
0.714262962940679,0.820816109231839,0.869257279847157),.UNSPECIFIED.);
#1040=B_SPLINE_CURVE_WITH_KNOTS('',3,(#48713,#48714,#48715,#48716,#48717,
#48718,#48719,#48720,#48721,#48722,#48723,#48724,#48725,#48726,#48727,#48728,
#48729,#48730,#48731,#48732,#48733,#48734),.UNSPECIFIED.,.F.,.F.,(4,2,2,
2,2,2,2,2,2,2,4),(0.0581119756758433,0.106553146291161,0.213106292582322,
0.308499338016649,0.386091982889075,0.4636846277615,0.541277272633925,0.61886991750635,
0.714262962940678,0.820816109231839,0.869257279847157),.UNSPECIFIED.);
#1041=B_SPLINE_CURVE_WITH_KNOTS('',3,(#48743,#48744,#48745,#48746,#48747,
#48748,#48749,#48750,#48751,#48752,#48753,#48754,#48755,#48756,#48757,#48758,
#48759,#48760,#48761,#48762,#48763,#48764),.UNSPECIFIED.,.F.,.F.,(4,2,2,
2,2,2,2,2,2,2,4),(0.0581119756758433,0.106553146291161,0.213106292582322,
0.30849933801665,0.386091982889075,0.4636846277615,0.541277272633925,0.61886991750635,
0.714262962940678,0.820816109231839,0.869257279847157),.UNSPECIFIED.);
#1042=B_SPLINE_CURVE_WITH_KNOTS('',3,(#48768,#48769,#48770,#48771,#48772,
#48773,#48774,#48775,#48776,#48777,#48778,#48779,#48780,#48781,#48782,#48783,
#48784,#48785,#48786,#48787,#48788,#48789),.UNSPECIFIED.,.F.,.F.,(4,2,2,
2,2,2,2,2,2,2,4),(0.0581119756758434,0.106553146291161,0.213106292582322,
0.30849933801665,0.386091982889075,0.4636846277615,0.541277272633925,0.61886991750635,
0.714262962940678,0.820816109231839,0.869257279847157),.UNSPECIFIED.);
#1043=B_SPLINE_CURVE_WITH_KNOTS('',3,(#48793,#48794,#48795,#48796,#48797,
#48798,#48799,#48800,#48801,#48802,#48803,#48804,#48805,#48806,#48807,#48808,
#48809,#48810,#48811,#48812,#48813,#48814),.UNSPECIFIED.,.F.,.F.,(4,2,2,
2,2,2,2,2,2,2,4),(0.0581119756758434,0.106553146291161,0.213106292582322,
0.30849933801665,0.386091982889075,0.4636846277615,0.541277272633925,0.61886991750635,
0.714262962940678,0.820816109231839,0.869257279847157),.UNSPECIFIED.);
#1044=B_SPLINE_CURVE_WITH_KNOTS('',3,(#48818,#48819,#48820,#48821,#48822,
#48823,#48824,#48825,#48826,#48827,#48828,#48829,#48830,#48831,#48832,#48833,
#48834,#48835,#48836,#48837,#48838,#48839),.UNSPECIFIED.,.F.,.F.,(4,2,2,
2,2,2,2,2,2,2,4),(0.0581119756758433,0.106553146291161,0.213106292582322,
0.30849933801665,0.386091982889075,0.4636846277615,0.541277272633925,0.61886991750635,
0.714262962940678,0.820816109231839,0.869257279847157),.UNSPECIFIED.);
#1045=B_SPLINE_CURVE_WITH_KNOTS('',3,(#48847,#48848,#48849,#48850,#48851,
#48852,#48853,#48854,#48855,#48856,#48857,#48858,#48859,#48860,#48861,#48862,
#48863,#48864,#48865,#48866,#48867,#48868),.UNSPECIFIED.,.F.,.F.,(4,2,2,
2,2,2,2,2,2,2,4),(0.0591825211272536,0.157966726598481,0.236950089897721,
0.315933453196962,0.391576304923761,0.467219156650561,0.54286200837736,
0.618504860104159,0.697488223403399,0.77647158670264,0.875255792173867),
 .UNSPECIFIED.);
#1046=B_SPLINE_CURVE_WITH_KNOTS('',3,(#48876,#48877,#48878,#48879,#48880,
#48881,#48882,#48883,#48884,#48885,#48886,#48887,#48888,#48889,#48890,#48891,
#48892,#48893,#48894,#48895,#48896,#48897),.UNSPECIFIED.,.F.,.F.,(4,2,2,
2,2,2,2,2,2,2,4),(0.0591825211272536,0.157966726598481,0.236950089897722,
0.315933453196962,0.391576304923761,0.467219156650561,0.54286200837736,
0.618504860104159,0.697488223403399,0.77647158670264,0.875255792173867),
 .UNSPECIFIED.);
#1047=B_SPLINE_CURVE_WITH_KNOTS('',3,(#48907,#48908,#48909,#48910,#48911,
#48912,#48913,#48914,#48915,#48916,#48917,#48918,#48919,#48920,#48921,#48922,
#48923,#48924,#48925,#48926,#48927,#48928),.UNSPECIFIED.,.F.,.F.,(4,2,2,
2,2,2,2,2,2,2,4),(0.0591825211272536,0.157966726598481,0.236950089897721,
0.315933453196962,0.391576304923761,0.46721915665056,0.54286200837736,0.618504860104159,
0.697488223403399,0.77647158670264,0.875255792173867),.UNSPECIFIED.);
#1048=B_SPLINE_CURVE_WITH_KNOTS('',3,(#48936,#48937,#48938,#48939,#48940,
#48941,#48942,#48943,#48944,#48945,#48946,#48947,#48948,#48949,#48950,#48951,
#48952,#48953,#48954,#48955,#48956,#48957),.UNSPECIFIED.,.F.,.F.,(4,2,2,
2,2,2,2,2,2,2,4),(0.0591825211272536,0.157966726598481,0.236950089897721,
0.315933453196962,0.391576304923761,0.46721915665056,0.542862008377359,
0.618504860104159,0.697488223403399,0.776471586702639,0.875255792173867),
 .UNSPECIFIED.);
#1049=B_SPLINE_CURVE_WITH_KNOTS('',3,(#48965,#48966,#48967,#48968,#48969,
#48970,#48971,#48972,#48973,#48974,#48975,#48976,#48977,#48978,#48979,#48980,
#48981,#48982,#48983,#48984,#48985,#48986),.UNSPECIFIED.,.F.,.F.,(4,2,2,
2,2,2,2,2,2,2,4),(0.0591825211272536,0.157966726598481,0.236950089897721,
0.315933453196962,0.391576304923761,0.46721915665056,0.54286200837736,0.618504860104159,
0.697488223403399,0.77647158670264,0.875255792173867),.UNSPECIFIED.);
#1050=B_SPLINE_CURVE_WITH_KNOTS('',3,(#48995,#48996,#48997,#48998,#48999,
#49000,#49001,#49002,#49003,#49004,#49005,#49006,#49007,#49008,#49009,#49010,
#49011,#49012,#49013,#49014,#49015,#49016),.UNSPECIFIED.,.F.,.F.,(4,2,2,
2,2,2,2,2,2,2,4),(0.0591825211272536,0.157966726598481,0.236950089897721,
0.315933453196962,0.391576304923761,0.46721915665056,0.542862008377359,
0.618504860104159,0.697488223403399,0.776471586702639,0.875255792173867),
 .UNSPECIFIED.);
#1051=B_SPLINE_CURVE_WITH_KNOTS('',3,(#49166,#49167,#49168,#49169,#49170,
#49171,#49172,#49173,#49174,#49175,#49176,#49177,#49178,#49179,#49180,#49181,
#49182,#49183,#49184,#49185,#49186,#49187),.UNSPECIFIED.,.F.,.F.,(4,2,2,
2,2,2,2,2,2,2,4),(0.0789094028588958,0.210573405340968,0.315860108011452,
0.421146810681936,0.522142632548711,0.623138454415485,0.72413427628226,
0.825130098149035,0.930416800819519,1.03570350349,1.16736750597208),
 .UNSPECIFIED.);
#1052=B_SPLINE_CURVE_WITH_KNOTS('',3,(#49191,#49192,#49193,#49194,#49195,
#49196,#49197,#49198,#49199,#49200,#49201,#49202,#49203,#49204,#49205,#49206,
#49207,#49208,#49209,#49210,#49211,#49212),.UNSPECIFIED.,.F.,.F.,(4,2,2,
2,2,2,2,2,2,2,4),(0.0774793363974613,0.142088896491891,0.284177792983782,
0.411119756996526,0.514392970548519,0.617666184100513,0.720939397652506,
0.8242126112045,0.951154575217244,1.09324347170913,1.15785303180356),
 .UNSPECIFIED.);
#1053=B_SPLINE_CURVE_WITH_KNOTS('',3,(#49218,#49219,#49220,#49221,#49222,
#49223,#49224,#49225,#49226,#49227,#49228,#49229,#49230,#49231,#49232,#49233,
#49234,#49235,#49236,#49237,#49238,#49239),.UNSPECIFIED.,.F.,.F.,(4,2,2,
2,2,2,2,2,2,2,4),(0.0774793363974613,0.142088896491891,0.284177792983782,
0.411119756996525,0.514392970548519,0.617666184100513,0.720939397652506,
0.8242126112045,0.951154575217243,1.09324347170913,1.15785303180356),
 .UNSPECIFIED.);
#1054=B_SPLINE_CURVE_WITH_KNOTS('',3,(#49243,#49244,#49245,#49246,#49247,
#49248,#49249,#49250,#49251,#49252,#49253,#49254,#49255,#49256,#49257,#49258,
#49259,#49260,#49261,#49262,#49263,#49264),.UNSPECIFIED.,.F.,.F.,(4,2,2,
2,2,2,2,2,2,2,4),(0.0774793363974614,0.142088896491891,0.284177792983781,
0.411119756996525,0.514392970548519,0.617666184100512,0.720939397652506,
0.824212611204499,0.951154575217243,1.09324347170913,1.15785303180356),
 .UNSPECIFIED.);
#1055=B_SPLINE_CURVE_WITH_KNOTS('',3,(#49268,#49269,#49270,#49271,#49272,
#49273,#49274,#49275,#49276,#49277,#49278,#49279),.UNSPECIFIED.,.F.,.F.,
(4,2,2,2,2,4),(0.0774793363974613,0.142088896491891,0.284177792983781,0.411119756996525,
0.514392970548519,0.617666184100512),.UNSPECIFIED.);
#1056=B_SPLINE_CURVE_WITH_KNOTS('',3,(#49284,#49285,#49286,#49287,#49288,
#49289,#49290,#49291,#49292,#49293,#49294,#49295),.UNSPECIFIED.,.F.,.F.,
(4,2,2,2,2,4),(0.617666184100512,0.720939397652506,0.824212611204499,0.951154575217243,
1.09324347170913,1.15785303180356),.UNSPECIFIED.);
#1057=B_SPLINE_CURVE_WITH_KNOTS('',3,(#49299,#49300,#49301,#49302,#49303,
#49304,#49305,#49306,#49307,#49308,#49309,#49310,#49311,#49312,#49313,#49314,
#49315,#49316,#49317,#49318,#49319,#49320),.UNSPECIFIED.,.F.,.F.,(4,2,2,
2,2,2,2,2,2,2,4),(0.0774793363974613,0.142088896491891,0.284177792983782,
0.411119756996526,0.514392970548519,0.617666184100513,0.720939397652507,
0.8242126112045,0.951154575217245,1.09324347170914,1.15785303180356),
 .UNSPECIFIED.);
#1058=B_SPLINE_CURVE_WITH_KNOTS('',3,(#49324,#49325,#49326,#49327,#49328,
#49329,#49330,#49331,#49332,#49333,#49334,#49335,#49336,#49337,#49338,#49339,
#49340,#49341,#49342,#49343,#49344,#49345),.UNSPECIFIED.,.F.,.F.,(4,2,2,
2,2,2,2,2,2,2,4),(0.0774793363974613,0.142088896491891,0.284177792983782,
0.411119756996526,0.514392970548519,0.617666184100513,0.720939397652506,
0.824212611204499,0.951154575217243,1.09324347170913,1.15785303180356),
 .UNSPECIFIED.);
#1059=B_SPLINE_CURVE_WITH_KNOTS('',3,(#49349,#49350,#49351,#49352,#49353,
#49354,#49355,#49356,#49357,#49358,#49359,#49360,#49361,#49362,#49363,#49364,
#49365,#49366,#49367,#49368,#49369,#49370),.UNSPECIFIED.,.F.,.F.,(4,2,2,
2,2,2,2,2,2,2,4),(0.0774793363974613,0.142088896491891,0.284177792983782,
0.411119756996526,0.514392970548519,0.617666184100513,0.720939397652506,
0.8242126112045,0.951154575217244,1.09324347170913,1.15785303180356),
 .UNSPECIFIED.);
#1060=B_SPLINE_CURVE_WITH_KNOTS('',3,(#49374,#49375,#49376,#49377,#49378,
#49379,#49380,#49381,#49382,#49383,#49384,#49385,#49386,#49387,#49388,#49389,
#49390,#49391,#49392,#49393,#49394,#49395),.UNSPECIFIED.,.F.,.F.,(4,2,2,
2,2,2,2,2,2,2,4),(0.0774793363974613,0.142088896491891,0.284177792983782,
0.411119756996526,0.514392970548519,0.617666184100513,0.720939397652506,
0.8242126112045,0.951154575217243,1.09324347170913,1.15785303180356),
 .UNSPECIFIED.);
#1061=B_SPLINE_CURVE_WITH_KNOTS('',3,(#49403,#49404,#49405,#49406,#49407,
#49408,#49409,#49410,#49411,#49412,#49413,#49414,#49415,#49416,#49417,#49418,
#49419,#49420,#49421,#49422,#49423,#49424),.UNSPECIFIED.,.F.,.F.,(4,2,2,
2,2,2,2,2,2,2,4),(0.0789094028588958,0.210573405340968,0.315860108011452,
0.421146810681936,0.522142632548711,0.623138454415485,0.72413427628226,
0.825130098149035,0.930416800819519,1.03570350349,1.16736750597208),
 .UNSPECIFIED.);
#1062=B_SPLINE_CURVE_WITH_KNOTS('',3,(#49432,#49433,#49434,#49435,#49436,
#49437,#49438,#49439,#49440,#49441,#49442,#49443,#49444,#49445,#49446,#49447,
#49448,#49449,#49450,#49451,#49452,#49453),.UNSPECIFIED.,.F.,.F.,(4,2,2,
2,2,2,2,2,2,2,4),(0.0789094028588958,0.210573405340969,0.315860108011453,
0.421146810681937,0.522142632548712,0.623138454415486,0.724134276282261,
0.825130098149035,0.930416800819519,1.03570350349,1.16736750597208),
 .UNSPECIFIED.);
#1063=B_SPLINE_CURVE_WITH_KNOTS('',3,(#49462,#49463,#49464,#49465,#49466,
#49467,#49468,#49469,#49470,#49471,#49472,#49473),.UNSPECIFIED.,.F.,.F.,
(4,2,2,2,2,4),(0.0789094028588958,0.210573405340968,0.315860108011452,0.421146810681937,
0.522142632548711,0.623138454415486),.UNSPECIFIED.);
#1064=B_SPLINE_CURVE_WITH_KNOTS('',3,(#49475,#49476,#49477,#49478,#49479,
#49480,#49481,#49482,#49483,#49484,#49485,#49486),.UNSPECIFIED.,.F.,.F.,
(4,2,2,2,2,4),(0.623138454415486,0.72413427628226,0.825130098149035,0.930416800819519,
1.03570350349,1.16736750597208),.UNSPECIFIED.);
#1065=B_SPLINE_CURVE_WITH_KNOTS('',3,(#49493,#49494,#49495,#49496,#49497,
#49498,#49499,#49500,#49501,#49502,#49503,#49504,#49505,#49506,#49507,#49508,
#49509,#49510,#49511,#49512,#49513,#49514),.UNSPECIFIED.,.F.,.F.,(4,2,2,
2,2,2,2,2,2,2,4),(0.0789094028588958,0.210573405340968,0.315860108011452,
0.421146810681936,0.522142632548711,0.623138454415486,0.72413427628226,
0.825130098149035,0.930416800819519,1.03570350349,1.16736750597208),
 .UNSPECIFIED.);
#1066=B_SPLINE_CURVE_WITH_KNOTS('',3,(#49522,#49523,#49524,#49525,#49526,
#49527,#49528,#49529,#49530,#49531,#49532,#49533,#49534,#49535,#49536,#49537,
#49538,#49539,#49540,#49541,#49542,#49543),.UNSPECIFIED.,.F.,.F.,(4,2,2,
2,2,2,2,2,2,2,4),(0.0789094028588957,0.210573405340968,0.315860108011452,
0.421146810681936,0.522142632548711,0.623138454415485,0.72413427628226,
0.825130098149035,0.930416800819519,1.03570350349,1.16736750597207),
 .UNSPECIFIED.);
#1067=B_SPLINE_CURVE_WITH_KNOTS('',3,(#49551,#49552,#49553,#49554,#49555,
#49556,#49557,#49558,#49559,#49560,#49561,#49562,#49563,#49564,#49565,#49566,
#49567,#49568,#49569,#49570,#49571,#49572),.UNSPECIFIED.,.F.,.F.,(4,2,2,
2,2,2,2,2,2,2,4),(0.0789094028588958,0.210573405340968,0.315860108011452,
0.421146810681936,0.522142632548711,0.623138454415486,0.72413427628226,
0.825130098149035,0.930416800819519,1.03570350349,1.16736750597208),
 .UNSPECIFIED.);
#1068=B_SPLINE_CURVE_WITH_KNOTS('',3,(#49581,#49582,#49583,#49584,#49585,
#49586,#49587,#49588,#49589,#49590,#49591,#49592,#49593,#49594,#49595,#49596,
#49597,#49598,#49599,#49600,#49601,#49602),.UNSPECIFIED.,.F.,.F.,(4,2,2,
2,2,2,2,2,2,2,4),(0.0789094028588958,0.210573405340968,0.315860108011452,
0.421146810681936,0.522142632548711,0.623138454415485,0.72413427628226,
0.825130098149035,0.930416800819519,1.03570350349,1.16736750597208),
 .UNSPECIFIED.);
#1069=B_SPLINE_CURVE_WITH_KNOTS('',3,(#50266,#50267,#50268,#50269,#50270,
#50271,#50272,#50273,#50274,#50275,#50276,#50277,#50278,#50279,#50280,#50281,
#50282,#50283,#50284,#50285,#50286,#50287,#50288,#50289,#50290),
 .UNSPECIFIED.,.F.,.F.,(4,3,3,3,3,3,3,3,4),(-3.56038179279204,-3.46201024481372,
-2.96743735269747,-2.47286446058123,-1.97829156846498,-1.48371867634874,
-0.989145784232491,-0.494572892116246,0.),.UNSPECIFIED.);
#1070=B_SPLINE_CURVE_WITH_KNOTS('',3,(#50293,#50294,#50295,#50296,#50297,
#50298,#50299,#50300,#50301,#50302,#50303,#50304,#50305,#50306,#50307,#50308,
#50309,#50310,#50311,#50312,#50313,#50314,#50315,#50316,#50317,#50318,#50319,
#50320,#50321,#50322,#50323,#50324,#50325,#50326,#50327,#50328,#50329,#50330,
#50331,#50332),.UNSPECIFIED.,.F.,.F.,(4,3,3,3,3,3,3,3,3,3,3,3,3,4),(0.937891254796418,
0.989145784232494,1.48371867634874,1.97829156846498,2.47286446058123,2.96743735269748,
3.46201024481372,3.95658313692997,4.45115602904621,4.94572892116246,5.44030181327871,
5.93487470539495,6.42944759751119,6.80228742277363),.UNSPECIFIED.);
#1071=B_SPLINE_CURVE_WITH_KNOTS('',3,(#50337,#50338,#50339,#50340,#50341,
#50342,#50343,#50344,#50345,#50346,#50347,#50348,#50349,#50350,#50351,#50352,
#50353,#50354,#50355,#50356,#50357,#50358,#50359,#50360,#50361,#50362,#50363,
#50364,#50365,#50366,#50367,#50368,#50369,#50370,#50371,#50372,#50373,#50374,
#50375,#50376),.UNSPECIFIED.,.F.,.F.,(4,3,3,3,3,3,3,3,3,3,3,3,3,4),(-9.8435670999716,
-9.39688495020867,-8.90231205809242,-8.40773916597618,-7.91316627385993,
-7.41859338174369,-6.92402048962744,-6.42944759751119,-5.93487470539495,
-5.4403018132787,-4.94572892116246,-4.45115602904621,-3.95658313692996,
-3.56038179279204),.UNSPECIFIED.);
#1072=B_SPLINE_CURVE_WITH_KNOTS('',3,(#50377,#50378,#50379,#50380,#50381,
#50382,#50383,#50384,#50385,#50386,#50387,#50388,#50389,#50390,#50391,#50392,
#50393,#50394,#50395,#50396,#50397,#50398,#50399,#50400,#50401,#50402,#50403,
#50404,#50405,#50406,#50407,#50408,#50409,#50410,#50411,#50412,#50413,#50414,
#50415,#50416,#50417,#50418,#50419),.UNSPECIFIED.,.F.,.F.,(4,3,3,3,3,3,
3,3,3,3,3,3,3,3,4),(6.80228742277363,6.92402048962744,7.41859338174369,
7.91316627385993,8.40773916597617,8.90231205809242,9.39688495020867,9.89145784232491,
10.3860307344412,10.8806036265574,11.3751765186736,11.8697494107899,12.3643223029061,
12.8588951950224,13.0854727299532),.UNSPECIFIED.);
#1073=B_SPLINE_CURVE_WITH_KNOTS('',3,(#50424,#50425,#50426,#50427,#50428,
#50429,#50430,#50431,#50432,#50433,#50434,#50435,#50436,#50437,#50438,#50439,
#50440,#50441,#50442,#50443,#50444,#50445,#50446,#50447,#50448,#50449,#50450,
#50451,#50452,#50453,#50454,#50455,#50456,#50457,#50458,#50459,#50460,#50461,
#50462,#50463,#50464,#50465,#50466),.UNSPECIFIED.,.F.,.F.,(4,3,3,3,3,3,
3,3,3,3,3,3,3,3,4),(-16.1267524071512,-15.8263325477199,-15.3317596556036,
-14.8371867634874,-14.3426138713711,-13.8480409792549,-13.3534680871386,
-12.8588951950224,-12.3643223029061,-11.8697494107899,-11.3751765186736,
-10.8806036265574,-10.3860307344412,-9.89145784232491,-9.8435670999716),
 .UNSPECIFIED.);
#1074=B_SPLINE_CURVE_WITH_KNOTS('',3,(#50467,#50468,#50469,#50470,#50471,
#50472,#50473,#50474,#50475,#50476,#50477,#50478,#50479,#50480,#50481,#50482,
#50483,#50484,#50485,#50486,#50487,#50488,#50489,#50490,#50491,#50492,#50493,
#50494,#50495,#50496,#50497,#50498,#50499,#50500,#50501,#50502,#50503,#50504,
#50505,#50506,#50507,#50508,#50509),.UNSPECIFIED.,.F.,.F.,(4,3,3,3,3,3,
3,3,3,3,3,3,3,3,4),(13.0854727299532,13.3534680871386,13.8480409792549,
14.3426138713711,14.8371867634874,15.3317596556036,15.8263325477199,16.3209054398361,
16.8154783319523,17.3100512240686,17.8046241161848,18.2991970083011,18.7937699004173,
19.2883427925336,19.3686580371328),.UNSPECIFIED.);
#1075=B_SPLINE_CURVE_WITH_KNOTS('',3,(#50514,#50515,#50516,#50517,#50518,
#50519,#50520,#50521,#50522,#50523,#50524,#50525,#50526,#50527,#50528,#50529,
#50530,#50531,#50532,#50533,#50534,#50535,#50536,#50537,#50538,#50539,#50540,
#50541,#50542,#50543,#50544,#50545,#50546,#50547,#50548,#50549,#50550,#50551,
#50552,#50553,#50554,#50555,#50556),.UNSPECIFIED.,.F.,.F.,(4,3,3,3,3,3,
3,3,3,3,3,3,3,3,4),(-22.4099377143308,-22.2557801452311,-21.7612072531148,
-21.2666343609986,-20.7720614688823,-20.2774885767661,-19.7829156846498,
-19.2883427925336,-18.7937699004173,-18.2991970083011,-17.8046241161848,
-17.3100512240686,-16.8154783319523,-16.3209054398361,-16.1267524071512),
 .UNSPECIFIED.);
#1076=B_SPLINE_CURVE_WITH_KNOTS('',3,(#50557,#50558,#50559,#50560,#50561,
#50562,#50563,#50564,#50565,#50566,#50567,#50568,#50569,#50570,#50571,#50572,
#50573,#50574,#50575,#50576,#50577,#50578,#50579,#50580,#50581,#50582,#50583,
#50584,#50585,#50586,#50587,#50588,#50589,#50590,#50591,#50592,#50593,#50594,
#50595,#50596),.UNSPECIFIED.,.F.,.F.,(4,3,3,3,3,3,3,3,3,3,3,3,3,4),(19.3686580371328,
19.7829156846498,20.2774885767661,20.7720614688823,21.2666343609986,21.7612072531148,
22.255780145231,22.7503530373473,23.2449259294635,23.7394988215798,24.234071713696,
24.7286446058123,25.2232174979285,25.6518433443124),.UNSPECIFIED.);
#1077=B_SPLINE_CURVE_WITH_KNOTS('',3,(#50601,#50602,#50603,#50604,#50605,
#50606,#50607,#50608,#50609,#50610,#50611,#50612,#50613,#50614,#50615,#50616,
#50617,#50618,#50619,#50620,#50621,#50622,#50623,#50624,#50625,#50626,#50627,
#50628,#50629,#50630,#50631,#50632,#50633,#50634,#50635,#50636,#50637,#50638,
#50639,#50640,#50641,#50642,#50643),.UNSPECIFIED.,.F.,.F.,(4,3,3,3,3,3,
3,3,3,3,3,3,3,3,4),(-28.6931230215104,-28.6852277427422,-28.190654850626,
-27.6960819585097,-27.2015090663935,-26.7069361742773,-26.212363282161,
-25.7177903900448,-25.2232174979285,-24.7286446058123,-24.234071713696,
-23.7394988215798,-23.2449259294635,-22.7503530373473,-22.4099377143308),
 .UNSPECIFIED.);
#1078=B_SPLINE_CURVE_WITH_KNOTS('',3,(#50644,#50645,#50646,#50647,#50648,
#50649,#50650,#50651,#50652,#50653,#50654,#50655,#50656,#50657,#50658,#50659,
#50660,#50661,#50662,#50663,#50664,#50665,#50666,#50667,#50668,#50669,#50670,
#50671,#50672,#50673,#50674,#50675,#50676,#50677,#50678,#50679,#50680,#50681,
#50682,#50683,#50684,#50685,#50686),.UNSPECIFIED.,.F.,.F.,(4,3,3,3,3,3,
3,3,3,3,3,3,3,3,4),(25.6518433443124,25.7177903900448,26.212363282161,26.7069361742773,
27.2015090663935,27.6960819585097,28.190654850626,28.6852277427422,29.1798006348585,
29.6743735269747,30.168946419091,30.6635193112072,31.1580922033235,31.6526650954397,
31.935028651492),.UNSPECIFIED.);
#1079=B_SPLINE_CURVE_WITH_KNOTS('',3,(#50691,#50692,#50693,#50694,#50695,
#50696,#50697,#50698,#50699,#50700,#50701,#50702,#50703,#50704,#50705,#50706,
#50707,#50708,#50709,#50710,#50711,#50712,#50713,#50714,#50715,#50716,#50717,
#50718,#50719,#50720,#50721,#50722,#50723,#50724,#50725,#50726,#50727,#50728,
#50729,#50730),.UNSPECIFIED.,.F.,.F.,(4,3,3,3,3,3,3,3,3,3,3,3,3,4),(-34.97630832869,
-34.6201024481372,-34.1255295560209,-33.6309566639047,-33.1363837717884,
-32.6418108796722,-32.147237987556,-31.6526650954397,-31.1580922033235,
-30.6635193112072,-30.168946419091,-29.6743735269747,-29.1798006348585,
-28.6931230215104),.UNSPECIFIED.);
#1080=B_SPLINE_CURVE_WITH_KNOTS('',3,(#50731,#50732,#50733,#50734,#50735,
#50736,#50737,#50738,#50739,#50740,#50741,#50742,#50743,#50744,#50745,#50746,
#50747,#50748,#50749,#50750,#50751,#50752,#50753,#50754,#50755,#50756,#50757,
#50758,#50759,#50760,#50761,#50762,#50763,#50764,#50765,#50766,#50767,#50768,
#50769,#50770,#50771,#50772,#50773),.UNSPECIFIED.,.F.,.F.,(4,3,3,3,3,3,
3,3,3,3,3,3,3,3,4),(31.935028651492,32.147237987556,32.6418108796722,33.1363837717885,
33.6309566639047,34.1255295560209,34.6201024481372,35.1146753402534,35.6092482323697,
36.1038211244859,36.5983940166022,37.0929669087184,37.5875398008347,38.0821126929509,
38.2182139586716),.UNSPECIFIED.);
#1081=B_SPLINE_CURVE_WITH_KNOTS('',3,(#50778,#50779,#50780,#50781,#50782,
#50783,#50784,#50785,#50786,#50787,#50788,#50789,#50790,#50791,#50792,#50793,
#50794,#50795,#50796,#50797,#50798,#50799,#50800,#50801,#50802,#50803,#50804,
#50805,#50806,#50807,#50808,#50809,#50810,#50811,#50812,#50813,#50814,#50815,
#50816,#50817,#50818,#50819,#50820),.UNSPECIFIED.,.F.,.F.,(4,3,3,3,3,3,
3,3,3,3,3,3,3,3,4),(-41.2594936358696,-41.0495500456484,-40.5549771535321,
-40.0604042614159,-39.5658313692996,-39.0712584771834,-38.5766855850671,
-38.0821126929509,-37.5875398008347,-37.0929669087184,-36.5983940166022,
-36.1038211244859,-35.6092482323697,-35.1146753402534,-34.97630832869),
 .UNSPECIFIED.);
#1082=B_SPLINE_CURVE_WITH_KNOTS('',3,(#50821,#50822,#50823,#50824,#50825,
#50826,#50827,#50828,#50829,#50830,#50831,#50832,#50833,#50834,#50835,#50836,
#50837,#50838,#50839,#50840,#50841,#50842,#50843,#50844,#50845,#50846,#50847,
#50848,#50849,#50850,#50851,#50852,#50853,#50854,#50855,#50856,#50857,#50858,
#50859,#50860),.UNSPECIFIED.,.F.,.F.,(4,3,3,3,3,3,3,3,3,3,3,3,3,4),(38.2182139586716,
38.5766855850671,39.0712584771834,39.5658313692996,40.0604042614159,40.5549771535321,
41.0495500456484,41.5441229377646,42.0386958298809,42.5332687219971,43.0278416141134,
43.5224145062296,44.0169873983459,44.5013992658512),.UNSPECIFIED.);
#1083=B_SPLINE_CURVE_WITH_KNOTS('',3,(#50865,#50866,#50867,#50868,#50869,
#50870,#50871,#50872,#50873,#50874,#50875,#50876,#50877,#50878,#50879,#50880,
#50881,#50882,#50883,#50884,#50885,#50886,#50887,#50888,#50889,#50890,#50891,
#50892,#50893,#50894,#50895,#50896,#50897,#50898,#50899,#50900,#50901,#50902,
#50903,#50904,#50905,#50906,#50907),.UNSPECIFIED.,.F.,.F.,(4,3,3,3,3,3,
3,3,3,3,3,3,3,3,4),(-47.5426789430491,-47.4789976431596,-46.9844247510433,
-46.4898518589271,-45.9952789668108,-45.5007060746946,-45.0061331825783,
-44.5115602904621,-44.0169873983458,-43.5224145062296,-43.0278416141134,
-42.5332687219971,-42.0386958298809,-41.5441229377646,-41.2594936358696),
 .UNSPECIFIED.);
#1084=B_SPLINE_CURVE_WITH_KNOTS('',3,(#50908,#50909,#50910,#50911,#50912,
#50913,#50914,#50915,#50916,#50917,#50918,#50919,#50920,#50921,#50922,#50923,
#50924,#50925,#50926,#50927,#50928,#50929,#50930,#50931,#50932,#50933,#50934,
#50935,#50936,#50937,#50938,#50939,#50940,#50941,#50942,#50943,#50944,#50945,
#50946,#50947,#50948,#50949,#50950),.UNSPECIFIED.,.F.,.F.,(4,3,3,3,3,3,
3,3,3,3,3,3,3,3,4),(44.5013992658512,44.5115602904621,45.0061331825783,
45.5007060746946,45.9952789668108,46.4898518589271,46.9844247510433,47.4789976431596,
47.9735705352758,48.4681434273921,48.9627163195083,49.4572892116245,49.9518621037408,
50.446434995857,50.7845845730308),.UNSPECIFIED.);
#1085=B_SPLINE_CURVE_WITH_KNOTS('',3,(#50957,#50958,#50959,#50960,#50961,
#50962,#50963,#50964,#50965,#50966),.UNSPECIFIED.,.F.,.F.,(4,3,3,4),(-54.4542726622231,
-54.403018132787,-53.9084452406708,-53.8258642502287),.UNSPECIFIED.);
#1086=B_SPLINE_CURVE_WITH_KNOTS('',3,(#50972,#50973,#50974,#50975,#50976,
#50977,#50978),.UNSPECIFIED.,.F.,.F.,(4,1,1,1,4),(65.9734457253856,66.0560267158277,
66.5505996079439,67.0451725000601,67.5397453921764),.UNSPECIFIED.);
#1087=B_SPLINE_CURVE_WITH_KNOTS('',3,(#50981,#50982,#50983,#50984,#50985,
#50986,#50987,#50988,#50989,#50990,#50991,#50992),.UNSPECIFIED.,.F.,.F.,
(4,1,1,1,1,1,1,1,1,4),(65.9734457253856,66.1298690403281,66.6244419324444,
67.1190148245607,67.6135877166769,68.1081606087931,68.6027335009094,69.0973063930256,
69.5918792851419,69.643133814578),.UNSPECIFIED.);
#1088=B_SPLINE_CURVE_WITH_KNOTS('',3,(#50997,#50998,#50999,#51000,#51001,
#51002,#51003,#51004,#51005,#51006,#51007,#51008,#51009,#51010,#51011,#51012),
 .UNSPECIFIED.,.F.,.F.,(4,1,1,1,1,1,1,1,1,1,1,1,1,4),(59.6902604182061,
60.1211520104327,60.615724902549,61.1102977946652,61.6048706867815,62.0994435788977,
62.5940164710139,63.0885893631302,63.5831622552464,64.0777351473627,64.5723080394789,
65.0668809315952,65.5614538237114,65.9734457253856),.UNSPECIFIED.);
#1089=B_SPLINE_CURVE_WITH_KNOTS('',3,(#51013,#51014,#51015,#51016,#51017,
#51018,#51019,#51020,#51021,#51022,#51023,#51024,#51025,#51026,#51027,#51028,
#51029),.UNSPECIFIED.,.F.,.F.,(4,1,1,1,1,1,1,1,1,1,1,1,1,1,4),(59.6902604182061,
59.700421442817,60.1949943349332,60.6895672270495,61.1841401191657,61.6787130112819,
62.1732859033982,62.6678587955144,63.1624316876307,63.6570045797469,64.1515774718632,
64.6461503639794,65.1407232560957,65.6352961482119,65.9734457253856),
 .UNSPECIFIED.);
#1090=B_SPLINE_CURVE_WITH_KNOTS('',3,(#51034,#51035,#51036,#51037,#51038,
#51039,#51040,#51041,#51042,#51043,#51044,#51045,#51046,#51047,#51048,#51049,
#51050),.UNSPECIFIED.,.F.,.F.,(4,1,1,1,1,1,1,1,1,1,1,1,1,1,4),(53.4070751110264,
53.6917044129215,54.1862773050378,54.680850197154,55.1754230892703,55.6699959813865,
56.1645688735028,56.659141765619,57.1537146577353,57.6482875498515,58.1428604419677,
58.637433334084,59.1320062262002,59.6265791183165,59.6902604182061),
 .UNSPECIFIED.);
#1091=B_SPLINE_CURVE_WITH_KNOTS('',3,(#51051,#51052,#51053,#51054,#51055,
#51056,#51057,#51058,#51059,#51060,#51061,#51062,#51063,#51064,#51065,#51066),
 .UNSPECIFIED.,.F.,.F.,(4,1,1,1,1,1,1,1,1,1,1,1,1,4),(53.4070751110264,
53.765546737422,54.2601196295383,54.7546925216545,55.2492654137708,55.743838305887,
56.2384111980032,56.7329840901195,57.2275569822357,57.722129874352,58.2167027664682,
58.7112756585845,59.2058485507007,59.6902604182061),.UNSPECIFIED.);
#1092=B_SPLINE_CURVE_WITH_KNOTS('',3,(#51071,#51072,#51073,#51074,#51075,
#51076,#51077,#51078,#51079,#51080,#51081,#51082,#51083,#51084,#51085,#51086,
#51087),.UNSPECIFIED.,.F.,.F.,(4,1,1,1,1,1,1,1,1,1,1,1,1,1,4),(47.1238898038469,
47.2622568154103,47.7568297075266,48.2514025996428,48.7459754917591,49.2405483838753,
49.7351212759916,50.2296941681078,50.7242670602241,51.2188399523403,51.7134128444565,
52.2079857365728,52.702558628689,53.1971315208053,53.4070751110264),
 .UNSPECIFIED.);
#1093=B_SPLINE_CURVE_WITH_KNOTS('',3,(#51088,#51089,#51090,#51091,#51092,
#51093,#51094,#51095,#51096,#51097,#51098,#51099,#51100,#51101,#51102,#51103,
#51104),.UNSPECIFIED.,.F.,.F.,(4,1,1,1,1,1,1,1,1,1,1,1,1,1,4),(47.1238898038469,
47.3360991399108,47.8306720320271,48.3252449241433,48.8198178162596,49.3143907083758,
49.8089636004921,50.3035364926083,50.7981093847245,51.2926822768408,51.787255168957,
52.2818280610733,52.7764009531895,53.2709738453058,53.4070751110264),
 .UNSPECIFIED.);
#1094=B_SPLINE_CURVE_WITH_KNOTS('',3,(#51109,#51110,#51111,#51112,#51113,
#51114,#51115,#51116,#51117,#51118,#51119,#51120,#51121,#51122,#51123,#51124),
 .UNSPECIFIED.,.F.,.F.,(4,1,1,1,1,1,1,1,1,1,1,1,1,4),(40.8407044966673,
41.3273821100154,41.8219550021316,42.3165278942479,42.8111007863641,43.3056736784804,
43.8002465705966,44.2948194627129,44.7893923548291,45.2839652469454,45.7785381390616,
46.2731110311778,46.7676839232941,47.1238898038469),.UNSPECIFIED.);
#1095=B_SPLINE_CURVE_WITH_KNOTS('',3,(#51125,#51126,#51127,#51128,#51129,
#51130,#51131,#51132,#51133,#51134,#51135,#51136,#51137,#51138,#51139,#51140,
#51141),.UNSPECIFIED.,.F.,.F.,(4,1,1,1,1,1,1,1,1,1,1,1,1,1,4),(40.8407044966673,
40.9066515423996,41.4012244345159,41.8957973266321,42.3903702187484,42.8849431108646,
43.3795160029809,43.8740888950971,44.3686617872134,44.8632346793296,45.3578075714458,
45.8523804635621,46.3469533556783,46.8415262477946,47.1238898038469),
 .UNSPECIFIED.);
#1096=B_SPLINE_CURVE_WITH_KNOTS('',3,(#51146,#51147,#51148,#51149,#51150,
#51151,#51152,#51153,#51154,#51155,#51156,#51157,#51158,#51159,#51160,#51161,
#51162),.UNSPECIFIED.,.F.,.F.,(4,1,1,1,1,1,1,1,1,1,1,1,1,1,4),(34.5575191894877,
34.8979345125042,35.3925074046204,35.8870802967367,36.3816531888529,36.8762260809692,
37.3707989730854,37.8653718652017,38.3599447573179,38.8545176494342,39.3490905415504,
39.8436634336667,40.3382363257829,40.8328092178991,40.8407044966673),
 .UNSPECIFIED.);
#1097=B_SPLINE_CURVE_WITH_KNOTS('',3,(#51163,#51164,#51165,#51166,#51167,
#51168,#51169,#51170,#51171,#51172,#51173,#51174,#51175,#51176,#51177,#51178),
 .UNSPECIFIED.,.F.,.F.,(4,1,1,1,1,1,1,1,1,1,1,1,1,4),(34.5575191894877,
34.9717768370047,35.4663497291209,35.9609226212372,36.4554955133534,36.9500684054697,
37.4446412975859,37.9392141897022,38.4337870818184,38.9283599739347,39.4229328660509,
39.9175057581671,40.4120786502834,40.8407044966673),.UNSPECIFIED.);
#1098=B_SPLINE_CURVE_WITH_KNOTS('',3,(#51183,#51184,#51185,#51186,#51187,
#51188,#51189,#51190,#51191,#51192,#51193,#51194,#51195,#51196,#51197,#51198,
#51199),.UNSPECIFIED.,.F.,.F.,(4,1,1,1,1,1,1,1,1,1,1,1,1,1,4),(28.2743338823081,
28.468486914993,28.9630598071093,29.4576326992255,29.9522055913417,30.446778483458,
30.9413513755742,31.4359242676905,31.9304971598067,32.425070051923,32.9196429440392,
33.4142158361555,33.9087887282717,34.403361620388,34.5575191894877),
 .UNSPECIFIED.);
#1099=B_SPLINE_CURVE_WITH_KNOTS('',3,(#51200,#51201,#51202,#51203,#51204,
#51205,#51206,#51207,#51208,#51209,#51210,#51211,#51212,#51213,#51214,#51215,
#51216),.UNSPECIFIED.,.F.,.F.,(4,1,1,1,1,1,1,1,1,1,1,1,1,1,4),(28.2743338823081,
28.5423292394935,29.0369021316097,29.531475023726,30.0260479158422,30.5206208079585,
31.0151937000747,31.509766592191,32.0043394843072,32.4989123764235,32.9934852685397,
33.488058160656,33.9826310527722,34.4772039448884,34.5575191894877),
 .UNSPECIFIED.);
#1100=B_SPLINE_CURVE_WITH_KNOTS('',3,(#51221,#51222,#51223,#51224,#51225,
#51226,#51227,#51228,#51229,#51230,#51231,#51232,#51233,#51234,#51235,#51236,
#51237),.UNSPECIFIED.,.F.,.F.,(4,1,1,1,1,1,1,1,1,1,1,1,1,1,4),(21.9911485751285,
22.0390393174818,22.5336122095981,23.0281851017143,23.5227579938306,24.0173308859468,
24.511903778063,25.0064766701793,25.5010495622955,25.9956224544118,26.490195346528,
26.9847682386443,27.4793411307605,27.9739140228768,28.2743338823081),
 .UNSPECIFIED.);
#1101=B_SPLINE_CURVE_WITH_KNOTS('',3,(#51238,#51239,#51240,#51241,#51242,
#51243,#51244,#51245,#51246,#51247,#51248,#51249,#51250,#51251,#51252,#51253,
#51254),.UNSPECIFIED.,.F.,.F.,(4,1,1,1,1,1,1,1,1,1,1,1,1,1,4),(21.9911485751285,
22.1128816419823,22.6074545340986,23.1020274262148,23.596600318331,24.0911732104473,
24.5857461025635,25.0803189946798,25.574891886796,26.0694647789123,26.5640376710285,
27.0586105631448,27.553183455261,28.0477563473773,28.2743338823081),
 .UNSPECIFIED.);
#1102=B_SPLINE_CURVE_WITH_KNOTS('',3,(#51260,#51261,#51262,#51263,#51264),
 .UNSPECIFIED.,.F.,.F.,(4,1,4),(15.1888611523549,15.6834340444711,15.7079632679489),
 .UNSPECIFIED.);
#1103=B_SPLINE_CURVE_WITH_KNOTS('',3,(#51267,#51268,#51269,#51270,#51271,
#51272,#51273,#51274,#51275,#51276),.UNSPECIFIED.,.F.,.F.,(4,1,1,1,1,1,
1,4),(13.0854727299533,13.1367272593894,13.6313001515056,14.1258730436219,
14.6204459357381,15.1150188278544,15.6095917199706,15.7079632679489),
 .UNSPECIFIED.);
#1104=B_SPLINE_CURVE_WITH_KNOTS('',3,(#51278,#51279,#51280,#51281,#51282,
#51283,#51284,#51285,#51286,#51287,#51288,#51289,#51290,#51291,#51292,#51293),
 .UNSPECIFIED.,.F.,.F.,(4,1,1,1,1,1,1,1,1,1,1,1,1,4),(15.7079632679489,
16.1041646120869,16.5987375042031,17.0933103963194,17.5878832884356,18.0824561805519,
18.5770290726681,19.0716019647843,19.5661748569006,20.0607477490168,20.5553206411331,
21.0498935332493,21.5444664253656,21.9911485751285),.UNSPECIFIED.);
#1105=B_SPLINE_CURVE_WITH_KNOTS('',3,(#51294,#51295,#51296,#51297,#51298,
#51299,#51300,#51301,#51302,#51303,#51304,#51305,#51306,#51307,#51308,#51309),
 .UNSPECIFIED.,.F.,.F.,(4,1,1,1,1,1,1,1,1,1,1,1,1,4),(15.7079632679489,
16.1780069365874,16.6725798287036,17.1671527208199,17.6617256129361,18.1562985050523,
18.6508713971686,19.1454442892848,19.6400171814011,20.1345900735173,20.6291629656336,
21.1237358577498,21.6183087498661,21.9911485751285),.UNSPECIFIED.);
#1106=B_SPLINE_CURVE_WITH_KNOTS('',3,(#51770,#51771,#51772,#51773,#51774,
#51775,#51776,#51777,#51778,#51779,#51780,#51781,#51782,#51783,#51784,#51785,
#51786,#51787,#51788,#51789,#51790,#51791,#51792,#51793,#51794,#51795,#51796,
#51797,#51798,#51799,#51800),.UNSPECIFIED.,.F.,.F.,(4,3,3,3,3,3,3,3,3,3,
4),(0.,0.0822466706468383,0.162608105240606,0.216579893838171,0.23924274204394,
0.301838371937517,0.36076250940623,0.388067588559334,0.409537377502954,
0.476290104322315,0.53753492181237),.UNSPECIFIED.);
#1107=B_SPLINE_CURVE_WITH_KNOTS('',3,(#51801,#51802,#51803,#51804,#51805,
#51806,#51807,#51808,#51809,#51810,#51811,#51812,#51813,#51814,#51815,#51816,
#51817,#51818,#51819,#51820,#51821,#51822,#51823,#51824,#51825,#51826,#51827,
#51828),.UNSPECIFIED.,.F.,.F.,(4,3,3,3,3,3,3,3,3,4),(0.,0.0665230127441691,
0.13429495842692,0.176258819244205,0.195926107024299,0.263526952009386,
0.33682854572103,0.365338415901403,0.449700157257057,0.534061898612711),
 .UNSPECIFIED.);
#1108=B_SPLINE_CURVE_WITH_KNOTS('',3,(#51829,#51830,#51831,#51832,#51833,
#51834,#51835,#51836,#51837,#51838,#51839,#51840,#51841,#51842,#51843,#51844,
#51845,#51846,#51847,#51848,#51849,#51850,#51851,#51852,#51853,#51854,#51855,
#51856,#51857,#51858,#51859,#51860,#51861,#51862,#51863,#51864,#51865,#51866,
#51867,#51868),.UNSPECIFIED.,.F.,.F.,(4,3,3,3,3,3,3,3,3,3,3,3,3,4),(-53.8258642502287,
-53.4138723485545,-52.9192994564383,-52.424726564322,-51.9301536722058,
-51.4355807800895,-50.9410078879733,-50.446434995857,-49.9518621037408,
-49.4572892116245,-48.9627163195083,-48.4681434273921,-47.9735705352758,
-47.5426789430491),.UNSPECIFIED.);
#1109=B_SPLINE_CURVE_WITH_KNOTS('',3,(#52330,#52331,#52332,#52333,#52334,
#52335,#52336,#52337,#52338,#52339,#52340,#52341,#52342,#52343,#52344,#52345,
#52346,#52347,#52348,#52349,#52350,#52351,#52352,#52353,#52354,#52355,#52356,
#52357),.UNSPECIFIED.,.F.,.F.,(4,3,3,3,3,3,3,3,3,4),(0.,0.0665230199567328,
0.134294967830964,0.176258831509978,0.195926124443112,0.263526952009376,
0.336828549458816,0.365338416771381,0.449700157692121,0.534061898612861),
 .UNSPECIFIED.);
#1110=B_SPLINE_CURVE_WITH_KNOTS('',3,(#52358,#52359,#52360,#52361,#52362,
#52363,#52364,#52365,#52366,#52367,#52368,#52369,#52370,#52371,#52372,#52373,
#52374,#52375,#52376,#52377,#52378,#52379,#52380,#52381,#52382,#52383,#52384,
#52385,#52386,#52387,#52388),.UNSPECIFIED.,.F.,.F.,(4,3,3,3,3,3,3,3,3,3,
4),(50.7845845730308,50.9410078879733,51.4355807800895,51.9301536722058,
52.424726564322,52.9192994564383,53.4138723485545,53.9084452406708,54.403018132787,
54.8975910249033,55.3921639170195),.UNSPECIFIED.);
#1111=B_SPLINE_CURVE_WITH_KNOTS('',3,(#52389,#52390,#52391,#52392,#52393,
#52394,#52395,#52396,#52397,#52398,#52399,#52400,#52401,#52402,#52403,#52404,
#52405,#52406,#52407,#52408,#52409,#52410,#52411,#52412,#52413,#52414,#52415,
#52416,#52417,#52418,#52419),.UNSPECIFIED.,.F.,.F.,(4,3,3,3,3,3,3,3,3,3,
4),(0.,0.0822466663612967,0.162608100396307,0.216579890867136,0.239242742625966,
0.301838371937549,0.360762509406336,0.388067584071394,0.409537375230468,
0.476290092032249,0.537534921812695),.UNSPECIFIED.);
#1112=B_SPLINE_CURVE_WITH_KNOTS('',3,(#52628,#52629,#52630,#52631,#52632,
#52633,#52634,#52635,#52636,#52637,#52638,#52639,#52640,#52641,#52642,#52643,
#52644,#52645,#52646),.UNSPECIFIED.,.F.,.F.,(4,3,3,3,3,3,4),(-3.69871549170445,
-3.49775346748116,-2.99807440069814,-2.49839533391511,-1.99871626713209,
-1.49903720034907,-1.00018350866767),.UNSPECIFIED.);
#1113=B_SPLINE_CURVE_WITH_KNOTS('',3,(#52649,#52650,#52651,#52652),
 .UNSPECIFIED.,.F.,.F.,(4,4),(0.,0.443060670554495),.UNSPECIFIED.);
#1114=B_SPLINE_CURVE_WITH_KNOTS('',3,(#52657,#52658,#52659,#52660,#52661,
#52662,#52663,#52664,#52665,#52666,#52667,#52668,#52669,#52670,#52671,#52672,
#52673,#52674,#52675,#52676,#52677,#52678,#52679,#52680,#52681,#52682,#52683,
#52684,#52685,#52686,#52687,#52688,#52689,#52690,#52691,#52692,#52693,#52694,
#52695,#52696),.UNSPECIFIED.,.F.,.F.,(4,3,3,3,3,3,3,3,3,3,3,3,3,4),(-9.98190079888403,
-9.49390226887744,-8.99422320209442,-8.4945441353114,-7.99486506852837,
-7.49518600174535,-6.99550693496233,-6.4958278681793,-5.99614880139628,
-5.49646973461325,-4.99679066783023,-4.49711160104721,-3.99743253426419,
-3.69871549170445),.UNSPECIFIED.);
#1115=B_SPLINE_CURVE_WITH_KNOTS('',3,(#52697,#52698,#52699,#52700,#52701,
#52702,#52703,#52704,#52705,#52706,#52707,#52708,#52709,#52710,#52711,#52712,
#52713,#52714,#52715,#52716,#52717,#52718,#52719,#52720,#52721,#52722,#52723,
#52724,#52725,#52726,#52727,#52728,#52729,#52730,#52731,#52732,#52733,#52734,
#52735,#52736,#52737,#52738,#52739),.UNSPECIFIED.,.F.,.F.,(4,3,3,3,3,3,
3,3,3,3,3,3,3,3,4),(0.443060670554495,0.49967906678306,0.999358133566079,
1.4990372003491,1.99871626713212,2.49839533391514,2.99807440069816,3.49775346748117,
3.99743253426419,4.49711160104721,4.99679066783023,5.49646973461325,5.99614880139627,
6.49582786817929,6.72624597773408),.UNSPECIFIED.);
#1116=B_SPLINE_CURVE_WITH_KNOTS('',3,(#52744,#52745,#52746,#52747,#52748,
#52749,#52750,#52751,#52752,#52753,#52754,#52755,#52756,#52757,#52758,#52759,
#52760,#52761,#52762,#52763,#52764,#52765,#52766,#52767,#52768,#52769,#52770,
#52771,#52772,#52773,#52774,#52775,#52776,#52777,#52778,#52779,#52780,#52781,
#52782,#52783,#52784,#52785,#52786),.UNSPECIFIED.,.F.,.F.,(4,3,3,3,3,3,
3,3,3,3,3,3,3,3,4),(-16.2650861060636,-15.9897301370567,-15.4900510702737,
-14.9903720034907,-14.4906929367077,-13.9910138699247,-13.4913348031416,
-12.9916557363586,-12.4919766695756,-11.9922976027926,-11.4926185360095,
-10.9929394692265,-10.4932604024435,-9.99358133566046,-9.98190079888403),
 .UNSPECIFIED.);
#1117=B_SPLINE_CURVE_WITH_KNOTS('',3,(#52787,#52788,#52789,#52790,#52791,
#52792,#52793,#52794,#52795,#52796,#52797,#52798,#52799,#52800,#52801,#52802,
#52803,#52804,#52805,#52806,#52807,#52808,#52809,#52810,#52811,#52812,#52813,
#52814,#52815,#52816,#52817,#52818,#52819,#52820,#52821,#52822,#52823,#52824,
#52825,#52826,#52827,#52828,#52829),.UNSPECIFIED.,.F.,.F.,(4,3,3,3,3,3,
3,3,3,3,3,3,3,3,4),(6.72624597773408,6.99550693496231,7.49518600174534,
7.99486506852837,8.49454413531139,8.99422320209442,9.49390226887745,9.99358133566048,
10.4932604024435,10.9929394692265,11.4926185360096,11.9922976027926,12.4919766695756,
12.9916557363586,13.0094312849137),.UNSPECIFIED.);
#1118=B_SPLINE_CURVE_WITH_KNOTS('',3,(#52834,#52835,#52836,#52837,#52838,
#52839,#52840,#52841,#52842,#52843,#52844,#52845,#52846,#52847,#52848,#52849,
#52850,#52851,#52852,#52853,#52854,#52855,#52856,#52857,#52858,#52859,#52860,
#52861,#52862,#52863,#52864,#52865,#52866,#52867,#52868,#52869,#52870,#52871,
#52872,#52873,#52874,#52875,#52876),.UNSPECIFIED.,.F.,.F.,(4,3,3,3,3,3,
3,3,3,3,3,3,3,3,4),(-22.5482714132432,-22.485558005236,-21.985878938453,
-21.48619987167,-20.986520804887,-20.486841738104,-19.9871626713209,-19.4874836045379,
-18.9878045377549,-18.4881254709719,-17.9884464041888,-17.4887673374058,
-16.9890882706228,-16.4894092038398,-16.2650861060636),.UNSPECIFIED.);
#1119=B_SPLINE_CURVE_WITH_KNOTS('',3,(#52877,#52878,#52879,#52880,#52881,
#52882,#52883,#52884,#52885,#52886,#52887,#52888,#52889,#52890,#52891,#52892,
#52893,#52894,#52895,#52896,#52897,#52898,#52899,#52900,#52901,#52902,#52903,
#52904,#52905,#52906,#52907,#52908,#52909,#52910,#52911,#52912,#52913,#52914,
#52915,#52916),.UNSPECIFIED.,.F.,.F.,(4,3,3,3,3,3,3,3,3,3,3,3,3,4),(13.0094312849137,
13.4913348031417,13.9910138699247,14.4906929367077,14.9903720034907,15.4900510702737,
15.9897301370568,16.4894092038398,16.9890882706228,17.4887673374058,17.9884464041888,
18.4881254709718,18.9878045377549,19.2926165920933),.UNSPECIFIED.);
#1120=B_SPLINE_CURVE_WITH_KNOTS('',3,(#52921,#52922,#52923,#52924,#52925,
#52926,#52927,#52928,#52929,#52930,#52931,#52932,#52933,#52934,#52935,#52936,
#52937,#52938,#52939,#52940,#52941,#52942,#52943,#52944,#52945,#52946,#52947,
#52948,#52949,#52950,#52951,#52952,#52953,#52954,#52955,#52956,#52957,#52958,
#52959,#52960),.UNSPECIFIED.,.F.,.F.,(4,3,3,3,3,3,3,3,3,3,3,3,3,4),(-28.8314567204228,
-28.4817068066323,-27.9820277398493,-27.4823486730663,-26.9826696062833,
-26.4829905395002,-25.9833114727172,-25.4836324059342,-24.9839533391512,
-24.4842742723681,-23.9845952055851,-23.4849161388021,-22.9852370720191,
-22.5482714132432),.UNSPECIFIED.);
#1121=B_SPLINE_CURVE_WITH_KNOTS('',3,(#52961,#52962,#52963,#52964,#52965,
#52966,#52967,#52968,#52969,#52970,#52971,#52972,#52973,#52974,#52975,#52976,
#52977,#52978,#52979,#52980,#52981,#52982,#52983,#52984,#52985,#52986,#52987,
#52988,#52989,#52990,#52991,#52992,#52993,#52994,#52995,#52996,#52997,#52998,
#52999,#53000,#53001,#53002,#53003),.UNSPECIFIED.,.F.,.F.,(4,3,3,3,3,3,
3,3,3,3,3,3,3,3,4),(19.2926165920933,19.4874836045379,19.9871626713209,
20.4868417381039,20.986520804887,21.48619987167,21.985878938453,22.4855580052361,
22.9852370720191,23.4849161388021,23.9845952055851,24.4842742723682,24.9839533391512,
25.4836324059342,25.5758018992728),.UNSPECIFIED.);
#1122=B_SPLINE_CURVE_WITH_KNOTS('',3,(#53008,#53009,#53010,#53011,#53012,
#53013,#53014,#53015,#53016,#53017,#53018,#53019,#53020,#53021,#53022,#53023,
#53024,#53025,#53026,#53027,#53028,#53029,#53030,#53031,#53032,#53033,#53034,
#53035,#53036,#53037,#53038,#53039,#53040,#53041,#53042,#53043,#53044,#53045,
#53046,#53047,#53048,#53049,#53050),.UNSPECIFIED.,.F.,.F.,(4,3,3,3,3,3,
3,3,3,3,3,3,3,3,4),(-35.1146420276024,-34.9775346748116,-34.4778556080286,
-33.9781765412456,-33.4784974744626,-32.9788184076795,-32.4791393408965,
-31.9794602741135,-31.4797812073305,-30.9801021405474,-30.4804230737644,
-29.9807440069814,-29.4810649401984,-28.9813858734153,-28.8314567204228),
 .UNSPECIFIED.);
#1123=B_SPLINE_CURVE_WITH_KNOTS('',3,(#53051,#53052,#53053,#53054,#53055,
#53056,#53057,#53058,#53059,#53060,#53061,#53062,#53063,#53064,#53065,#53066,
#53067,#53068,#53069,#53070,#53071,#53072,#53073,#53074,#53075,#53076,#53077,
#53078,#53079,#53080,#53081,#53082,#53083,#53084,#53085,#53086,#53087,#53088,
#53089,#53090),.UNSPECIFIED.,.F.,.F.,(4,3,3,3,3,3,3,3,3,3,3,3,3,4),(25.5758018992728,
25.9833114727172,26.4829905395003,26.9826696062833,27.4823486730663,27.9820277398493,
28.4817068066324,28.9813858734154,29.4810649401984,29.9807440069814,30.4804230737645,
30.9801021405475,31.4797812073305,31.8589872064524),.UNSPECIFIED.);
#1124=B_SPLINE_CURVE_WITH_KNOTS('',3,(#53095,#53096,#53097,#53098,#53099,
#53100,#53101,#53102,#53103,#53104,#53105,#53106,#53107,#53108,#53109,#53110,
#53111,#53112,#53113,#53114,#53115,#53116,#53117,#53118,#53119,#53120,#53121,
#53122,#53123,#53124,#53125,#53126,#53127,#53128,#53129,#53130,#53131,#53132,
#53133,#53134),.UNSPECIFIED.,.F.,.F.,(4,3,3,3,3,3,3,3,3,3,3,3,3,4),(-41.397827334782,
-40.9736834762079,-40.4740044094249,-39.9743253426419,-39.4746462758588,
-38.9749672090758,-38.4752881422928,-37.9756090755098,-37.4759300087267,
-36.9762509419437,-36.4765718751607,-35.9768928083777,-35.4772137415947,
-35.1146420276024),.UNSPECIFIED.);
#1125=B_SPLINE_CURVE_WITH_KNOTS('',3,(#53135,#53136,#53137,#53138,#53139,
#53140,#53141,#53142,#53143,#53144,#53145,#53146,#53147,#53148,#53149,#53150,
#53151,#53152,#53153,#53154,#53155,#53156,#53157,#53158,#53159,#53160,#53161,
#53162,#53163,#53164,#53165,#53166,#53167,#53168,#53169,#53170,#53171,#53172,
#53173,#53174,#53175,#53176,#53177),.UNSPECIFIED.,.F.,.F.,(4,3,3,3,3,3,
3,3,3,3,3,3,3,3,4),(31.8589872064524,31.9794602741135,32.4791393408966,
32.9788184076796,33.4784974744626,33.9781765412456,34.4778556080286,34.9775346748117,
35.4772137415947,35.9768928083777,36.4765718751607,36.9762509419437,37.4759300087267,
37.9756090755098,38.142172513632),.UNSPECIFIED.);
#1126=B_SPLINE_CURVE_WITH_KNOTS('',3,(#53182,#53183,#53184,#53185,#53186,
#53187,#53188,#53189,#53190,#53191,#53192,#53193,#53194,#53195,#53196,#53197,
#53198,#53199,#53200,#53201,#53202,#53203,#53204,#53205,#53206,#53207,#53208,
#53209,#53210,#53211,#53212,#53213,#53214,#53215,#53216,#53217,#53218,#53219,
#53220,#53221,#53222,#53223,#53224),.UNSPECIFIED.,.F.,.F.,(4,3,3,3,3,3,
3,3,3,3,3,3,3,3,4),(-47.6810126419616,-47.4695113443872,-46.9698322776042,
-46.4701532108212,-45.9704741440381,-45.4707950772551,-44.9711160104721,
-44.4714369436891,-43.971757876906,-43.472078810123,-42.97239974334,-42.472720676557,
-41.973041609774,-41.4733625429909,-41.397827334782),.UNSPECIFIED.);
#1127=B_SPLINE_CURVE_WITH_KNOTS('',3,(#53225,#53226,#53227,#53228,#53229,
#53230,#53231,#53232,#53233,#53234,#53235,#53236,#53237,#53238,#53239,#53240,
#53241,#53242,#53243,#53244,#53245,#53246,#53247,#53248,#53249,#53250,#53251,
#53252,#53253,#53254,#53255,#53256,#53257,#53258,#53259,#53260,#53261,#53262,
#53263,#53264),.UNSPECIFIED.,.F.,.F.,(4,3,3,3,3,3,3,3,3,3,3,3,3,4),(38.142172513632,
38.4752881422928,38.9749672090758,39.4746462758589,39.9743253426419,40.4740044094249,
40.973683476208,41.473362542991,41.973041609774,42.472720676557,42.9723997433401,
43.4720788101231,43.9717578769061,44.4253578208116),.UNSPECIFIED.);
#1128=B_SPLINE_CURVE_WITH_KNOTS('',3,(#53269,#53270,#53271,#53272,#53273,
#53274,#53275,#53276,#53277,#53278,#53279,#53280,#53281,#53282,#53283,#53284,
#53285,#53286,#53287,#53288,#53289,#53290,#53291,#53292,#53293,#53294,#53295,
#53296),.UNSPECIFIED.,.F.,.F.,(4,3,3,3,3,3,3,3,3,4),(-53.9641979491412,
-52.9659810790005,-51.9666229454344,-50.9672648118684,-49.9679066783023,
-49.4682276115193,-48.9685485447363,-48.4688694779533,-47.9691904111702,
-47.6810126419616),.UNSPECIFIED.);
#1129=B_SPLINE_CURVE_WITH_KNOTS('',3,(#53297,#53298,#53299,#53300,#53301,
#53302,#53303,#53304,#53305,#53306,#53307,#53308,#53309,#53310,#53311,#53312,
#53313,#53314,#53315,#53316,#53317,#53318,#53319,#53320,#53321,#53322,#53323,
#53324,#53325,#53326,#53327,#53328,#53329,#53330,#53331,#53332,#53333,#53334,
#53335,#53336),.UNSPECIFIED.,.F.,.F.,(4,3,3,3,3,3,3,3,3,3,3,3,3,4),(44.4253578208116,
44.4714369436892,44.9711160104722,45.4707950772552,45.9704741440382,46.4701532108212,
46.9698322776042,47.4695113443873,47.9691904111703,48.4688694779533,48.9685485447363,
49.4682276115193,49.9679066783024,50.7085431279912),.UNSPECIFIED.);
#1130=B_SPLINE_CURVE_WITH_KNOTS('',3,(#53341,#53342,#53343,#53344,#53345,
#53346,#53347,#53348,#53349,#53350,#53351,#53352,#53353,#53354,#53355,#53356,
#53357,#53358,#53359,#53360,#53361,#53362),.UNSPECIFIED.,.F.,.F.,(4,3,3,
3,3,3,3,4),(-60.2473832563207,-59.9614880139628,-58.9621298803968,-57.9627717468307,
-56.9634136132647,-55.9640554796986,-54.9646973461326,-53.9641979491412),
 .UNSPECIFIED.);
#1131=B_SPLINE_CURVE_WITH_KNOTS('',3,(#53363,#53364,#53365,#53366,#53367,
#53368,#53369,#53370,#53371,#53372,#53373,#53374,#53375,#53376,#53377,#53378,
#53379,#53380,#53381,#53382,#53383,#53384,#53385,#53386,#53387),
 .UNSPECIFIED.,.F.,.F.,(4,3,3,3,3,3,3,3,4),(50.7085431279912,50.9672648118684,
51.9666229454345,52.9659810790005,53.9653392125666,54.9646973461326,55.9640554796987,
56.9634136132647,56.9917284351708),.UNSPECIFIED.);
#1132=B_SPLINE_CURVE_WITH_KNOTS('',3,(#53392,#53393,#53394,#53395,#53396,
#53397,#53398,#53399,#53400,#53401,#53402,#53403,#53404,#53405,#53406,#53407,
#53408,#53409,#53410,#53411,#53412,#53413),.UNSPECIFIED.,.F.,.F.,(4,3,3,
3,3,3,3,4),(-66.5305685635003,-65.9576368153591,-64.958278681793,-63.958920548227,
-62.9595624146609,-61.9602042810949,-60.9608461475288,-60.2473832563207),
 .UNSPECIFIED.);
#1133=B_SPLINE_CURVE_WITH_KNOTS('',3,(#53414,#53415,#53416,#53417,#53418,
#53419,#53420,#53421,#53422,#53423,#53424,#53425,#53426,#53427,#53428,#53429,
#53430,#53431,#53432,#53433,#53434,#53435),.UNSPECIFIED.,.F.,.F.,(4,3,3,
3,3,3,3,4),(56.9917284351708,57.9627717468308,58.9621298803968,59.9614880139629,
60.9608461475289,61.960204281095,62.959562414661,63.2749137423504),
 .UNSPECIFIED.);
#1134=B_SPLINE_CURVE_WITH_KNOTS('',3,(#53440,#53441,#53442,#53443,#53444,
#53445,#53446,#53447,#53448,#53449,#53450,#53451,#53452,#53453,#53454,#53455,
#53456,#53457,#53458,#53459,#53460,#53461),.UNSPECIFIED.,.F.,.F.,(4,3,3,
3,3,3,3,4),(-72.8137538706799,-71.9537856167554,-70.9544274831893,-69.9550693496233,
-68.9557112160572,-67.9563530824912,-66.9569949489251,-66.5305685635003),
 .UNSPECIFIED.);
#1135=B_SPLINE_CURVE_WITH_KNOTS('',3,(#53462,#53463,#53464,#53465,#53466,
#53467,#53468,#53469,#53470,#53471,#53472,#53473,#53474,#53475,#53476,#53477,
#53478,#53479,#53480,#53481,#53482,#53483),.UNSPECIFIED.,.F.,.F.,(4,3,3,
3,3,3,3,4),(63.2749137423504,63.958920548227,64.9582786817931,65.9576368153591,
66.9569949489252,67.9563530824912,68.9557112160573,69.55809904953),
 .UNSPECIFIED.);
#1136=B_SPLINE_CURVE_WITH_KNOTS('',3,(#53488,#53489,#53490,#53491,#53492,
#53493,#53494,#53495,#53496,#53497,#53498,#53499,#53500,#53501,#53502,#53503,
#53504,#53505,#53506,#53507,#53508,#53509,#53510,#53511,#53512),
 .UNSPECIFIED.,.F.,.F.,(4,3,3,3,3,3,3,3,4),(-79.0969391778595,-78.9492925517177,
-77.9499344181516,-76.9505762845856,-75.9512181510195,-74.9518600174535,
-73.9525018838875,-72.9531437503214,-72.8137538706799),.UNSPECIFIED.);
#1137=B_SPLINE_CURVE_WITH_KNOTS('',3,(#53513,#53514,#53515,#53516,#53517,
#53518,#53519,#53520,#53521,#53522,#53523,#53524,#53525,#53526,#53527,#53528,
#53529,#53530,#53531,#53532,#53533,#53534),.UNSPECIFIED.,.F.,.F.,(4,3,3,
3,3,3,3,4),(69.55809904953,69.9550693496233,70.9544274831893,71.9537856167554,
72.9531437503215,73.9525018838875,74.9518600174536,75.8412843567096),
 .UNSPECIFIED.);
#1138=B_SPLINE_CURVE_WITH_KNOTS('',3,(#53539,#53540,#53541,#53542,#53543,
#53544,#53545,#53546,#53547,#53548,#53549,#53550,#53551,#53552,#53553,#53554,
#53555,#53556,#53557,#53558,#53559,#53560),.UNSPECIFIED.,.F.,.F.,(4,3,3,
3,3,3,3,4),(-85.3801244850391,-84.945441353114,-83.9460832195479,-82.9467250859819,
-81.9473669524158,-80.9480088188498,-79.9486506852837,-79.0969391778595),
 .UNSPECIFIED.);
#1139=B_SPLINE_CURVE_WITH_KNOTS('',3,(#53561,#53562,#53563,#53564,#53565,
#53566,#53567,#53568,#53569,#53570,#53571,#53572,#53573,#53574,#53575,#53576,
#53577,#53578,#53579,#53580,#53581,#53582,#53583,#53584,#53585),
 .UNSPECIFIED.,.F.,.F.,(4,3,3,3,3,3,3,3,4),(75.8412843567096,75.9512181510196,
76.9505762845857,77.9499344181517,78.9492925517178,79.9486506852838,80.9480088188499,
81.9473669524159,82.1244696638892),.UNSPECIFIED.);
#1140=B_SPLINE_CURVE_WITH_KNOTS('',3,(#53590,#53591,#53592,#53593,#53594,
#53595,#53596,#53597,#53598,#53599,#53600,#53601,#53602,#53603,#53604,#53605,
#53606,#53607,#53608,#53609,#53610,#53611),.UNSPECIFIED.,.F.,.F.,(4,3,3,
3,3,3,3,4),(-91.6633097922187,-90.9415901545102,-89.9422320209442,-88.9428738873782,
-87.9435157538121,-86.944157620246,-85.94479948668,-85.3801244850391),
 .UNSPECIFIED.);
#1141=B_SPLINE_CURVE_WITH_KNOTS('',3,(#53612,#53613,#53614,#53615,#53616,
#53617,#53618,#53619,#53620,#53621,#53622,#53623,#53624,#53625,#53626,#53627,
#53628,#53629,#53630,#53631,#53632,#53633),.UNSPECIFIED.,.F.,.F.,(4,3,3,
3,3,3,3,4),(82.1244696638892,82.946725085982,83.946083219548,84.9454413531141,
85.9447994866801,86.9441576202461,87.9435157538122,88.4076549710687),
 .UNSPECIFIED.);
#1142=B_SPLINE_CURVE_WITH_KNOTS('',3,(#53638,#53639,#53640,#53641,#53642,
#53643,#53644,#53645,#53646,#53647,#53648,#53649,#53650,#53651,#53652,#53653,
#53654,#53655,#53656,#53657,#53658,#53659,#53660,#53661,#53662),
 .UNSPECIFIED.,.F.,.F.,(4,3,3,3,3,3,3,3,4),(-97.9464950993983,-97.9370970894726,
-96.9377389559065,-95.9383808223405,-94.9390226887744,-93.9396645552084,
-92.9403064216423,-91.9409482880763,-91.6633097922187),.UNSPECIFIED.);
#1143=B_SPLINE_CURVE_WITH_KNOTS('',3,(#53663,#53664,#53665,#53666,#53667,
#53668,#53669,#53670,#53671,#53672,#53673,#53674,#53675,#53676,#53677,#53678,
#53679,#53680,#53681,#53682,#53683,#53684),.UNSPECIFIED.,.F.,.F.,(4,3,3,
3,3,3,3,4),(88.4076549710687,88.9428738873782,89.9422320209442,90.9415901545103,
91.9409482880763,92.9403064216424,93.9396645552084,94.6908402782483),
 .UNSPECIFIED.);
#1144=B_SPLINE_CURVE_WITH_KNOTS('',3,(#53689,#53690,#53691,#53692,#53693,
#53694,#53695,#53696,#53697,#53698,#53699,#53700,#53701,#53702,#53703,#53704,
#53705,#53706,#53707,#53708,#53709,#53710),.UNSPECIFIED.,.F.,.F.,(4,3,3,
3,3,3,3,4),(-104.229680406578,-103.933245890869,-102.933887757303,-101.934529623737,
-100.935171490171,-99.9358133566047,-98.9364552230386,-97.9464950993983),
 .UNSPECIFIED.);
#1145=B_SPLINE_CURVE_WITH_KNOTS('',3,(#53711,#53712,#53713,#53714,#53715,
#53716,#53717,#53718,#53719,#53720,#53721,#53722,#53723,#53724,#53725,#53726,
#53727,#53728,#53729,#53730,#53731,#53732,#53733,#53734,#53735),
 .UNSPECIFIED.,.F.,.F.,(4,3,3,3,3,3,3,3,4),(94.6908402782483,94.9390226887745,
95.9383808223405,96.9377389559065,97.9370970894726,98.9364552230386,99.9358133566047,
100.935171490171,100.974025585428),.UNSPECIFIED.);
#1146=B_SPLINE_CURVE_WITH_KNOTS('',3,(#53740,#53741,#53742,#53743,#53744,
#53745,#53746,#53747,#53748,#53749,#53750,#53751,#53752,#53753,#53754,#53755,
#53756,#53757,#53758,#53759,#53760,#53761),.UNSPECIFIED.,.F.,.F.,(4,3,3,
3,3,3,3,4),(-110.512865713757,-109.929394692265,-108.930036558699,-107.930678425133,
-106.931320291567,-105.931962158001,-104.932604024435,-104.229680406578),
 .UNSPECIFIED.);
#1147=B_SPLINE_CURVE_WITH_KNOTS('',3,(#53762,#53763,#53764,#53765,#53766,
#53767,#53768,#53769,#53770,#53771,#53772,#53773,#53774,#53775,#53776,#53777,
#53778,#53779,#53780,#53781,#53782,#53783),.UNSPECIFIED.,.F.,.F.,(4,3,3,
3,3,3,3,4),(100.974025585428,101.934529623737,102.933887757303,103.933245890869,
104.932604024435,105.931962158001,106.931320291567,107.257210892608),
 .UNSPECIFIED.);
#1148=B_SPLINE_CURVE_WITH_KNOTS('',3,(#53788,#53789,#53790,#53791,#53792,
#53793,#53794,#53795,#53796,#53797,#53798,#53799,#53800,#53801,#53802,#53803,
#53804,#53805,#53806,#53807,#53808,#53809),.UNSPECIFIED.,.F.,.F.,(4,3,3,
3,3,3,3,4),(-116.796051020937,-115.925543493661,-114.926185360095,-113.926827226529,
-112.927469092963,-111.928110959397,-110.928752825831,-110.512865713757),
 .UNSPECIFIED.);
#1149=B_SPLINE_CURVE_WITH_KNOTS('',3,(#53810,#53811,#53812,#53813,#53814,
#53815,#53816,#53817,#53818,#53819,#53820,#53821,#53822,#53823,#53824,#53825,
#53826,#53827,#53828,#53829,#53830,#53831),.UNSPECIFIED.,.F.,.F.,(4,3,3,
3,3,3,3,4),(107.257210892608,107.930678425133,108.930036558699,109.929394692265,
110.928752825831,111.928110959397,112.927469092963,113.540396199787),
 .UNSPECIFIED.);
#1150=B_SPLINE_CURVE_WITH_KNOTS('',3,(#53836,#53837,#53838,#53839,#53840,
#53841,#53842,#53843,#53844,#53845,#53846,#53847,#53848,#53849,#53850,#53851,
#53852,#53853,#53854,#53855,#53856,#53857,#53858,#53859,#53860),
 .UNSPECIFIED.,.F.,.F.,(4,3,3,3,3,3,3,3,4),(-123.079236328117,-122.921050428624,
-121.921692295058,-120.922334161492,-119.922976027926,-118.92361789436,
-117.924259760793,-116.924901627227,-116.796051020937),.UNSPECIFIED.);
#1151=B_SPLINE_CURVE_WITH_KNOTS('',3,(#53861,#53862,#53863,#53864,#53865,
#53866,#53867,#53868,#53869,#53870,#53871,#53872,#53873,#53874,#53875,#53876,
#53877,#53878,#53879,#53880,#53881,#53882),.UNSPECIFIED.,.F.,.F.,(4,3,3,
3,3,3,3,4),(113.540396199787,113.926827226529,114.926185360095,115.925543493661,
116.924901627228,117.924259760794,118.92361789436,119.823581506967),
 .UNSPECIFIED.);
#1152=B_SPLINE_CURVE_WITH_KNOTS('',3,(#53887,#53888,#53889,#53890,#53891,
#53892,#53893,#53894,#53895,#53896,#53897,#53898,#53899,#53900,#53901,#53902,
#53903,#53904,#53905,#53906,#53907,#53908),.UNSPECIFIED.,.F.,.F.,(4,3,3,
3,3,3,3,4),(-129.362421635296,-128.91719923002,-127.917841096454,-126.918482962888,
-125.919124829322,-124.919766695756,-123.92040856219,-123.079236328117),
 .UNSPECIFIED.);
#1153=B_SPLINE_CURVE_WITH_KNOTS('',3,(#53909,#53910,#53911,#53912,#53913,
#53914,#53915,#53916,#53917,#53918,#53919,#53920,#53921,#53922,#53923,#53924,
#53925,#53926,#53927,#53928,#53929,#53930,#53931,#53932,#53933),
 .UNSPECIFIED.,.F.,.F.,(4,3,3,3,3,3,3,3,4),(119.823581506967,119.922976027926,
120.922334161492,121.921692295058,122.921050428624,123.92040856219,124.919766695756,
125.919124829322,126.106766814146),.UNSPECIFIED.);
#1154=B_SPLINE_CURVE_WITH_KNOTS('',3,(#53938,#53939,#53940,#53941,#53942,
#53943,#53944,#53945,#53946,#53947,#53948,#53949,#53950,#53951,#53952,#53953,
#53954,#53955,#53956,#53957,#53958,#53959),.UNSPECIFIED.,.F.,.F.,(4,3,3,
3,3,3,3,4),(-135.645606942476,-134.913348031416,-133.91398989785,-132.914631764284,
-131.915273630718,-130.915915497152,-129.916557363586,-129.362421635296),
 .UNSPECIFIED.);
#1155=B_SPLINE_CURVE_WITH_KNOTS('',3,(#53960,#53961,#53962,#53963,#53964,
#53965,#53966,#53967,#53968,#53969,#53970,#53971,#53972,#53973,#53974,#53975,
#53976,#53977,#53978,#53979,#53980,#53981),.UNSPECIFIED.,.F.,.F.,(4,3,3,
3,3,3,3,4),(126.106766814146,126.918482962888,127.917841096454,128.91719923002,
129.916557363586,130.915915497152,131.915273630718,132.389952121326),
 .UNSPECIFIED.);
#1156=B_SPLINE_CURVE_WITH_KNOTS('',3,(#53986,#53987,#53988,#53989,#53990,
#53991,#53992,#53993,#53994,#53995,#53996,#53997,#53998,#53999,#54000,#54001,
#54002,#54003,#54004,#54005,#54006,#54007,#54008,#54009,#54010),
 .UNSPECIFIED.,.F.,.F.,(4,3,3,3,3,3,3,3,4),(-141.928792249655,-141.908854966379,
-140.909496832813,-139.910138699247,-138.91078056568,-137.911422432114,
-136.912064298548,-135.912706164982,-135.645606942476),.UNSPECIFIED.);
#1157=B_SPLINE_CURVE_WITH_KNOTS('',3,(#54011,#54012,#54013,#54014,#54015,
#54016,#54017,#54018,#54019,#54020,#54021,#54022,#54023,#54024,#54025,#54026,
#54027,#54028,#54029,#54030,#54031,#54032),.UNSPECIFIED.,.F.,.F.,(4,3,3,
3,3,3,3,4),(132.389952121326,132.914631764284,133.91398989785,134.913348031416,
135.912706164982,136.912064298549,137.911422432115,138.673137428505),
 .UNSPECIFIED.);
#1158=B_SPLINE_CURVE_WITH_KNOTS('',3,(#54037,#54038,#54039,#54040,#54041,
#54042,#54043,#54044,#54045,#54046,#54047,#54048,#54049,#54050,#54051,#54052,
#54053,#54054,#54055,#54056,#54057,#54058),.UNSPECIFIED.,.F.,.F.,(4,3,3,
3,3,3,3,4),(-148.211977556835,-147.905003767775,-146.905645634209,-145.906287500643,
-144.906929367077,-143.907571233511,-142.908213099945,-141.928792249655),
 .UNSPECIFIED.);
#1159=B_SPLINE_CURVE_WITH_KNOTS('',3,(#54059,#54060,#54061,#54062,#54063,
#54064,#54065,#54066,#54067,#54068,#54069,#54070,#54071,#54072,#54073,#54074,
#54075,#54076,#54077,#54078,#54079,#54080,#54081,#54082,#54083),
 .UNSPECIFIED.,.F.,.F.,(4,3,3,3,3,3,3,3,4),(138.673137428505,138.910780565681,
139.910138699247,140.909496832813,141.908854966379,142.908213099945,143.907571233511,
144.906929367077,144.956322735685),.UNSPECIFIED.);
#1160=B_SPLINE_CURVE_WITH_KNOTS('',3,(#54088,#54089,#54090,#54091,#54092,
#54093,#54094,#54095,#54096,#54097,#54098,#54099,#54100,#54101,#54102,#54103,
#54104,#54105,#54106,#54107,#54108,#54109),.UNSPECIFIED.,.F.,.F.,(4,3,3,
3,3,3,3,4),(-154.495162864015,-153.901152569171,-152.901794435605,-151.902436302039,
-150.903078168473,-149.903720034907,-148.904361901341,-148.211977556835),
 .UNSPECIFIED.);
#1161=B_SPLINE_CURVE_WITH_KNOTS('',3,(#54110,#54111,#54112,#54113,#54114,
#54115,#54116,#54117,#54118,#54119,#54120,#54121,#54122,#54123,#54124,#54125,
#54126,#54127,#54128,#54129,#54130,#54131),.UNSPECIFIED.,.F.,.F.,(4,3,3,
3,3,3,3,4),(144.956322735685,145.906287500643,146.905645634209,147.905003767775,
148.904361901341,149.903720034907,150.903078168473,151.239508042865),
 .UNSPECIFIED.);
#1162=B_SPLINE_CURVE_WITH_KNOTS('',3,(#54136,#54137,#54138,#54139,#54140,
#54141,#54142,#54143,#54144,#54145,#54146,#54147,#54148,#54149,#54150,#54151,
#54152,#54153,#54154,#54155,#54156,#54157),.UNSPECIFIED.,.F.,.F.,(4,3,3,
3,3,3,3,4),(-160.778348171194,-159.897301370567,-158.897943237001,-157.898585103435,
-156.899226969869,-155.899868836303,-154.900510702737,-154.495162864015),
 .UNSPECIFIED.);
#1163=B_SPLINE_CURVE_WITH_KNOTS('',3,(#54158,#54159,#54160,#54161,#54162,
#54163,#54164,#54165,#54166,#54167,#54168,#54169,#54170,#54171,#54172,#54173,
#54174,#54175,#54176,#54177,#54178,#54179),.UNSPECIFIED.,.F.,.F.,(4,3,3,
3,3,3,3,4),(151.239508042865,151.902436302039,152.901794435605,153.901152569171,
154.900510702737,155.899868836303,156.899226969869,157.522693350044),
 .UNSPECIFIED.);
#1164=B_SPLINE_CURVE_WITH_KNOTS('',3,(#54184,#54185,#54186,#54187,#54188,
#54189,#54190,#54191,#54192,#54193,#54194,#54195,#54196,#54197,#54198,#54199,
#54200,#54201,#54202,#54203,#54204,#54205,#54206,#54207,#54208),
 .UNSPECIFIED.,.F.,.F.,(4,3,3,3,3,3,3,3,4),(-167.061533478374,-166.89280830553,
-165.893450171964,-164.894092038398,-163.894733904832,-162.895375771266,
-161.8960176377,-160.896659504134,-160.778348171194),.UNSPECIFIED.);
#1165=B_SPLINE_CURVE_WITH_KNOTS('',3,(#54209,#54210,#54211,#54212,#54213,
#54214,#54215,#54216,#54217,#54218,#54219,#54220,#54221,#54222,#54223,#54224,
#54225,#54226,#54227,#54228,#54229,#54230),.UNSPECIFIED.,.F.,.F.,(4,3,3,
3,3,3,3,4),(157.522693350044,157.898585103435,158.897943237002,159.897301370568,
160.896659504134,161.8960176377,162.895375771266,163.805878657224),
 .UNSPECIFIED.);
#1166=B_SPLINE_CURVE_WITH_KNOTS('',3,(#54235,#54236,#54237,#54238,#54239,
#54240,#54241,#54242,#54243,#54244,#54245,#54246,#54247,#54248,#54249,#54250,
#54251,#54252,#54253,#54254,#54255,#54256),.UNSPECIFIED.,.F.,.F.,(4,3,3,
3,3,3,3,4),(-173.344718785553,-172.888957106926,-171.88959897336,-170.890240839794,
-169.890882706228,-168.891524572662,-167.892166439096,-167.061533478374),
 .UNSPECIFIED.);
#1167=B_SPLINE_CURVE_WITH_KNOTS('',3,(#54257,#54258,#54259,#54260,#54261,
#54262,#54263,#54264,#54265,#54266,#54267,#54268,#54269,#54270,#54271,#54272,
#54273,#54274,#54275,#54276,#54277,#54278,#54279,#54280,#54281),
 .UNSPECIFIED.,.F.,.F.,(4,3,3,3,3,3,3,3,4),(163.805878657224,163.894733904832,
164.894092038398,165.893450171964,166.89280830553,167.892166439096,168.891524572662,
169.890882706228,170.089063964403),.UNSPECIFIED.);
#1168=B_SPLINE_CURVE_WITH_KNOTS('',3,(#54286,#54287,#54288,#54289,#54290,
#54291,#54292,#54293,#54294,#54295,#54296,#54297,#54298,#54299,#54300,#54301,
#54302,#54303,#54304,#54305,#54306,#54307),.UNSPECIFIED.,.F.,.F.,(4,3,3,
3,3,3,3,4),(-179.627904092733,-178.885105908322,-177.885747774756,-176.88638964119,
-175.887031507624,-174.887673374058,-173.888315240492,-173.344718785553),
 .UNSPECIFIED.);
#1169=B_SPLINE_CURVE_WITH_KNOTS('',3,(#54308,#54309,#54310,#54311,#54312,
#54313,#54314,#54315,#54316,#54317,#54318,#54319,#54320,#54321,#54322,#54323,
#54324,#54325,#54326,#54327,#54328,#54329),.UNSPECIFIED.,.F.,.F.,(4,3,3,
3,3,3,3,4),(170.089063964403,170.890240839794,171.88959897336,172.888957106926,
173.888315240492,174.887673374058,175.887031507624,176.372249271583),
 .UNSPECIFIED.);
#1170=B_SPLINE_CURVE_WITH_KNOTS('',3,(#54334,#54335,#54336,#54337,#54338,
#54339,#54340,#54341,#54342,#54343,#54344,#54345,#54346,#54347,#54348,#54349,
#54350,#54351,#54352,#54353,#54354,#54355,#54356,#54357,#54358),
 .UNSPECIFIED.,.F.,.F.,(4,3,3,3,3,3,3,3,4),(-185.911089399912,-185.880612843285,
-184.881254709719,-183.881896576153,-182.882538442587,-181.88318030902,
-180.883822175454,-179.884464041888,-179.627904092733),.UNSPECIFIED.);
#1171=B_SPLINE_CURVE_WITH_KNOTS('',3,(#54359,#54360,#54361,#54362,#54363,
#54364,#54365,#54366,#54367,#54368,#54369,#54370,#54371,#54372,#54373,#54374,
#54375,#54376,#54377,#54378,#54379,#54380),.UNSPECIFIED.,.F.,.F.,(4,3,3,
3,3,3,3,4),(176.372249271583,176.88638964119,177.885747774756,178.885105908322,
179.884464041889,180.883822175455,181.883180309021,182.655434578762),
 .UNSPECIFIED.);
#1172=B_SPLINE_CURVE_WITH_KNOTS('',3,(#54385,#54386,#54387,#54388,#54389,
#54390,#54391,#54392,#54393,#54394,#54395,#54396,#54397,#54398,#54399,#54400,
#54401,#54402,#54403,#54404,#54405,#54406),.UNSPECIFIED.,.F.,.F.,(4,3,3,
3,3,3,3,4),(-192.194274707092,-191.876761644681,-190.877403511115,-189.878045377549,
-188.878687243983,-187.879329110417,-186.879970976851,-185.911089399912),
 .UNSPECIFIED.);
#1173=B_SPLINE_CURVE_WITH_KNOTS('',3,(#54407,#54408,#54409,#54410,#54411,
#54412,#54413,#54414,#54415,#54416,#54417,#54418,#54419,#54420,#54421,#54422,
#54423,#54424,#54425,#54426,#54427,#54428,#54429,#54430,#54431),
 .UNSPECIFIED.,.F.,.F.,(4,3,3,3,3,3,3,3,4),(182.655434578762,182.882538442587,
183.881896576153,184.881254709719,185.880612843285,186.879970976851,187.879329110417,
188.878687243983,188.938619885942),.UNSPECIFIED.);
#1174=B_SPLINE_CURVE_WITH_KNOTS('',3,(#54436,#54437,#54438,#54439,#54440,
#54441,#54442,#54443,#54444,#54445,#54446,#54447,#54448,#54449,#54450,#54451,
#54452,#54453,#54454,#54455,#54456,#54457),.UNSPECIFIED.,.F.,.F.,(4,3,3,
3,3,3,3,4),(-198.477460014271,-197.872910446077,-196.873552312511,-195.874194178945,
-194.874836045379,-193.875477911813,-192.876119778247,-192.194274707092),
 .UNSPECIFIED.);
#1175=B_SPLINE_CURVE_WITH_KNOTS('',3,(#54458,#54459,#54460,#54461,#54462,
#54463,#54464,#54465,#54466,#54467,#54468,#54469,#54470,#54471,#54472,#54473,
#54474,#54475,#54476,#54477,#54478,#54479),.UNSPECIFIED.,.F.,.F.,(4,3,3,
3,3,3,3,4),(188.938619885942,189.878045377549,190.877403511115,191.876761644681,
192.876119778247,193.875477911813,194.874836045379,195.221805193122),
 .UNSPECIFIED.);
#1176=B_SPLINE_CURVE_WITH_KNOTS('',3,(#54484,#54485,#54486,#54487,#54488,
#54489,#54490,#54491,#54492,#54493,#54494,#54495,#54496,#54497,#54498,#54499,
#54500,#54501,#54502,#54503,#54504,#54505),.UNSPECIFIED.,.F.,.F.,(4,3,3,
3,3,3,3,4),(-204.760645321451,-203.869059247473,-202.869701113907,-201.870342980341,
-200.870984846775,-199.871626713209,-198.872268579643,-198.477460014271),
 .UNSPECIFIED.);
#1177=B_SPLINE_CURVE_WITH_KNOTS('',3,(#54506,#54507,#54508,#54509,#54510,
#54511,#54512,#54513,#54514,#54515,#54516,#54517,#54518,#54519,#54520,#54521,
#54522,#54523,#54524,#54525,#54526,#54527),.UNSPECIFIED.,.F.,.F.,(4,3,3,
3,3,3,3,4),(195.221805193122,195.874194178945,196.873552312511,197.872910446077,
198.872268579643,199.871626713209,200.870984846776,201.504990500301),
 .UNSPECIFIED.);
#1178=B_SPLINE_CURVE_WITH_KNOTS('',3,(#54532,#54533,#54534,#54535,#54536,
#54537,#54538,#54539,#54540,#54541,#54542,#54543,#54544,#54545,#54546,#54547,
#54548,#54549,#54550,#54551,#54552,#54553,#54554,#54555,#54556),
 .UNSPECIFIED.,.F.,.F.,(4,3,3,3,3,3,3,3,4),(-211.043830628631,-210.864566182436,
-209.86520804887,-208.865849915304,-207.866491781738,-206.867133648172,
-205.867775514606,-204.86841738104,-204.760645321451),.UNSPECIFIED.);
#1179=B_SPLINE_CURVE_WITH_KNOTS('',3,(#54557,#54558,#54559,#54560,#54561,
#54562,#54563,#54564,#54565,#54566,#54567,#54568,#54569,#54570,#54571,#54572,
#54573,#54574,#54575,#54576,#54577,#54578),.UNSPECIFIED.,.F.,.F.,(4,3,3,
3,3,3,3,4),(201.504990500301,201.870342980342,202.869701113908,203.869059247474,
204.86841738104,205.867775514606,206.867133648172,207.788175807481),
 .UNSPECIFIED.);
#1180=B_SPLINE_CURVE_WITH_KNOTS('',3,(#54583,#54584,#54585,#54586,#54587,
#54588,#54589,#54590,#54591,#54592,#54593,#54594,#54595,#54596,#54597,#54598,
#54599,#54600,#54601,#54602,#54603,#54604),.UNSPECIFIED.,.F.,.F.,(4,3,3,
3,3,3,3,4),(-217.32701593581,-216.860714983832,-215.861356850266,-214.8619987167,
-213.862640583134,-212.863282449568,-211.863924316002,-211.043830628631),
 .UNSPECIFIED.);
#1181=B_SPLINE_CURVE_WITH_KNOTS('',3,(#54605,#54606,#54607,#54608,#54609,
#54610,#54611,#54612,#54613,#54614,#54615,#54616,#54617,#54618,#54619,#54620,
#54621,#54622,#54623,#54624,#54625,#54626,#54627,#54628,#54629),
 .UNSPECIFIED.,.F.,.F.,(4,3,3,3,3,3,3,3,4),(207.788175807481,207.866491781738,
208.865849915304,209.86520804887,210.864566182436,211.863924316002,212.863282449568,
213.862640583134,214.07136111466),.UNSPECIFIED.);
#1182=B_SPLINE_CURVE_WITH_KNOTS('',3,(#54634,#54635,#54636,#54637,#54638,
#54639,#54640,#54641,#54642,#54643,#54644,#54645,#54646,#54647,#54648,#54649,
#54650,#54651,#54652,#54653,#54654,#54655),.UNSPECIFIED.,.F.,.F.,(4,3,3,
3,3,3,3,4),(-223.61020124299,-222.856863785228,-221.857505651662,-220.858147518096,
-219.85878938453,-218.859431250964,-217.860073117398,-217.32701593581),
 .UNSPECIFIED.);
#1183=B_SPLINE_CURVE_WITH_KNOTS('',3,(#54656,#54657,#54658,#54659,#54660,
#54661,#54662,#54663,#54664,#54665,#54666,#54667,#54668,#54669,#54670,#54671,
#54672,#54673,#54674,#54675,#54676,#54677),.UNSPECIFIED.,.F.,.F.,(4,3,3,
3,3,3,3,4),(214.07136111466,214.8619987167,215.861356850266,216.860714983832,
217.860073117398,218.859431250964,219.85878938453,220.35454642184),
 .UNSPECIFIED.);
#1184=B_SPLINE_CURVE_WITH_KNOTS('',3,(#54682,#54683,#54684,#54685,#54686,
#54687,#54688,#54689,#54690,#54691,#54692,#54693,#54694,#54695,#54696,#54697,
#54698,#54699,#54700,#54701,#54702,#54703,#54704,#54705,#54706),
 .UNSPECIFIED.,.F.,.F.,(4,3,3,3,3,3,3,3,4),(-229.893386550169,-229.852370720191,
-228.853012586625,-227.853654453059,-226.854296319493,-225.854938185927,
-224.85558005236,-223.856221918794,-223.61020124299),.UNSPECIFIED.);
#1185=B_SPLINE_CURVE_WITH_KNOTS('',3,(#54707,#54708,#54709,#54710,#54711,
#54712,#54713,#54714,#54715,#54716,#54717,#54718,#54719,#54720,#54721,#54722,
#54723,#54724,#54725,#54726,#54727,#54728),.UNSPECIFIED.,.F.,.F.,(4,3,3,
3,3,3,3,4),(220.35454642184,220.858147518096,221.857505651663,222.856863785229,
223.856221918795,224.855580052361,225.854938185927,226.637731729019),
 .UNSPECIFIED.);
#1186=B_SPLINE_CURVE_WITH_KNOTS('',3,(#54733,#54734,#54735,#54736,#54737,
#54738,#54739,#54740,#54741,#54742,#54743,#54744,#54745,#54746,#54747,#54748,
#54749,#54750,#54751,#54752,#54753,#54754),.UNSPECIFIED.,.F.,.F.,(4,3,3,
3,3,3,3,4),(-236.176571857349,-235.848519521587,-234.849161388021,-233.849803254455,
-232.850445120889,-231.851086987323,-230.851728853757,-229.893386550169),
 .UNSPECIFIED.);
#1187=B_SPLINE_CURVE_WITH_KNOTS('',3,(#54755,#54756,#54757,#54758,#54759,
#54760,#54761,#54762,#54763,#54764,#54765,#54766,#54767,#54768,#54769,#54770,
#54771,#54772,#54773,#54774,#54775,#54776,#54777,#54778,#54779),
 .UNSPECIFIED.,.F.,.F.,(4,3,3,3,3,3,3,3,4),(226.637731729019,226.854296319493,
227.853654453059,228.853012586625,229.852370720191,230.851728853757,231.851086987323,
232.850445120889,232.920917036199),.UNSPECIFIED.);
#1188=B_SPLINE_CURVE_WITH_KNOTS('',3,(#54784,#54785,#54786,#54787,#54788,
#54789,#54790,#54791,#54792,#54793,#54794,#54795,#54796,#54797,#54798,#54799,
#54800,#54801,#54802,#54803,#54804,#54805),.UNSPECIFIED.,.F.,.F.,(4,3,3,
3,3,3,3,4),(-242.459757164528,-241.844668322983,-240.845310189417,-239.845952055851,
-238.846593922285,-237.847235788719,-236.847877655153,-236.176571857349),
 .UNSPECIFIED.);
#1189=B_SPLINE_CURVE_WITH_KNOTS('',3,(#54806,#54807,#54808,#54809,#54810,
#54811,#54812,#54813,#54814,#54815,#54816,#54817,#54818,#54819,#54820,#54821,
#54822,#54823,#54824,#54825,#54826,#54827),.UNSPECIFIED.,.F.,.F.,(4,3,3,
3,3,3,3,4),(232.920917036199,233.849803254455,234.849161388021,235.848519521587,
236.847877655153,237.847235788719,238.846593922285,239.204102343378),
 .UNSPECIFIED.);
#1190=B_SPLINE_CURVE_WITH_KNOTS('',3,(#54832,#54833,#54834,#54835,#54836,
#54837,#54838,#54839,#54840,#54841,#54842,#54843,#54844,#54845,#54846,#54847,
#54848,#54849,#54850,#54851,#54852,#54853),.UNSPECIFIED.,.F.,.F.,(4,3,3,
3,3,3,3,4),(-248.742942471708,-247.84081712438,-246.841458990814,-245.842100857247,
-244.842742723681,-243.843384590115,-242.844026456549,-242.459757164528),
 .UNSPECIFIED.);
#1191=B_SPLINE_CURVE_WITH_KNOTS('',3,(#54854,#54855,#54856,#54857,#54858,
#54859,#54860,#54861,#54862,#54863,#54864,#54865,#54866,#54867,#54868,#54869,
#54870,#54871,#54872,#54873,#54874,#54875),.UNSPECIFIED.,.F.,.F.,(4,3,3,
3,3,3,3,4),(239.204102343378,239.845952055851,240.845310189417,241.844668322983,
242.84402645655,243.843384590116,244.842742723682,245.487287650558),
 .UNSPECIFIED.);
#1192=B_SPLINE_CURVE_WITH_KNOTS('',3,(#54880,#54881,#54882,#54883,#54884,
#54885,#54886,#54887,#54888,#54889,#54890,#54891,#54892,#54893,#54894,#54895,
#54896,#54897,#54898,#54899,#54900,#54901,#54902,#54903,#54904),
 .UNSPECIFIED.,.F.,.F.,(4,3,3,3,3,3,3,3,4),(-255.026127778888,-254.836324059342,
-253.836965925776,-252.83760779221,-251.838249658644,-250.838891525078,
-249.839533391512,-248.840175257946,-248.742942471708),.UNSPECIFIED.);
#1193=B_SPLINE_CURVE_WITH_KNOTS('',3,(#54905,#54906,#54907,#54908,#54909,
#54910,#54911,#54912,#54913,#54914,#54915,#54916,#54917,#54918,#54919,#54920,
#54921,#54922,#54923,#54924,#54925,#54926),.UNSPECIFIED.,.F.,.F.,(4,3,3,
3,3,3,3,4),(245.487287650558,245.842100857248,246.841458990814,247.84081712438,
248.840175257946,249.839533391512,250.838891525078,251.770472957738),
 .UNSPECIFIED.);
#1194=B_SPLINE_CURVE_WITH_KNOTS('',3,(#54931,#54932,#54933,#54934,#54935,
#54936,#54937,#54938,#54939,#54940,#54941,#54942,#54943,#54944,#54945,#54946,
#54947,#54948,#54949,#54950,#54951,#54952),.UNSPECIFIED.,.F.,.F.,(4,3,3,
3,3,3,3,4),(-261.309313086067,-260.832472860738,-259.833114727172,-258.833756593606,
-257.83439846004,-256.835040326474,-255.835682192908,-255.026127778888),
 .UNSPECIFIED.);
#1195=B_SPLINE_CURVE_WITH_KNOTS('',3,(#54953,#54954,#54955,#54956,#54957,
#54958,#54959,#54960,#54961,#54962,#54963,#54964,#54965,#54966,#54967,#54968,
#54969,#54970,#54971,#54972,#54973,#54974,#54975,#54976,#54977),
 .UNSPECIFIED.,.F.,.F.,(4,3,3,3,3,3,3,3,4),(251.770472957738,251.838249658644,
252.83760779221,253.836965925776,254.836324059342,255.835682192908,256.835040326474,
257.83439846004,258.053658264917),.UNSPECIFIED.);
#1196=B_SPLINE_CURVE_WITH_KNOTS('',3,(#54982,#54983,#54984,#54985,#54986,
#54987,#54988,#54989,#54990,#54991,#54992,#54993,#54994,#54995,#54996,#54997,
#54998,#54999,#55000,#55001,#55002,#55003),.UNSPECIFIED.,.F.,.F.,(4,3,3,
3,3,3,3,4),(-267.592498393247,-266.828621662134,-265.829263528568,-264.829905395002,
-263.830547261436,-262.83118912787,-261.831830994304,-261.309313086067),
 .UNSPECIFIED.);
#1197=B_SPLINE_CURVE_WITH_KNOTS('',3,(#55004,#55005,#55006,#55007,#55008,
#55009,#55010,#55011,#55012,#55013,#55014,#55015,#55016,#55017,#55018,#55019,
#55020,#55021,#55022,#55023,#55024,#55025),.UNSPECIFIED.,.F.,.F.,(4,3,3,
3,3,3,3,4),(258.053658264917,258.833756593606,259.833114727172,260.832472860738,
261.831830994304,262.83118912787,263.830547261436,264.336843572097),
 .UNSPECIFIED.);
#1198=B_SPLINE_CURVE_WITH_KNOTS('',3,(#55030,#55031,#55032,#55033,#55034,
#55035,#55036,#55037,#55038,#55039,#55040,#55041,#55042,#55043,#55044,#55045,
#55046,#55047,#55048,#55049,#55050,#55051,#55052,#55053,#55054),
 .UNSPECIFIED.,.F.,.F.,(4,3,3,3,3,3,3,3,4),(-273.875683700426,-273.824128597097,
-272.824770463531,-271.825412329965,-270.826054196399,-269.826696062833,
-268.827337929266,-267.8279797957,-267.592498393247),.UNSPECIFIED.);
#1199=B_SPLINE_CURVE_WITH_KNOTS('',3,(#55055,#55056,#55057,#55058,#55059,
#55060,#55061,#55062,#55063,#55064,#55065,#55066,#55067,#55068,#55069,#55070,
#55071,#55072,#55073,#55074,#55075,#55076),.UNSPECIFIED.,.F.,.F.,(4,3,3,
3,3,3,3,4),(264.336843572097,264.829905395003,265.829263528569,266.828621662135,
267.827979795701,268.827337929267,269.826696062833,270.620028879276),
 .UNSPECIFIED.);
#1200=B_SPLINE_CURVE_WITH_KNOTS('',3,(#55081,#55082,#55083,#55084,#55085,
#55086,#55087,#55088,#55089,#55090,#55091,#55092,#55093,#55094,#55095,#55096,
#55097,#55098,#55099,#55100,#55101,#55102),.UNSPECIFIED.,.F.,.F.,(4,3,3,
3,3,3,3,4),(-280.158869007606,-279.820277398493,-278.820919264927,-277.821561131361,
-276.822202997795,-275.822844864229,-274.823486730663,-273.875683700426),
 .UNSPECIFIED.);
#1201=B_SPLINE_CURVE_WITH_KNOTS('',3,(#55103,#55104,#55105,#55106,#55107,
#55108,#55109,#55110,#55111,#55112,#55113,#55114,#55115,#55116,#55117,#55118,
#55119,#55120,#55121,#55122,#55123,#55124,#55125,#55126,#55127),
 .UNSPECIFIED.,.F.,.F.,(4,3,3,3,3,3,3,3,4),(270.620028879276,270.826054196399,
271.825412329965,272.824770463531,273.824128597097,274.823486730663,275.822844864229,
276.822202997795,276.903214186456),.UNSPECIFIED.);
#1202=B_SPLINE_CURVE_WITH_KNOTS('',3,(#55132,#55133,#55134,#55135,#55136,
#55137,#55138,#55139,#55140,#55141,#55142,#55143,#55144,#55145,#55146,#55147,
#55148,#55149,#55150,#55151,#55152,#55153),.UNSPECIFIED.,.F.,.F.,(4,3,3,
3,3,3,3,4),(-286.442054314785,-285.816426199889,-284.817068066323,-283.817709932757,
-282.818351799191,-281.818993665625,-280.819635532059,-280.158869007606),
 .UNSPECIFIED.);
#1203=B_SPLINE_CURVE_WITH_KNOTS('',3,(#55154,#55155,#55156,#55157,#55158,
#55159,#55160,#55161,#55162,#55163,#55164,#55165,#55166,#55167,#55168,#55169,
#55170,#55171,#55172,#55173,#55174,#55175),.UNSPECIFIED.,.F.,.F.,(4,3,3,
3,3,3,3,4),(276.903214186456,277.821561131361,278.820919264927,279.820277398493,
280.819635532059,281.818993665625,282.818351799191,283.186399493635),
 .UNSPECIFIED.);
#1204=B_SPLINE_CURVE_WITH_KNOTS('',3,(#55180,#55181,#55182,#55183,#55184,
#55185,#55186,#55187,#55188,#55189,#55190,#55191,#55192,#55193,#55194,#55195,
#55196,#55197,#55198,#55199,#55200,#55201),.UNSPECIFIED.,.F.,.F.,(4,3,3,
3,3,3,3,4),(-292.725239621965,-291.812575001286,-290.81321686772,-289.813858734153,
-288.814500600587,-287.815142467021,-286.815784333455,-286.442054314785),
 .UNSPECIFIED.);
#1205=B_SPLINE_CURVE_WITH_KNOTS('',3,(#55202,#55203,#55204,#55205,#55206,
#55207,#55208,#55209,#55210,#55211,#55212,#55213,#55214,#55215,#55216,#55217,
#55218,#55219,#55220,#55221,#55222,#55223),.UNSPECIFIED.,.F.,.F.,(4,3,3,
3,3,3,3,4),(283.186399493635,283.817709932757,284.817068066323,285.81642619989,
286.815784333456,287.815142467022,288.814500600588,289.469584800815),
 .UNSPECIFIED.);
#1206=B_SPLINE_CURVE_WITH_KNOTS('',3,(#55228,#55229,#55230,#55231,#55232,
#55233,#55234,#55235,#55236,#55237,#55238,#55239,#55240,#55241,#55242,#55243,
#55244,#55245,#55246,#55247,#55248,#55249,#55250,#55251,#55252),
 .UNSPECIFIED.,.F.,.F.,(4,3,3,3,3,3,3,3,4),(-299.008424929145,-298.808081936248,
-297.808723802682,-296.809365669116,-295.81000753555,-294.810649401984,
-293.811291268418,-292.811933134852,-292.725239621965),.UNSPECIFIED.);
#1207=B_SPLINE_CURVE_WITH_KNOTS('',3,(#55253,#55254,#55255,#55256,#55257,
#55258,#55259,#55260,#55261,#55262,#55263,#55264,#55265,#55266,#55267,#55268,
#55269,#55270,#55271,#55272,#55273,#55274),.UNSPECIFIED.,.F.,.F.,(4,3,3,
3,3,3,3,4),(289.469584800815,289.813858734154,290.81321686772,291.812575001286,
292.811933134852,293.811291268418,294.810649401984,295.752770107995),
 .UNSPECIFIED.);
#1208=B_SPLINE_CURVE_WITH_KNOTS('',3,(#55279,#55280,#55281,#55282,#55283,
#55284,#55285,#55286,#55287,#55288,#55289,#55290,#55291,#55292,#55293,#55294,
#55295,#55296,#55297,#55298,#55299,#55300),.UNSPECIFIED.,.F.,.F.,(4,3,3,
3,3,3,3,4),(-305.291610236324,-304.804230737644,-303.804872604078,-302.805514470512,
-301.806156336946,-300.80679820338,-299.807440069814,-299.008424929145),
 .UNSPECIFIED.);
#1209=B_SPLINE_CURVE_WITH_KNOTS('',3,(#55301,#55302,#55303,#55304,#55305,
#55306,#55307,#55308,#55309,#55310,#55311,#55312,#55313,#55314,#55315,#55316,
#55317,#55318,#55319,#55320,#55321,#55322,#55323,#55324,#55325),
 .UNSPECIFIED.,.F.,.F.,(4,3,3,3,3,3,3,3,4),(295.752770107995,295.81000753555,
296.809365669116,297.808723802682,298.808081936248,299.807440069814,300.80679820338,
301.806156336946,302.035955415174),.UNSPECIFIED.);
#1210=B_SPLINE_CURVE_WITH_KNOTS('',3,(#55330,#55331,#55332,#55333,#55334,
#55335,#55336,#55337,#55338,#55339,#55340,#55341,#55342,#55343,#55344,#55345,
#55346,#55347,#55348,#55349,#55350,#55351),.UNSPECIFIED.,.F.,.F.,(4,3,3,
3,3,3,3,4),(-311.574795543504,-310.80037953904,-309.801021405475,-308.801663271908,
-307.802305138342,-306.802947004776,-305.80358887121,-305.291610236324),
 .UNSPECIFIED.);
#1211=B_SPLINE_CURVE_WITH_KNOTS('',3,(#55352,#55353,#55354,#55355,#55356,
#55357,#55358,#55359,#55360,#55361,#55362,#55363,#55364,#55365,#55366,#55367,
#55368,#55369,#55370,#55371,#55372,#55373),.UNSPECIFIED.,.F.,.F.,(4,3,3,
3,3,3,3,4),(302.035955415174,302.805514470512,303.804872604078,304.804230737644,
305.80358887121,306.802947004777,307.802305138343,308.319140722354),
 .UNSPECIFIED.);
#1212=B_SPLINE_CURVE_WITH_KNOTS('',3,(#55378,#55379,#55380,#55381,#55382,
#55383,#55384,#55385,#55386,#55387,#55388,#55389,#55390,#55391,#55392,#55393,
#55394,#55395,#55396,#55397,#55398,#55399,#55400,#55401,#55402),
 .UNSPECIFIED.,.F.,.F.,(4,3,3,3,3,3,3,3,4),(-317.857980850683,-317.795886474003,
-316.796528340437,-315.797170206871,-314.797812073305,-313.798453939739,
-312.799095806173,-311.799737672607,-311.574795543504),.UNSPECIFIED.);
#1213=B_SPLINE_CURVE_WITH_KNOTS('',3,(#55403,#55404,#55405,#55406,#55407,
#55408,#55409,#55410,#55411,#55412,#55413,#55414,#55415,#55416,#55417,#55418,
#55419,#55420,#55421,#55422,#55423,#55424),.UNSPECIFIED.,.F.,.F.,(4,3,3,
3,3,3,3,4),(308.319140722354,308.801663271909,309.801021405475,310.800379539041,
311.799737672607,312.799095806173,313.798453939739,314.602326029533),
 .UNSPECIFIED.);
#1214=B_SPLINE_CURVE_WITH_KNOTS('',3,(#55429,#55430,#55431,#55432,#55433,
#55434,#55435,#55436,#55437,#55438,#55439,#55440,#55441,#55442,#55443,#55444,
#55445,#55446,#55447,#55448,#55449,#55450),.UNSPECIFIED.,.F.,.F.,(4,3,3,
3,3,3,3,4),(-324.141166157863,-323.792035275399,-322.792677141833,-321.793319008267,
-320.793960874701,-319.794602741135,-318.795244607569,-317.857980850683),
 .UNSPECIFIED.);
#1215=B_SPLINE_CURVE_WITH_KNOTS('',3,(#55451,#55452,#55453,#55454,#55455,
#55456,#55457,#55458,#55459,#55460,#55461,#55462,#55463,#55464,#55465,#55466,
#55467,#55468,#55469,#55470,#55471,#55472,#55473,#55474,#55475),
 .UNSPECIFIED.,.F.,.F.,(4,3,3,3,3,3,3,3,4),(314.602326029533,314.797812073305,
315.797170206871,316.796528340437,317.795886474003,318.795244607569,319.794602741135,
320.793960874701,320.885511336713),.UNSPECIFIED.);
#1216=B_SPLINE_CURVE_WITH_KNOTS('',3,(#55480,#55481,#55482,#55483,#55484,
#55485,#55486,#55487,#55488,#55489,#55490,#55491,#55492,#55493,#55494,#55495,
#55496,#55497,#55498,#55499,#55500,#55501),.UNSPECIFIED.,.F.,.F.,(4,3,3,
3,3,3,3,4),(-330.424351465042,-329.788184076795,-328.788825943229,-327.789467809663,
-326.790109676097,-325.790751542531,-324.791393408965,-324.141166157863),
 .UNSPECIFIED.);
#1217=B_SPLINE_CURVE_WITH_KNOTS('',3,(#55502,#55503,#55504,#55505,#55506,
#55507,#55508,#55509,#55510,#55511,#55512,#55513,#55514,#55515,#55516,#55517,
#55518,#55519,#55520,#55521,#55522,#55523),.UNSPECIFIED.,.F.,.F.,(4,3,3,
3,3,3,3,4),(320.885511336713,321.793319008267,322.792677141833,323.792035275399,
324.791393408965,325.790751542531,326.790109676097,327.168696643892),
 .UNSPECIFIED.);
#1218=B_SPLINE_CURVE_WITH_KNOTS('',3,(#55528,#55529,#55530,#55531,#55532,
#55533,#55534,#55535,#55536,#55537,#55538,#55539,#55540,#55541,#55542,#55543,
#55544,#55545,#55546,#55547,#55548,#55549),.UNSPECIFIED.,.F.,.F.,(4,3,3,
3,3,3,3,4),(-336.707536772222,-335.784332878192,-334.784974744626,-333.78561661106,
-332.786258477494,-331.786900343927,-330.787542210361,-330.424351465042),
 .UNSPECIFIED.);
#1219=B_SPLINE_CURVE_WITH_KNOTS('',3,(#55550,#55551,#55552,#55553,#55554,
#55555,#55556,#55557,#55558,#55559,#55560,#55561,#55562,#55563,#55564,#55565,
#55566,#55567,#55568,#55569,#55570,#55571),.UNSPECIFIED.,.F.,.F.,(4,3,3,
3,3,3,3,4),(327.168696643892,327.789467809663,328.78882594323,329.788184076796,
330.787542210362,331.786900343928,332.786258477494,333.451881951072),
 .UNSPECIFIED.);
#1220=B_SPLINE_CURVE_WITH_KNOTS('',3,(#55576,#55577,#55578,#55579,#55580,
#55581,#55582,#55583,#55584,#55585,#55586,#55587,#55588,#55589,#55590,#55591,
#55592,#55593,#55594,#55595,#55596,#55597,#55598,#55599,#55600),
 .UNSPECIFIED.,.F.,.F.,(4,3,3,3,3,3,3,3,4),(-342.990722079402,-342.779839813154,
-341.780481679588,-340.781123546022,-339.781765412456,-338.78240727889,
-337.783049145324,-336.783691011758,-336.707536772222),.UNSPECIFIED.);
#1221=B_SPLINE_CURVE_WITH_KNOTS('',3,(#55601,#55602,#55603,#55604,#55605,
#55606,#55607,#55608,#55609,#55610,#55611,#55612,#55613,#55614,#55615,#55616,
#55617,#55618,#55619,#55620,#55621,#55622),.UNSPECIFIED.,.F.,.F.,(4,3,3,
3,3,3,3,4),(333.451881951072,333.78561661106,334.784974744626,335.784332878192,
336.783691011758,337.783049145324,338.78240727889,339.735067258252),
 .UNSPECIFIED.);
#1222=B_SPLINE_CURVE_WITH_KNOTS('',3,(#55627,#55628,#55629,#55630,#55631,
#55632,#55633,#55634,#55635,#55636,#55637,#55638,#55639,#55640,#55641,#55642,
#55643,#55644,#55645,#55646,#55647,#55648,#55649,#55650,#55651,#55652,#55653,
#55654,#55655,#55656,#55657,#55658,#55659,#55660),.UNSPECIFIED.,.F.,.F.,
(4,3,3,3,3,3,3,3,3,3,3,4),(-349.273907386581,-348.77598861455,-348.276309547767,
-347.776630480984,-347.276951414201,-346.777272347418,-346.277593280635,
-345.777914213852,-345.278235147069,-344.778556080286,-343.77919794672,
-342.990722079402),.UNSPECIFIED.);
#1223=B_SPLINE_CURVE_WITH_KNOTS('',3,(#55661,#55662,#55663,#55664,#55665,
#55666,#55667,#55668,#55669,#55670,#55671,#55672,#55673,#55674,#55675,#55676,
#55677,#55678,#55679,#55680,#55681,#55682,#55683,#55684,#55685,#55686,#55687,
#55688),.UNSPECIFIED.,.F.,.F.,(4,3,3,3,3,3,3,3,3,4),(339.735067258252,339.781765412456,
340.781123546022,341.780481679588,342.779839813154,343.77919794672,344.778556080286,
345.278235147069,345.777914213852,346.018252565431),.UNSPECIFIED.);
#1224=B_SPLINE_CURVE_WITH_KNOTS('',3,(#55693,#55694,#55695,#55696,#55697,
#55698,#55699,#55700,#55701,#55702,#55703,#55704,#55705,#55706,#55707,#55708,
#55709,#55710,#55711,#55712,#55713,#55714,#55715,#55716,#55717,#55718,#55719,
#55720,#55721,#55722,#55723,#55724,#55725,#55726,#55727,#55728,#55729,#55730,
#55731,#55732,#55733,#55734,#55735),.UNSPECIFIED.,.F.,.F.,(4,3,3,3,3,3,
3,3,3,3,3,3,3,3,4),(-355.557092693761,-355.27181648273,-354.772137415947,
-354.272458349164,-353.77277928238,-353.273100215597,-352.773421148814,
-352.273742082031,-351.774063015248,-351.274383948465,-350.774704881682,
-350.275025814899,-349.775346748116,-349.275667681333,-349.273907386581),
 .UNSPECIFIED.);
#1225=B_SPLINE_CURVE_WITH_KNOTS('',3,(#55736,#55737,#55738,#55739,#55740,
#55741,#55742,#55743,#55744,#55745,#55746,#55747,#55748,#55749,#55750,#55751,
#55752,#55753,#55754,#55755,#55756,#55757,#55758,#55759,#55760,#55761,#55762,
#55763,#55764,#55765,#55766,#55767,#55768,#55769,#55770,#55771,#55772,#55773,
#55774,#55775,#55776,#55777,#55778),.UNSPECIFIED.,.F.,.F.,(4,3,3,3,3,3,
3,3,3,3,3,3,3,3,4),(346.018252565431,346.277593280635,346.777272347418,
347.276951414201,347.776630480984,348.276309547767,348.77598861455,349.275667681334,
349.775346748116,350.2750258149,350.774704881683,351.274383948466,351.774063015249,
352.273742082032,352.301437872611),.UNSPECIFIED.);
#1226=B_SPLINE_CURVE_WITH_KNOTS('',3,(#55783,#55784,#55785,#55786,#55787,
#55788,#55789,#55790,#55791,#55792,#55793,#55794,#55795,#55796,#55797,#55798,
#55799,#55800,#55801,#55802,#55803,#55804,#55805,#55806,#55807,#55808,#55809,
#55810,#55811,#55812,#55813,#55814,#55815,#55816,#55817,#55818,#55819,#55820,
#55821,#55822,#55823,#55824,#55825),.UNSPECIFIED.,.F.,.F.,(4,3,3,3,3,3,
3,3,3,3,3,3,3,3,4),(-361.84027800094,-361.767644350909,-361.267965284126,
-360.768286217343,-360.26860715056,-359.768928083777,-359.269249016994,
-358.769569950211,-358.269890883428,-357.770211816645,-357.270532749862,
-356.770853683079,-356.271174616296,-355.771495549513,-355.557092693761),
 .UNSPECIFIED.);
#1227=B_SPLINE_CURVE_WITH_KNOTS('',3,(#55826,#55827,#55828,#55829,#55830,
#55831,#55832,#55833,#55834,#55835,#55836,#55837,#55838,#55839,#55840,#55841,
#55842,#55843,#55844,#55845,#55846,#55847,#55848,#55849,#55850,#55851,#55852,
#55853,#55854,#55855,#55856,#55857,#55858,#55859,#55860,#55861,#55862,#55863,
#55864,#55865),.UNSPECIFIED.,.F.,.F.,(4,3,3,3,3,3,3,3,3,3,3,3,3,4),(352.301437872611,
352.773421148815,353.273100215598,353.772779282381,354.272458349164,354.772137415947,
355.27181648273,355.771495549513,356.271174616296,356.770853683079,357.270532749862,
357.770211816645,358.269890883428,358.58462317979),.UNSPECIFIED.);
#1228=B_SPLINE_CURVE_WITH_KNOTS('',3,(#55870,#55871,#55872,#55873,#55874,
#55875,#55876,#55877,#55878,#55879,#55880,#55881,#55882,#55883,#55884,#55885,
#55886,#55887,#55888,#55889,#55890,#55891,#55892,#55893,#55894,#55895,#55896,
#55897,#55898,#55899,#55900,#55901,#55902,#55903,#55904,#55905,#55906,#55907,
#55908,#55909),.UNSPECIFIED.,.F.,.F.,(4,3,3,3,3,3,3,3,3,3,3,3,3,4),(-368.12346330812,
-367.763793152305,-367.264114085522,-366.764435018739,-366.264755951956,
-365.765076885173,-365.26539781839,-364.765718751607,-364.266039684824,
-363.766360618041,-363.266681551258,-362.767002484475,-362.267323417692,
-361.84027800094),.UNSPECIFIED.);
#1229=B_SPLINE_CURVE_WITH_KNOTS('',3,(#55910,#55911,#55912,#55913,#55914,
#55915,#55916,#55917,#55918,#55919,#55920,#55921,#55922,#55923,#55924,#55925,
#55926,#55927,#55928,#55929,#55930,#55931,#55932,#55933,#55934,#55935,#55936,
#55937,#55938,#55939,#55940,#55941,#55942,#55943,#55944,#55945,#55946,#55947,
#55948,#55949,#55950,#55951,#55952),.UNSPECIFIED.,.F.,.F.,(4,3,3,3,3,3,
3,3,3,3,3,3,3,3,4),(358.58462317979,358.769569950211,359.269249016994,359.768928083777,
360.26860715056,360.768286217343,361.267965284126,361.767644350909,362.267323417692,
362.767002484475,363.266681551258,363.766360618041,364.266039684824,364.765718751607,
364.86780848697),.UNSPECIFIED.);
#1230=B_SPLINE_CURVE_WITH_KNOTS('',3,(#55957,#55958,#55959,#55960,#55961,
#55962,#55963,#55964,#55965,#55966,#55967,#55968,#55969,#55970,#55971,#55972,
#55973,#55974,#55975,#55976,#55977,#55978,#55979,#55980,#55981,#55982,#55983,
#55984,#55985,#55986,#55987,#55988,#55989,#55990,#55991,#55992,#55993,#55994,
#55995,#55996,#55997,#55998,#55999),.UNSPECIFIED.,.F.,.F.,(4,3,3,3,3,3,
3,3,3,3,3,3,3,3,4),(-374.406648615299,-374.259621020484,-373.759941953701,
-373.260262886918,-372.760583820135,-372.260904753352,-371.761225686569,
-371.261546619786,-370.761867553003,-370.26218848622,-369.762509419437,
-369.262830352654,-368.763151285871,-368.263472219088,-368.12346330812),
 .UNSPECIFIED.);
#1231=B_SPLINE_CURVE_WITH_KNOTS('',3,(#56000,#56001,#56002,#56003,#56004,
#56005,#56006,#56007,#56008,#56009,#56010,#56011,#56012,#56013,#56014,#56015,
#56016,#56017,#56018,#56019,#56020,#56021,#56022,#56023,#56024,#56025,#56026,
#56027,#56028,#56029,#56030,#56031,#56032,#56033,#56034,#56035,#56036,#56037,
#56038,#56039),.UNSPECIFIED.,.F.,.F.,(4,3,3,3,3,3,3,3,3,3,3,3,3,4),(364.86780848697,
365.26539781839,365.765076885173,366.264755951956,366.764435018739,367.264114085522,
367.763793152305,368.263472219088,368.763151285871,369.262830352654,369.762509419437,
370.26218848622,370.761867553004,371.150993794149),.UNSPECIFIED.);
#1232=B_SPLINE_CURVE_WITH_KNOTS('',3,(#56044,#56045,#56046,#56047,#56048,
#56049,#56050,#56051,#56052,#56053,#56054,#56055,#56056,#56057,#56058,#56059,
#56060,#56061,#56062,#56063,#56064,#56065,#56066,#56067,#56068,#56069,#56070,
#56071,#56072,#56073,#56074,#56075,#56076,#56077,#56078,#56079,#56080,#56081,
#56082,#56083),.UNSPECIFIED.,.F.,.F.,(4,3,3,3,3,3,3,3,3,3,3,3,3,4),(-380.689833922479,
-380.255769821881,-379.756090755098,-379.256411688315,-378.756732621532,
-378.257053554749,-377.757374487966,-377.257695421183,-376.7580163544,-376.258337287616,
-375.758658220834,-375.25897915405,-374.759300087267,-374.406648615299),
 .UNSPECIFIED.);
#1233=B_SPLINE_CURVE_WITH_KNOTS('',3,(#56084,#56085,#56086,#56087,#56088,
#56089,#56090,#56091,#56092,#56093,#56094,#56095,#56096,#56097,#56098,#56099,
#56100,#56101,#56102,#56103,#56104,#56105,#56106,#56107,#56108,#56109,#56110,
#56111,#56112,#56113,#56114,#56115,#56116,#56117,#56118,#56119,#56120,#56121,
#56122,#56123,#56124,#56125,#56126),.UNSPECIFIED.,.F.,.F.,(4,3,3,3,3,3,
3,3,3,3,3,3,3,3,4),(371.150993794149,371.261546619787,371.76122568657,372.260904753353,
372.760583820136,373.260262886919,373.759941953702,374.259621020485,374.759300087268,
375.258979154051,375.758658220834,376.258337287617,376.7580163544,377.257695421183,
377.434179101329),.UNSPECIFIED.);
#1234=B_SPLINE_CURVE_WITH_KNOTS('',3,(#56131,#56132,#56133,#56134,#56135,
#56136,#56137,#56138,#56139,#56140,#56141,#56142,#56143,#56144,#56145,#56146,
#56147,#56148,#56149,#56150,#56151,#56152,#56153,#56154,#56155,#56156,#56157,
#56158,#56159,#56160,#56161,#56162,#56163,#56164,#56165,#56166,#56167,#56168,
#56169,#56170,#56171,#56172,#56173),.UNSPECIFIED.,.F.,.F.,(4,3,3,3,3,3,
3,3,3,3,3,3,3,3,4),(-386.973019229658,-386.75159769006,-386.251918623277,
-385.752239556494,-385.252560489711,-384.752881422928,-384.253202356145,
-383.753523289362,-383.253844222579,-382.754165155796,-382.254486089013,
-381.75480702223,-381.255127955447,-380.755448888664,-380.689833922479),
 .UNSPECIFIED.);
#1235=B_SPLINE_CURVE_WITH_KNOTS('',3,(#56174,#56175,#56176,#56177,#56178,
#56179,#56180,#56181,#56182,#56183,#56184,#56185,#56186,#56187,#56188,#56189,
#56190,#56191,#56192,#56193,#56194,#56195,#56196,#56197,#56198,#56199,#56200,
#56201,#56202,#56203,#56204,#56205,#56206,#56207,#56208,#56209,#56210,#56211,
#56212,#56213),.UNSPECIFIED.,.F.,.F.,(4,3,3,3,3,3,3,3,3,3,3,3,3,4),(377.434179101329,
377.757374487966,378.257053554749,378.756732621532,379.256411688315,379.756090755098,
380.255769821881,380.755448888664,381.255127955447,381.75480702223,382.254486089013,
382.754165155796,383.253844222579,383.717364408508),.UNSPECIFIED.);
#1236=B_SPLINE_CURVE_WITH_KNOTS('',3,(#56218,#56219,#56220,#56221,#56222,
#56223,#56224,#56225,#56226,#56227,#56228,#56229,#56230,#56231,#56232,#56233,
#56234,#56235,#56236,#56237,#56238,#56239,#56240,#56241,#56242,#56243,#56244,
#56245,#56246,#56247,#56248,#56249,#56250,#56251,#56252,#56253,#56254,#56255,
#56256,#56257,#56258,#56259,#56260),.UNSPECIFIED.,.F.,.F.,(4,3,3,3,3,3,
3,3,3,3,3,3,3,3,4),(-393.256204536838,-393.247425558239,-392.747746491456,
-392.248067424673,-391.74838835789,-391.248709291107,-390.749030224324,
-390.249351157541,-389.749672090758,-389.249993023975,-388.750313957192,
-388.250634890409,-387.750955823626,-387.251276756843,-386.973019229658),
 .UNSPECIFIED.);
#1237=B_SPLINE_CURVE_WITH_KNOTS('',3,(#56261,#56262,#56263,#56264,#56265,
#56266,#56267,#56268,#56269,#56270,#56271,#56272,#56273,#56274,#56275,#56276,
#56277,#56278,#56279,#56280,#56281,#56282,#56283,#56284,#56285,#56286,#56287,
#56288,#56289,#56290,#56291,#56292,#56293,#56294,#56295,#56296,#56297,#56298,
#56299,#56300,#56301,#56302,#56303),.UNSPECIFIED.,.F.,.F.,(4,3,3,3,3,3,
3,3,3,3,3,3,3,3,4),(383.717364408508,383.753523289362,384.253202356145,
384.752881422928,385.252560489711,385.752239556494,386.251918623277,386.75159769006,
387.251276756843,387.750955823626,388.250634890409,388.750313957192,389.249993023975,
389.749672090758,390.000549715688),.UNSPECIFIED.);
#1238=B_SPLINE_CURVE_WITH_KNOTS('',3,(#56309,#56310,#56311,#56312),
 .UNSPECIFIED.,.F.,.F.,(4,4),(405.265452313083,405.755527026166),
 .UNSPECIFIED.);
#1239=B_SPLINE_CURVE_WITH_KNOTS('',3,(#56318,#56319,#56320,#56321,#56322,
#56323,#56324,#56325,#56326,#56327,#56328,#56329,#56330,#56331,#56332,#56333,
#56334),.UNSPECIFIED.,.F.,.F.,(4,1,1,1,1,1,1,1,1,1,1,1,1,1,4),(398.982267005903,
399.260524533088,399.760203599871,400.259882666654,400.759561733437,401.25924080022,
401.758919867003,402.258598933787,402.75827800057,403.257957067353,403.757636134136,
404.257315200919,404.756994267702,405.256673334485,405.265452313083),
 .UNSPECIFIED.);
#1240=B_SPLINE_CURVE_WITH_KNOTS('',3,(#56337,#56338,#56339,#56340,#56341,
#56342,#56343,#56344,#56345,#56346,#56347,#56348,#56349),.UNSPECIFIED.,
 .F.,.F.,(4,1,1,1,1,1,1,1,1,1,4),(398.982267005904,399.231068447758,399.730747514541,
400.230426581324,400.730105648107,401.22978471489,401.729463781673,402.229142848456,
402.728821915239,403.228500982022,403.728180048805),.UNSPECIFIED.);
#1241=B_SPLINE_CURVE_WITH_KNOTS('',3,(#56354,#56355,#56356,#56357,#56358,
#56359,#56360,#56361,#56362,#56363,#56364,#56365,#56366,#56367,#56368,#56369,
#56370),.UNSPECIFIED.,.F.,.F.,(4,1,1,1,1,1,1,1,1,1,1,1,1,1,4),(392.699081698724,
392.764696664909,393.264375731692,393.764054798475,394.263733865258,394.763412932041,
395.263091998824,395.762771065607,396.26245013239,396.762129199173,397.261808265956,
397.761487332739,398.261166399522,398.760845466305,398.982267005903),
 .UNSPECIFIED.);
#1242=B_SPLINE_CURVE_WITH_KNOTS('',3,(#56371,#56372,#56373,#56374,#56375,
#56376,#56377,#56378,#56379,#56380,#56381,#56382,#56383,#56384,#56385,#56386,
#56387),.UNSPECIFIED.,.F.,.F.,(4,1,1,1,1,1,1,1,1,1,1,1,1,1,4),(392.699081698724,
392.735240579579,393.234919646362,393.734598713145,394.234277779928,394.733956846711,
395.233635913494,395.733314980277,396.23299404706,396.732673113843,397.232352180626,
397.732031247409,398.231710314192,398.731389380975,398.982267005904),
 .UNSPECIFIED.);
#1243=B_SPLINE_CURVE_WITH_KNOTS('',3,(#56392,#56393,#56394,#56395,#56396,
#56397,#56398,#56399,#56400,#56401,#56402,#56403,#56404,#56405,#56406,#56407),
 .UNSPECIFIED.,.F.,.F.,(4,1,1,1,1,1,1,1,1,1,1,1,1,4),(386.415896391544,
386.768547863513,387.268226930296,387.767905997079,388.267585063862,388.767264130645,
389.266943197428,389.766622264211,390.266301330994,390.765980397777,391.26565946456,
391.765338531343,392.265017598126,392.699081698724),.UNSPECIFIED.);
#1244=B_SPLINE_CURVE_WITH_KNOTS('',3,(#56408,#56409,#56410,#56411,#56412,
#56413,#56414,#56415,#56416,#56417,#56418,#56419,#56420,#56421,#56422,#56423),
 .UNSPECIFIED.,.F.,.F.,(4,1,1,1,1,1,1,1,1,1,1,1,1,4),(386.415896391545,
386.739091778183,387.238770844966,387.738449911749,388.238128978532,388.737808045315,
389.237487112098,389.737166178881,390.236845245664,390.736524312447,391.23620337923,
391.735882446013,392.235561512796,392.699081698724),.UNSPECIFIED.);
#1245=B_SPLINE_CURVE_WITH_KNOTS('',3,(#56428,#56429,#56430,#56431,#56432,
#56433,#56434,#56435,#56436,#56437,#56438,#56439,#56440,#56441,#56442,#56443,
#56444),.UNSPECIFIED.,.F.,.F.,(4,1,1,1,1,1,1,1,1,1,1,1,1,1,4),(380.132711084365,
380.272719995333,380.772399062117,381.2720781289,381.771757195683,382.271436262466,
382.771115329249,383.270794396032,383.770473462815,384.270152529598,384.769831596381,
385.269510663164,385.769189729947,386.26886879673,386.415896391544),
 .UNSPECIFIED.);
#1246=B_SPLINE_CURVE_WITH_KNOTS('',3,(#56445,#56446,#56447,#56448,#56449,
#56450,#56451,#56452,#56453,#56454,#56455,#56456,#56457,#56458,#56459,#56460,
#56461),.UNSPECIFIED.,.F.,.F.,(4,1,1,1,1,1,1,1,1,1,1,1,1,1,4),(380.132711084365,
380.243263910003,380.742942976786,381.242622043569,381.742301110352,382.241980177135,
382.741659243918,383.241338310702,383.741017377485,384.240696444268,384.740375511051,
385.240054577834,385.739733644617,386.2394127114,386.415896391545),
 .UNSPECIFIED.);
#1247=B_SPLINE_CURVE_WITH_KNOTS('',3,(#56466,#56467,#56468,#56469,#56470,
#56471,#56472,#56473,#56474,#56475,#56476,#56477,#56478,#56479,#56480,#56481),
 .UNSPECIFIED.,.F.,.F.,(4,1,1,1,1,1,1,1,1,1,1,1,1,4),(373.849525777185,
374.276571193937,374.77625026072,375.275929327503,375.775608394286,376.275287461069,
376.774966527852,377.274645594635,377.774324661418,378.274003728201,378.773682794984,
379.273361861767,379.77304092855,380.132711084365),.UNSPECIFIED.);
#1248=B_SPLINE_CURVE_WITH_KNOTS('',3,(#56482,#56483,#56484,#56485,#56486,
#56487,#56488,#56489,#56490,#56491,#56492,#56493,#56494,#56495,#56496,#56497),
 .UNSPECIFIED.,.F.,.F.,(4,1,1,1,1,1,1,1,1,1,1,1,1,4),(373.849525777185,
374.247115108607,374.74679417539,375.246473242173,375.746152308956,376.245831375739,
376.745510442522,377.245189509305,377.744868576088,378.244547642871,378.744226709654,
379.243905776437,379.74358484322,380.132711084365),.UNSPECIFIED.);
#1249=B_SPLINE_CURVE_WITH_KNOTS('',3,(#56502,#56503,#56504,#56505,#56506,
#56507,#56508,#56509,#56510,#56511,#56512,#56513,#56514,#56515,#56516,#56517,
#56518),.UNSPECIFIED.,.F.,.F.,(4,1,1,1,1,1,1,1,1,1,1,1,1,1,4),(367.566340470006,
367.780743325758,368.280422392541,368.780101459324,369.279780526107,369.77945959289,
370.279138659673,370.778817726456,371.278496793239,371.778175860022,372.277854926805,
372.777533993588,373.277213060371,373.776892127154,373.849525777185),
 .UNSPECIFIED.);
#1250=B_SPLINE_CURVE_WITH_KNOTS('',3,(#56519,#56520,#56521,#56522,#56523,
#56524,#56525,#56526,#56527,#56528,#56529,#56530,#56531,#56532,#56533,#56534,
#56535),.UNSPECIFIED.,.F.,.F.,(4,1,1,1,1,1,1,1,1,1,1,1,1,1,4),(367.566340470006,
367.751287240428,368.250966307211,368.750645373994,369.250324440777,369.75000350756,
370.249682574343,370.749361641126,371.249040707909,371.748719774692,372.248398841475,
372.748077908258,373.247756975041,373.747436041824,373.849525777185),
 .UNSPECIFIED.);
#1251=B_SPLINE_CURVE_WITH_KNOTS('',3,(#56540,#56541,#56542,#56543,#56544,
#56545,#56546,#56547,#56548,#56549,#56550,#56551,#56552,#56553,#56554,#56555,
#56556),.UNSPECIFIED.,.F.,.F.,(4,1,1,1,1,1,1,1,1,1,1,1,1,1,4),(361.283155162826,
361.284915457579,361.784594524362,362.284273591145,362.783952657928,363.283631724711,
363.783310791494,364.282989858277,364.78266892506,365.282347991843,365.782027058626,
366.281706125409,366.781385192192,367.281064258975,367.566340470006),
 .UNSPECIFIED.);
#1252=B_SPLINE_CURVE_WITH_KNOTS('',3,(#56557,#56558,#56559,#56560,#56561,
#56562,#56563,#56564,#56565,#56566,#56567,#56568,#56569,#56570,#56571,#56572),
 .UNSPECIFIED.,.F.,.F.,(4,1,1,1,1,1,1,1,1,1,1,1,1,4),(361.283155162826,
361.755138439031,362.254817505815,362.754496572598,363.254175639381,363.753854706164,
364.253533772947,364.75321283973,365.252891906513,365.752570973296,366.252250040079,
366.751929106862,367.251608173645,367.566340470006),.UNSPECIFIED.);
#1253=B_SPLINE_CURVE_WITH_KNOTS('',3,(#56577,#56578,#56579,#56580,#56581,
#56582,#56583,#56584,#56585,#56586,#56587,#56588,#56589,#56590),
 .UNSPECIFIED.,.F.,.F.,(4,1,1,1,1,1,1,1,1,1,1,4),(354.999969855646,355.788445722965,
356.787803856531,357.287482923314,357.787161990097,358.28684105688,358.786520123663,
359.286199190446,359.78587825723,360.285557324013,360.785236390796,361.283155162826),
 .UNSPECIFIED.);
#1254=B_SPLINE_CURVE_WITH_KNOTS('',3,(#56591,#56592,#56593,#56594,#56595,
#56596,#56597,#56598,#56599,#56600,#56601,#56602,#56603,#56604,#56605,#56606,
#56607),.UNSPECIFIED.,.F.,.F.,(4,1,1,1,1,1,1,1,1,1,1,1,1,1,4),(354.999969855647,
355.259310570852,355.758989637635,356.258668704418,356.758347771201,357.258026837984,
357.757705904767,358.25738497155,358.757064038333,359.256743105116,359.756422171899,
360.256101238682,360.755780305465,361.255459372248,361.283155162826),
 .UNSPECIFIED.);
#1255=B_SPLINE_CURVE_WITH_KNOTS('',3,(#56612,#56613,#56614,#56615,#56616,
#56617,#56618,#56619,#56620,#56621,#56622),.UNSPECIFIED.,.F.,.F.,(4,1,1,
1,1,1,1,1,4),(348.716784548467,348.792938788003,349.792296921569,350.791655055135,
351.791013188701,352.790371322267,353.789729455833,354.789087589399,354.999969855646),
 .UNSPECIFIED.);
#1256=B_SPLINE_CURVE_WITH_KNOTS('',3,(#56623,#56624,#56625,#56626,#56627,
#56628,#56629,#56630,#56631,#56632,#56633,#56634),.UNSPECIFIED.,.F.,.F.,
(4,1,1,1,1,1,1,1,1,4),(348.716784548467,348.763482702673,349.762840836239,
350.762198969805,351.761557103371,352.760915236937,353.760273370503,354.259952437286,
354.759631504069,354.999969855647),.UNSPECIFIED.);
#1257=B_SPLINE_CURVE_WITH_KNOTS('',3,(#56639,#56640,#56641,#56642,#56643,
#56644,#56645,#56646,#56647,#56648),.UNSPECIFIED.,.F.,.F.,(4,1,1,1,1,1,
1,4),(342.433599241287,342.796789986607,343.796148120173,344.795506253739,
345.794864387305,346.794222520871,347.793580654437,348.716784548467),
 .UNSPECIFIED.);
#1258=B_SPLINE_CURVE_WITH_KNOTS('',3,(#56649,#56650,#56651,#56652,#56653,
#56654,#56655,#56656,#56657,#56658),.UNSPECIFIED.,.F.,.F.,(4,1,1,1,1,1,
1,4),(342.433599241288,342.767333901277,343.766692034843,344.766050168409,
345.765408301975,346.764766435541,347.764124569107,348.716784548467),
 .UNSPECIFIED.);
#1259=B_SPLINE_CURVE_WITH_KNOTS('',3,(#56663,#56664,#56665,#56666,#56667,
#56668,#56669,#56670,#56671,#56672),.UNSPECIFIED.,.F.,.F.,(4,1,1,1,1,1,
1,4),(336.150413934108,336.80064118521,337.799999318776,338.799357452343,
339.798715585909,340.798073719475,341.797431853041,342.433599241287),
 .UNSPECIFIED.);
#1260=B_SPLINE_CURVE_WITH_KNOTS('',3,(#56673,#56674,#56675,#56676,#56677,
#56678,#56679,#56680,#56681,#56682),.UNSPECIFIED.,.F.,.F.,(4,1,1,1,1,1,
1,4),(336.150413934108,336.77118509988,337.770543233446,338.769901367012,
339.769259500578,340.768617634145,341.767975767711,342.433599241288),
 .UNSPECIFIED.);
#1261=B_SPLINE_CURVE_WITH_KNOTS('',3,(#56687,#56688,#56689,#56690,#56691,
#56692,#56693,#56694,#56695,#56696),.UNSPECIFIED.,.F.,.F.,(4,1,1,1,1,1,
1,4),(329.867228626928,330.804492383814,331.80385051738,332.803208650946,
333.802566784512,334.801924918078,335.801283051644,336.150413934108),
 .UNSPECIFIED.);
#1262=B_SPLINE_CURVE_WITH_KNOTS('',3,(#56697,#56698,#56699,#56700,#56701,
#56702,#56703,#56704,#56705,#56706),.UNSPECIFIED.,.F.,.F.,(4,1,1,1,1,1,
1,4),(329.867228626928,330.775036298484,331.77439443205,332.773752565616,
333.773110699182,334.772468832748,335.771826966314,336.150413934108),
 .UNSPECIFIED.);
#1263=B_SPLINE_CURVE_WITH_KNOTS('',3,(#56711,#56712,#56713,#56714,#56715,
#56716,#56717,#56718,#56719,#56720,#56721),.UNSPECIFIED.,.F.,.F.,(4,1,1,
1,1,1,1,1,4),(323.584043319749,323.808985448852,324.808343582418,325.807701715984,
326.80705984955,327.806417983116,328.805776116682,329.805134250248,329.867228626928),
 .UNSPECIFIED.);
#1264=B_SPLINE_CURVE_WITH_KNOTS('',3,(#56722,#56723,#56724,#56725,#56726,
#56727,#56728,#56729,#56730,#56731,#56732),.UNSPECIFIED.,.F.,.F.,(4,1,1,
1,1,1,1,1,4),(323.584043319749,323.779529363522,324.778887497088,325.778245630654,
326.77760376422,327.776961897786,328.776320031352,329.775678164918,329.867228626928),
 .UNSPECIFIED.);
#1265=B_SPLINE_CURVE_WITH_KNOTS('',3,(#56737,#56738,#56739,#56740,#56741,
#56742,#56743,#56744,#56745,#56746),.UNSPECIFIED.,.F.,.F.,(4,1,1,1,1,1,
1,4),(317.300858012569,317.812836647456,318.812194781022,319.811552914588,
320.810911048154,321.81026918172,322.809627315286,323.584043319749),
 .UNSPECIFIED.);
#1266=B_SPLINE_CURVE_WITH_KNOTS('',3,(#56747,#56748,#56749,#56750,#56751,
#56752,#56753,#56754,#56755,#56756),.UNSPECIFIED.,.F.,.F.,(4,1,1,1,1,1,
1,4),(317.300858012569,317.783380562125,318.782738695691,319.782096829258,
320.781454962824,321.78081309639,322.780171229956,323.584043319749),
 .UNSPECIFIED.);
#1267=B_SPLINE_CURVE_WITH_KNOTS('',3,(#56761,#56762,#56763,#56764,#56765,
#56766,#56767,#56768,#56769,#56770),.UNSPECIFIED.,.F.,.F.,(4,1,1,1,1,1,
1,4),(311.017672705389,311.816687846059,312.816045979625,313.815404113191,
314.814762246757,315.814120380323,316.81347851389,317.300858012569),
 .UNSPECIFIED.);
#1268=B_SPLINE_CURVE_WITH_KNOTS('',3,(#56771,#56772,#56773,#56774,#56775,
#56776,#56777,#56778,#56779,#56780),.UNSPECIFIED.,.F.,.F.,(4,1,1,1,1,1,
1,4),(311.01767270539,311.787231760729,312.786589894295,313.785948027861,
314.785306161427,315.784664294993,316.784022428559,317.300858012569),
 .UNSPECIFIED.);
#1269=B_SPLINE_CURVE_WITH_KNOTS('',3,(#56785,#56786,#56787,#56788,#56789,
#56790,#56791,#56792,#56793,#56794,#56795),.UNSPECIFIED.,.F.,.F.,(4,1,1,
1,1,1,1,1,4),(304.73448739821,304.821180911097,305.820539044663,306.819897178229,
307.819255311795,308.818613445361,309.817971578927,310.817329712493,311.017672705389),
 .UNSPECIFIED.);
#1270=B_SPLINE_CURVE_WITH_KNOTS('',3,(#56796,#56797,#56798,#56799,#56800,
#56801,#56802,#56803,#56804,#56805,#56806),.UNSPECIFIED.,.F.,.F.,(4,1,1,
1,1,1,1,1,4),(304.73448739821,304.791724825767,305.791082959333,306.790441092899,
307.789799226465,308.789157360031,309.788515493597,310.787873627163,311.01767270539),
 .UNSPECIFIED.);
#1271=B_SPLINE_CURVE_WITH_KNOTS('',3,(#56811,#56812,#56813,#56814,#56815,
#56816,#56817,#56818,#56819,#56820),.UNSPECIFIED.,.F.,.F.,(4,1,1,1,1,1,
1,4),(298.45130209103,298.825032109701,299.824390243267,300.823748376833,
301.823106510399,302.822464643965,303.821822777531,304.73448739821),
 .UNSPECIFIED.);
#1272=B_SPLINE_CURVE_WITH_KNOTS('',3,(#56821,#56822,#56823,#56824,#56825,
#56826,#56827,#56828,#56829,#56830),.UNSPECIFIED.,.F.,.F.,(4,1,1,1,1,1,
1,4),(298.451302091031,298.795576024371,299.794934157937,300.794292291503,
301.793650425069,302.793008558635,303.792366692201,304.73448739821),
 .UNSPECIFIED.);
#1273=B_SPLINE_CURVE_WITH_KNOTS('',3,(#56835,#56836,#56837,#56838,#56839,
#56840,#56841,#56842,#56843,#56844),.UNSPECIFIED.,.F.,.F.,(4,1,1,1,1,1,
1,4),(292.168116783851,292.828883308304,293.82824144187,294.827599575437,
295.826957709003,296.826315842569,297.825673976135,298.45130209103),
 .UNSPECIFIED.);
#1274=B_SPLINE_CURVE_WITH_KNOTS('',3,(#56845,#56846,#56847,#56848,#56849,
#56850,#56851,#56852,#56853,#56854),.UNSPECIFIED.,.F.,.F.,(4,1,1,1,1,1,
1,4),(292.168116783851,292.799427222974,293.79878535654,294.798143490106,
295.797501623672,296.796859757238,297.796217890804,298.451302091031),
 .UNSPECIFIED.);
#1275=B_SPLINE_CURVE_WITH_KNOTS('',3,(#56859,#56860,#56861,#56862,#56863,
#56864,#56865,#56866,#56867,#56868),.UNSPECIFIED.,.F.,.F.,(4,1,1,1,1,1,
1,4),(285.884931476671,286.832734506908,287.832092640474,288.83145077404,
289.830808907606,290.830167041172,291.829525174738,292.168116783851),
 .UNSPECIFIED.);
#1276=B_SPLINE_CURVE_WITH_KNOTS('',3,(#56869,#56870,#56871,#56872,#56873,
#56874,#56875,#56876,#56877,#56878),.UNSPECIFIED.,.F.,.F.,(4,1,1,1,1,1,
1,4),(285.884931476672,286.803278421578,287.802636555144,288.80199468871,
289.801352822276,290.800710955842,291.800069089408,292.168116783851),
 .UNSPECIFIED.);
#1277=B_SPLINE_CURVE_WITH_KNOTS('',3,(#56883,#56884,#56885,#56886,#56887,
#56888,#56889,#56890,#56891,#56892,#56893),.UNSPECIFIED.,.F.,.F.,(4,1,1,
1,1,1,1,1,4),(279.601746169492,279.837227571946,280.836585705512,281.835943839078,
282.835301972644,283.83466010621,284.834018239776,285.833376373342,285.884931476671),
 .UNSPECIFIED.);
#1278=B_SPLINE_CURVE_WITH_KNOTS('',3,(#56894,#56895,#56896,#56897,#56898,
#56899,#56900,#56901,#56902,#56903,#56904),.UNSPECIFIED.,.F.,.F.,(4,1,1,
1,1,1,1,1,4),(279.601746169492,279.807771486616,280.807129620182,281.806487753748,
282.805845887314,283.80520402088,284.804562154446,285.803920288012,285.884931476672),
 .UNSPECIFIED.);
#1279=B_SPLINE_CURVE_WITH_KNOTS('',3,(#56909,#56910,#56911,#56912,#56913,
#56914,#56915,#56916,#56917,#56918),.UNSPECIFIED.,.F.,.F.,(4,1,1,1,1,1,
1,4),(273.318560862312,273.84107877055,274.840436904116,275.839795037682,
276.839153171248,277.838511304814,278.83786943838,279.601746169492),
 .UNSPECIFIED.);
#1280=B_SPLINE_CURVE_WITH_KNOTS('',3,(#56919,#56920,#56921,#56922,#56923,
#56924,#56925,#56926,#56927,#56928),.UNSPECIFIED.,.F.,.F.,(4,1,1,1,1,1,
1,4),(273.318560862312,273.811622685219,274.810980818785,275.810338952351,
276.809697085917,277.809055219484,278.80841335305,279.601746169492),
 .UNSPECIFIED.);
#1281=B_SPLINE_CURVE_WITH_KNOTS('',3,(#56933,#56934,#56935,#56936,#56937,
#56938,#56939,#56940,#56941,#56942),.UNSPECIFIED.,.F.,.F.,(4,1,1,1,1,1,
1,4),(267.035375555133,267.844929969153,268.844288102719,269.843646236285,
270.843004369851,271.842362503417,272.841720636983,273.318560862312),
 .UNSPECIFIED.);
#1282=B_SPLINE_CURVE_WITH_KNOTS('',3,(#56943,#56944,#56945,#56946,#56947,
#56948,#56949,#56950,#56951,#56952),.UNSPECIFIED.,.F.,.F.,(4,1,1,1,1,1,
1,4),(267.035375555133,267.815473883823,268.814832017389,269.814190150955,
270.813548284521,271.812906418087,272.812264551653,273.318560862312),
 .UNSPECIFIED.);
#1283=B_SPLINE_CURVE_WITH_KNOTS('',3,(#56957,#56958,#56959,#56960,#56961,
#56962,#56963,#56964,#56965,#56966,#56967),.UNSPECIFIED.,.F.,.F.,(4,1,1,
1,1,1,1,1,4),(260.752190247953,260.849423034191,261.848781167757,262.848139301323,
263.847497434889,264.846855568455,265.846213702021,266.845571835587,267.035375555133),
 .UNSPECIFIED.);
#1284=B_SPLINE_CURVE_WITH_KNOTS('',3,(#56968,#56969,#56970,#56971,#56972,
#56973,#56974,#56975,#56976,#56977,#56978),.UNSPECIFIED.,.F.,.F.,(4,1,1,
1,1,1,1,1,4),(260.752190247953,260.819966948861,261.819325082427,262.818683215993,
263.818041349559,264.817399483125,265.816757616691,266.816115750257,267.035375555133),
 .UNSPECIFIED.);
#1285=B_SPLINE_CURVE_WITH_KNOTS('',3,(#56983,#56984,#56985,#56986,#56987,
#56988,#56989,#56990,#56991,#56992),.UNSPECIFIED.,.F.,.F.,(4,1,1,1,1,1,
1,4),(254.469004940773,254.853274232795,255.852632366361,256.851990499927,
257.851348633493,258.850706767059,259.850064900625,260.752190247953),
 .UNSPECIFIED.);
#1286=B_SPLINE_CURVE_WITH_KNOTS('',3,(#56993,#56994,#56995,#56996,#56997,
#56998,#56999,#57000,#57001,#57002),.UNSPECIFIED.,.F.,.F.,(4,1,1,1,1,1,
1,4),(254.469004940774,254.823818147464,255.82317628103,256.822534414597,
257.821892548163,258.821250681729,259.820608815295,260.752190247953),
 .UNSPECIFIED.);
#1287=B_SPLINE_CURVE_WITH_KNOTS('',3,(#57007,#57008,#57009,#57010,#57011,
#57012,#57013,#57014,#57015,#57016),.UNSPECIFIED.,.F.,.F.,(4,1,1,1,1,1,
1,4),(248.185819633594,248.857125431398,249.856483564964,250.85584169853,
251.855199832097,252.854557965663,253.853916099229,254.469004940773),
 .UNSPECIFIED.);
#1288=B_SPLINE_CURVE_WITH_KNOTS('',3,(#57017,#57018,#57019,#57020,#57021,
#57022,#57023,#57024,#57025,#57026),.UNSPECIFIED.,.F.,.F.,(4,1,1,1,1,1,
1,4),(248.185819633594,248.827669346068,249.827027479634,250.8263856132,
251.825743746766,252.825101880332,253.824460013898,254.469004940774),
 .UNSPECIFIED.);
#1289=B_SPLINE_CURVE_WITH_KNOTS('',3,(#57031,#57032,#57033,#57034,#57035,
#57036,#57037,#57038,#57039,#57040),.UNSPECIFIED.,.F.,.F.,(4,1,1,1,1,1,
1,4),(241.902634326414,242.860976630002,243.860334763568,244.859692897134,
245.8590510307,246.858409164266,247.857767297832,248.185819633594),
 .UNSPECIFIED.);
#1290=B_SPLINE_CURVE_WITH_KNOTS('',3,(#57041,#57042,#57043,#57044,#57045,
#57046,#57047,#57048,#57049,#57050),.UNSPECIFIED.,.F.,.F.,(4,1,1,1,1,1,
1,4),(241.902634326415,242.831520544672,243.830878678238,244.830236811804,
245.82959494537,246.828953078936,247.828311212502,248.185819633594),
 .UNSPECIFIED.);
#1291=B_SPLINE_CURVE_WITH_KNOTS('',3,(#57055,#57056,#57057,#57058,#57059,
#57060,#57061,#57062,#57063,#57064,#57065),.UNSPECIFIED.,.F.,.F.,(4,1,1,
1,1,1,1,1,4),(235.619449019235,235.86546969504,236.864827828606,237.864185962172,
238.863544095738,239.862902229304,240.86226036287,241.861618496436,241.902634326414),
 .UNSPECIFIED.);
#1292=B_SPLINE_CURVE_WITH_KNOTS('',3,(#57066,#57067,#57068,#57069,#57070,
#57071,#57072,#57073,#57074,#57075,#57076),.UNSPECIFIED.,.F.,.F.,(4,1,1,
1,1,1,1,1,4),(235.619449019235,235.83601360971,236.835371743276,237.834729876842,
238.834088010408,239.833446143974,240.83280427754,241.832162411106,241.902634326415),
 .UNSPECIFIED.);
#1293=B_SPLINE_CURVE_WITH_KNOTS('',3,(#57081,#57082,#57083,#57084,#57085,
#57086,#57087,#57088,#57089,#57090),.UNSPECIFIED.,.F.,.F.,(4,1,1,1,1,1,
1,4),(229.336263712055,229.869320893643,230.86867902721,231.868037160776,
232.867395294342,233.866753427908,234.866111561474,235.619449019235),
 .UNSPECIFIED.);
#1294=B_SPLINE_CURVE_WITH_KNOTS('',3,(#57091,#57092,#57093,#57094,#57095,
#57096,#57097,#57098,#57099,#57100),.UNSPECIFIED.,.F.,.F.,(4,1,1,1,1,1,
1,4),(229.336263712055,229.839864808313,230.839222941879,231.838581075445,
232.837939209011,233.837297342577,234.836655476144,235.619449019235),
 .UNSPECIFIED.);
#1295=B_SPLINE_CURVE_WITH_KNOTS('',3,(#57105,#57106,#57107,#57108,#57109,
#57110,#57111,#57112,#57113,#57114),.UNSPECIFIED.,.F.,.F.,(4,1,1,1,1,1,
1,4),(223.053078404876,223.873172092247,224.872530225813,225.871888359379,
226.871246492945,227.870604626511,228.869962760077,229.336263712055),
 .UNSPECIFIED.);
#1296=B_SPLINE_CURVE_WITH_KNOTS('',3,(#57115,#57116,#57117,#57118,#57119,
#57120,#57121,#57122,#57123,#57124),.UNSPECIFIED.,.F.,.F.,(4,1,1,1,1,1,
1,4),(223.053078404876,223.843716006917,224.843074140483,225.842432274049,
226.841790407615,227.841148541181,228.840506674747,229.336263712055),
 .UNSPECIFIED.);
#1297=B_SPLINE_CURVE_WITH_KNOTS('',3,(#57129,#57130,#57131,#57132,#57133,
#57134,#57135,#57136,#57137,#57138,#57139),.UNSPECIFIED.,.F.,.F.,(4,1,1,
1,1,1,1,1,4),(216.769893097696,216.877665157285,217.877023290851,218.876381424417,
219.875739557983,220.875097691549,221.874455825115,222.873813958681,223.053078404876),
 .UNSPECIFIED.);
#1298=B_SPLINE_CURVE_WITH_KNOTS('',3,(#57140,#57141,#57142,#57143,#57144,
#57145,#57146,#57147,#57148,#57149,#57150),.UNSPECIFIED.,.F.,.F.,(4,1,1,
1,1,1,1,1,4),(216.769893097696,216.848209071955,217.847567205521,218.846925339087,
219.846283472653,220.845641606219,221.844999739785,222.844357873351,223.053078404876),
 .UNSPECIFIED.);
#1299=B_SPLINE_CURVE_WITH_KNOTS('',3,(#57155,#57156,#57157,#57158,#57159,
#57160,#57161,#57162,#57163,#57164),.UNSPECIFIED.,.F.,.F.,(4,1,1,1,1,1,
1,4),(210.486707790516,210.881516355889,211.880874489455,212.880232623021,
213.879590756587,214.878948890153,215.878307023719,216.769893097696),
 .UNSPECIFIED.);
#1300=B_SPLINE_CURVE_WITH_KNOTS('',3,(#57165,#57166,#57167,#57168,#57169,
#57170,#57171,#57172,#57173,#57174),.UNSPECIFIED.,.F.,.F.,(4,1,1,1,1,1,
1,4),(210.486707790517,210.852060270558,211.851418404124,212.85077653769,
213.850134671257,214.849492804823,215.848850938389,216.769893097696),
 .UNSPECIFIED.);
#1301=B_SPLINE_CURVE_WITH_KNOTS('',3,(#57179,#57180,#57181,#57182,#57183,
#57184,#57185,#57186,#57187,#57188),.UNSPECIFIED.,.F.,.F.,(4,1,1,1,1,1,
1,4),(204.203522483337,204.885367554492,205.884725688058,206.884083821624,
207.88344195519,208.882800088756,209.882158222323,210.486707790516),
 .UNSPECIFIED.);
#1302=B_SPLINE_CURVE_WITH_KNOTS('',3,(#57189,#57190,#57191,#57192,#57193,
#57194,#57195,#57196,#57197,#57198),.UNSPECIFIED.,.F.,.F.,(4,1,1,1,1,1,
1,4),(204.203522483337,204.855911469162,205.855269602728,206.854627736294,
207.85398586986,208.853344003426,209.852702136992,210.486707790517),
 .UNSPECIFIED.);
#1303=B_SPLINE_CURVE_WITH_KNOTS('',3,(#57203,#57204,#57205,#57206,#57207,
#57208,#57209,#57210,#57211,#57212),.UNSPECIFIED.,.F.,.F.,(4,1,1,1,1,1,
1,4),(197.920337176157,198.889218753096,199.888576886662,200.887935020228,
201.887293153794,202.88665128736,203.886009420926,204.203522483337),
 .UNSPECIFIED.);
#1304=B_SPLINE_CURVE_WITH_KNOTS('',3,(#57213,#57214,#57215,#57216,#57217,
#57218,#57219,#57220,#57221,#57222),.UNSPECIFIED.,.F.,.F.,(4,1,1,1,1,1,
1,4),(197.920337176158,198.859762667766,199.859120801332,200.858478934898,
201.857837068464,202.85719520203,203.856553335596,204.203522483337),
 .UNSPECIFIED.);
#1305=B_SPLINE_CURVE_WITH_KNOTS('',3,(#57227,#57228,#57229,#57230,#57231,
#57232,#57233,#57234,#57235,#57236,#57237),.UNSPECIFIED.,.F.,.F.,(4,1,1,
1,1,1,1,1,4),(191.637151868978,191.893711818134,192.8930699517,193.892428085266,
194.891786218832,195.891144352398,196.890502485964,197.88986061953,197.920337176157),
 .UNSPECIFIED.);
#1306=B_SPLINE_CURVE_WITH_KNOTS('',3,(#57238,#57239,#57240,#57241,#57242,
#57243,#57244,#57245,#57246,#57247,#57248),.UNSPECIFIED.,.F.,.F.,(4,1,1,
1,1,1,1,1,4),(191.637151868978,191.864255732803,192.86361386637,193.862971999936,
194.862330133502,195.861688267068,196.861046400634,197.8604045342,197.920337176158),
 .UNSPECIFIED.);
#1307=B_SPLINE_CURVE_WITH_KNOTS('',3,(#57253,#57254,#57255,#57256,#57257,
#57258,#57259,#57260,#57261,#57262),.UNSPECIFIED.,.F.,.F.,(4,1,1,1,1,1,
1,4),(185.353966561798,185.897563016737,186.896921150303,187.89627928387,
188.895637417436,189.894995551002,190.894353684568,191.637151868978),
 .UNSPECIFIED.);
#1308=B_SPLINE_CURVE_WITH_KNOTS('',3,(#57263,#57264,#57265,#57266,#57267,
#57268,#57269,#57270,#57271,#57272),.UNSPECIFIED.,.F.,.F.,(4,1,1,1,1,1,
1,4),(185.353966561799,185.868106931407,186.867465064973,187.866823198539,
188.866181332105,189.865539465671,190.864897599237,191.637151868978),
 .UNSPECIFIED.);
#1309=B_SPLINE_CURVE_WITH_KNOTS('',3,(#57277,#57278,#57279,#57280,#57281,
#57282,#57283,#57284,#57285,#57286),.UNSPECIFIED.,.F.,.F.,(4,1,1,1,1,1,
1,4),(179.070781254619,179.901414215341,180.900772348907,181.900130482473,
182.899488616039,183.898846749605,184.898204883171,185.353966561798),
 .UNSPECIFIED.);
#1310=B_SPLINE_CURVE_WITH_KNOTS('',3,(#57287,#57288,#57289,#57290,#57291,
#57292,#57293,#57294,#57295,#57296),.UNSPECIFIED.,.F.,.F.,(4,1,1,1,1,1,
1,4),(179.070781254619,179.871958130011,180.871316263577,181.870674397143,
182.870032530709,183.869390664275,184.868748797841,185.353966561799),
 .UNSPECIFIED.);
#1311=B_SPLINE_CURVE_WITH_KNOTS('',3,(#57301,#57302,#57303,#57304,#57305,
#57306,#57307,#57308,#57309,#57310,#57311),.UNSPECIFIED.,.F.,.F.,(4,1,1,
1,1,1,1,1,4),(172.787595947439,172.905907280379,173.905265413945,174.904623547511,
175.903981681077,176.903339814643,177.902697948209,178.902056081775,179.070781254619),
 .UNSPECIFIED.);
#1312=B_SPLINE_CURVE_WITH_KNOTS('',3,(#57312,#57313,#57314,#57315,#57316,
#57317,#57318,#57319,#57320,#57321,#57322),.UNSPECIFIED.,.F.,.F.,(4,1,1,
1,1,1,1,1,4),(172.787595947439,172.876451195049,173.875809328615,174.875167462181,
175.874525595747,176.873883729313,177.873241862879,178.872599996445,179.070781254619),
 .UNSPECIFIED.);
#1313=B_SPLINE_CURVE_WITH_KNOTS('',3,(#57327,#57328,#57329,#57330,#57331,
#57332,#57333,#57334,#57335,#57336),.UNSPECIFIED.,.F.,.F.,(4,1,1,1,1,1,
1,4),(166.504410640259,166.909758478983,167.909116612549,168.908474746115,
169.907832879681,170.907191013247,171.906549146813,172.787595947439),
 .UNSPECIFIED.);
#1314=B_SPLINE_CURVE_WITH_KNOTS('',3,(#57337,#57338,#57339,#57340,#57341,
#57342,#57343,#57344,#57345,#57346),.UNSPECIFIED.,.F.,.F.,(4,1,1,1,1,1,
1,4),(166.50441064026,166.880302393652,167.879660527218,168.879018660784,
169.87837679435,170.877734927916,171.877093061483,172.787595947439),
 .UNSPECIFIED.);
#1315=B_SPLINE_CURVE_WITH_KNOTS('',3,(#57351,#57352,#57353,#57354,#57355,
#57356,#57357,#57358,#57359,#57360),.UNSPECIFIED.,.F.,.F.,(4,1,1,1,1,1,
1,4),(160.22122533308,160.913609677586,161.912967811152,162.912325944718,
163.911684078284,164.91104221185,165.910400345416,166.504410640259),
 .UNSPECIFIED.);
#1316=B_SPLINE_CURVE_WITH_KNOTS('',3,(#57361,#57362,#57363,#57364,#57365,
#57366,#57367,#57368,#57369,#57370),.UNSPECIFIED.,.F.,.F.,(4,1,1,1,1,1,
1,4),(160.22122533308,160.884153592256,161.883511725822,162.882869859388,
163.882227992954,164.88158612652,165.880944260086,166.50441064026),
 .UNSPECIFIED.);
#1317=B_SPLINE_CURVE_WITH_KNOTS('',3,(#57375,#57376,#57377,#57378,#57379,
#57380,#57381,#57382,#57383,#57384),.UNSPECIFIED.,.F.,.F.,(4,1,1,1,1,1,
1,4),(153.9380400259,154.91746087619,155.916819009756,156.916177143322,
157.915535276888,158.914893410454,159.91425154402,160.22122533308),
 .UNSPECIFIED.);
#1318=B_SPLINE_CURVE_WITH_KNOTS('',3,(#57385,#57386,#57387,#57388,#57389,
#57390,#57391,#57392,#57393,#57394),.UNSPECIFIED.,.F.,.F.,(4,1,1,1,1,1,
1,4),(153.938040025901,154.88800479086,155.887362924426,156.886721057992,
157.886079191558,158.885437325124,159.88479545869,160.22122533308),
 .UNSPECIFIED.);
#1319=B_SPLINE_CURVE_WITH_KNOTS('',3,(#57399,#57400,#57401,#57402,#57403,
#57404,#57405,#57406,#57407,#57408,#57409),.UNSPECIFIED.,.F.,.F.,(4,1,1,
1,1,1,1,1,4),(147.654854718721,147.921953941228,148.921312074794,149.92067020836,
150.920028341926,151.919386475492,152.918744609058,153.918102742624,153.9380400259),
 .UNSPECIFIED.);
#1320=B_SPLINE_CURVE_WITH_KNOTS('',3,(#57410,#57411,#57412,#57413,#57414,
#57415,#57416,#57417,#57418,#57419,#57420),.UNSPECIFIED.,.F.,.F.,(4,1,1,
1,1,1,1,1,4),(147.654854718721,147.892497855897,148.891855989463,149.891214123029,
150.890572256596,151.889930390162,152.889288523728,153.888646657294,153.938040025901),
 .UNSPECIFIED.);
#1321=B_SPLINE_CURVE_WITH_KNOTS('',3,(#57425,#57426,#57427,#57428,#57429,
#57430,#57431,#57432,#57433,#57434),.UNSPECIFIED.,.F.,.F.,(4,1,1,1,1,1,
1,4),(141.371669411541,141.925805139831,142.925163273397,143.924521406963,
144.92387954053,145.923237674096,146.922595807662,147.654854718721),
 .UNSPECIFIED.);
#1322=B_SPLINE_CURVE_WITH_KNOTS('',3,(#57435,#57436,#57437,#57438,#57439,
#57440,#57441,#57442,#57443,#57444),.UNSPECIFIED.,.F.,.F.,(4,1,1,1,1,1,
1,4),(141.371669411542,141.896349054501,142.895707188067,143.895065321633,
144.894423455199,145.893781588765,146.893139722331,147.654854718721),
 .UNSPECIFIED.);
#1323=B_SPLINE_CURVE_WITH_KNOTS('',3,(#57449,#57450,#57451,#57452,#57453,
#57454,#57455,#57456,#57457,#57458),.UNSPECIFIED.,.F.,.F.,(4,1,1,1,1,1,
1,4),(135.088484104362,135.929656338435,136.929014472001,137.928372605567,
138.927730739133,139.927088872699,140.926447006265,141.371669411541),
 .UNSPECIFIED.);
#1324=B_SPLINE_CURVE_WITH_KNOTS('',3,(#57459,#57460,#57461,#57462,#57463,
#57464,#57465,#57466,#57467,#57468),.UNSPECIFIED.,.F.,.F.,(4,1,1,1,1,1,
1,4),(135.088484104362,135.900200253105,136.899558386671,137.898916520237,
138.898274653803,139.897632787369,140.896990920935,141.371669411542),
 .UNSPECIFIED.);
#1325=B_SPLINE_CURVE_WITH_KNOTS('',3,(#57473,#57474,#57475,#57476,#57477,
#57478,#57479,#57480,#57481,#57482,#57483),.UNSPECIFIED.,.F.,.F.,(4,1,1,
1,1,1,1,1,4),(128.805298797182,128.934149403473,129.933507537039,130.932865670605,
131.932223804171,132.931581937737,133.930940071303,134.930298204869,135.088484104362),
 .UNSPECIFIED.);
#1326=B_SPLINE_CURVE_WITH_KNOTS('',3,(#57484,#57485,#57486,#57487,#57488,
#57489,#57490,#57491,#57492,#57493,#57494),.UNSPECIFIED.,.F.,.F.,(4,1,1,
1,1,1,1,1,4),(128.805298797182,128.904693318142,129.904051451709,130.903409585275,
131.902767718841,132.902125852407,133.901483985973,134.900842119539,135.088484104362),
 .UNSPECIFIED.);
#1327=B_SPLINE_CURVE_WITH_KNOTS('',3,(#57499,#57500,#57501,#57502,#57503,
#57504,#57505,#57506,#57507,#57508),.UNSPECIFIED.,.F.,.F.,(4,1,1,1,1,1,
1,4),(122.522113490002,122.938000602077,123.937358735643,124.936716869209,
125.936075002775,126.935433136341,127.934791269907,128.805298797182),
 .UNSPECIFIED.);
#1328=B_SPLINE_CURVE_WITH_KNOTS('',3,(#57509,#57510,#57511,#57512,#57513,
#57514,#57515,#57516,#57517,#57518),.UNSPECIFIED.,.F.,.F.,(4,1,1,1,1,1,
1,4),(122.522113490003,122.908544516746,123.907902650312,124.907260783878,
125.906618917444,126.90597705101,127.905335184576,128.805298797182),
 .UNSPECIFIED.);
#1329=B_SPLINE_CURVE_WITH_KNOTS('',3,(#57523,#57524,#57525,#57526,#57527,
#57528,#57529,#57530,#57531,#57532),.UNSPECIFIED.,.F.,.F.,(4,1,1,1,1,1,
1,4),(116.238928182823,116.94185180068,117.941209934246,118.940568067812,
119.939926201378,120.939284334944,121.93864246851,122.522113490002),
 .UNSPECIFIED.);
#1330=B_SPLINE_CURVE_WITH_KNOTS('',3,(#57533,#57534,#57535,#57536,#57537,
#57538,#57539,#57540,#57541,#57542),.UNSPECIFIED.,.F.,.F.,(4,1,1,1,1,1,
1,4),(116.238928182823,116.91239571535,117.911753848916,118.911111982482,
119.910470116048,120.909828249614,121.90918638318,122.522113490003),
 .UNSPECIFIED.);
#1331=B_SPLINE_CURVE_WITH_KNOTS('',3,(#57547,#57548,#57549,#57550,#57551,
#57552,#57553,#57554,#57555,#57556),.UNSPECIFIED.,.F.,.F.,(4,1,1,1,1,1,
1,4),(109.955742875643,110.945702999284,111.94506113285,112.944419266416,
113.943777399982,114.943135533548,115.942493667114,116.238928182823),
 .UNSPECIFIED.);
#1332=B_SPLINE_CURVE_WITH_KNOTS('',3,(#57557,#57558,#57559,#57560,#57561,
#57562,#57563,#57564,#57565,#57566),.UNSPECIFIED.,.F.,.F.,(4,1,1,1,1,1,
1,4),(109.955742875644,110.916246913954,111.91560504752,112.914963181086,
113.914321314652,114.913679448218,115.913037581784,116.238928182823),
 .UNSPECIFIED.);
#1333=B_SPLINE_CURVE_WITH_KNOTS('',3,(#57571,#57572,#57573,#57574,#57575,
#57576,#57577,#57578,#57579,#57580,#57581),.UNSPECIFIED.,.F.,.F.,(4,1,1,
1,1,1,1,1,4),(103.672557568464,103.950196064322,104.949554197888,105.948912331454,
106.94827046502,107.947628598586,108.946986732152,109.946344865718,109.955742875643),
 .UNSPECIFIED.);
#1334=B_SPLINE_CURVE_WITH_KNOTS('',3,(#57582,#57583,#57584,#57585,#57586,
#57587,#57588,#57589,#57590,#57591,#57592),.UNSPECIFIED.,.F.,.F.,(4,1,1,
1,1,1,1,1,4),(103.672557568464,103.920739978991,104.920098112557,105.919456246123,
106.918814379689,107.918172513255,108.917530646822,109.916888780388,109.955742875644),
 .UNSPECIFIED.);
#1335=B_SPLINE_CURVE_WITH_KNOTS('',3,(#57597,#57598,#57599,#57600,#57601,
#57602,#57603,#57604,#57605,#57606),.UNSPECIFIED.,.F.,.F.,(4,1,1,1,1,1,
1,4),(97.3893722612841,97.9540472629253,98.9534053964914,99.9527635300574,
100.952121663623,101.95147979719,102.950837930756,103.672557568464),
 .UNSPECIFIED.);
#1336=B_SPLINE_CURVE_WITH_KNOTS('',3,(#57607,#57608,#57609,#57610,#57611,
#57612,#57613,#57614,#57615,#57616),.UNSPECIFIED.,.F.,.F.,(4,1,1,1,1,1,
1,4),(97.3893722612845,97.924591177595,98.9239493111611,99.9233074447271,
100.922665578293,101.922023711859,102.921381845425,103.672557568464),
 .UNSPECIFIED.);
#1337=B_SPLINE_CURVE_WITH_KNOTS('',3,(#57621,#57622,#57623,#57624,#57625,
#57626,#57627,#57628,#57629,#57630),.UNSPECIFIED.,.F.,.F.,(4,1,1,1,1,1,
1,4),(91.1061869541045,91.9578984615291,92.9572565950951,93.9566147286612,
94.9559728622272,95.9553309957932,96.9546891293593,97.3893722612841),
 .UNSPECIFIED.);
#1338=B_SPLINE_CURVE_WITH_KNOTS('',3,(#57631,#57632,#57633,#57634,#57635,
#57636,#57637,#57638,#57639,#57640),.UNSPECIFIED.,.F.,.F.,(4,1,1,1,1,1,
1,4),(91.1061869541048,91.9284423761987,92.9278005097648,93.9271586433308,
94.9265167768969,95.9258749104629,96.925233044029,97.3893722612845),
 .UNSPECIFIED.);
#1339=B_SPLINE_CURVE_WITH_KNOTS('',3,(#57645,#57646,#57647,#57648,#57649,
#57650,#57651,#57652,#57653,#57654,#57655),.UNSPECIFIED.,.F.,.F.,(4,1,1,
1,1,1,1,1,4),(84.8230016469249,84.9623915265667,85.9617496601328,86.9611077936988,
87.9604659272649,88.9598240608309,89.959182194397,90.958540327963,91.1061869541045),
 .UNSPECIFIED.);
#1340=B_SPLINE_CURVE_WITH_KNOTS('',3,(#57656,#57657,#57658,#57659,#57660,
#57661,#57662,#57663,#57664,#57665,#57666),.UNSPECIFIED.,.F.,.F.,(4,1,1,
1,1,1,1,1,4),(84.8230016469253,84.9329354412364,85.9322935748025,86.9316517083685,
87.9310098419346,88.9303679755006,89.9297261090666,90.9290842426327,91.1061869541048),
 .UNSPECIFIED.);
#1341=B_SPLINE_CURVE_WITH_KNOTS('',3,(#57671,#57672,#57673,#57674,#57675,
#57676,#57677,#57678,#57679,#57680),.UNSPECIFIED.,.F.,.F.,(4,1,1,1,1,1,
1,4),(78.5398163397454,78.9662427251705,79.9656008587365,80.9649589923026,
81.9643171258686,82.9636752594347,83.9630333930007,84.8230016469249),
 .UNSPECIFIED.);
#1342=B_SPLINE_CURVE_WITH_KNOTS('',3,(#57681,#57682,#57683,#57684,#57685,
#57686,#57687,#57688,#57689,#57690),.UNSPECIFIED.,.F.,.F.,(4,1,1,1,1,1,
1,4),(78.5398163397457,78.9367866398401,79.9361447734062,80.9355029069722,
81.9348610405383,82.9342191741043,83.9335773076704,84.8230016469253),
 .UNSPECIFIED.);
#1343=B_SPLINE_CURVE_WITH_KNOTS('',3,(#57695,#57696,#57697,#57698,#57699,
#57700,#57701,#57702,#57703,#57704),.UNSPECIFIED.,.F.,.F.,(4,1,1,1,1,1,
1,4),(72.2566310325658,72.9700939237742,73.9694520573402,74.9688101909063,
75.9681683244723,76.9675264580384,77.9668845916044,78.5398163397454),
 .UNSPECIFIED.);
#1344=B_SPLINE_CURVE_WITH_KNOTS('',3,(#57705,#57706,#57707,#57708,#57709,
#57710,#57711,#57712,#57713,#57714),.UNSPECIFIED.,.F.,.F.,(4,1,1,1,1,1,
1,4),(72.2566310325661,72.9406378384438,73.9399959720099,74.9393541055759,
75.938712239142,76.938070372708,77.9374285062741,78.5398163397457),
 .UNSPECIFIED.);
#1345=B_SPLINE_CURVE_WITH_KNOTS('',3,(#57719,#57720,#57721,#57722,#57723,
#57724,#57725,#57726,#57727,#57728,#57729),.UNSPECIFIED.,.F.,.F.,(4,1,1,
1,1,1,1,1,4),(65.9734457253862,65.9745869888119,66.9739451223779,67.9733032559439,
68.97266138951,69.972019523076,70.9713776566421,71.9707357902081,72.2566310325658),
 .UNSPECIFIED.);
#1346=B_SPLINE_CURVE_WITH_KNOTS('',3,(#57730,#57731,#57732,#57733,#57734,
#57735,#57736,#57737,#57738,#57739),.UNSPECIFIED.,.F.,.F.,(4,1,1,1,1,1,
1,4),(65.9734457253865,66.9444890370476,67.9438471706136,68.9432053041797,
69.9425634377457,70.9419215713118,71.9412797048778,72.2566310325661),
 .UNSPECIFIED.);
#1347=B_SPLINE_CURVE_WITH_KNOTS('',3,(#57744,#57745,#57746,#57747,#57748,
#57749,#57750,#57751,#57752,#57753,#57754,#57755),.UNSPECIFIED.,.F.,.F.,
(4,1,1,1,1,1,1,1,1,4),(59.6902604182066,59.9784381874156,60.4781172541986,
60.9777963209816,61.4774753877646,61.9771544545477,62.9765125881137,63.9758707216798,
64.9752288552458,65.9734457253862),.UNSPECIFIED.);
#1348=B_SPLINE_CURVE_WITH_KNOTS('',3,(#57756,#57757,#57758,#57759,#57760,
#57761,#57762,#57763,#57764,#57765,#57766),.UNSPECIFIED.,.F.,.F.,(4,1,1,
1,1,1,1,1,4),(59.6902604182069,59.9489821020852,60.9483402356513,61.9476983692173,
62.9470565027834,63.9464146363494,64.9457727699155,65.9451309034815,65.9734457253865),
 .UNSPECIFIED.);
#1349=B_SPLINE_CURVE_WITH_KNOTS('',3,(#57771,#57772,#57773,#57774,#57775,
#57776,#57777,#57778,#57779,#57780,#57781,#57782,#57783,#57784,#57785,#57786,
#57787),.UNSPECIFIED.,.F.,.F.,(4,1,1,1,1,1,1,1,1,1,1,1,1,1,4),(53.407075111027,
53.4826103192363,53.9822893860193,54.4819684528023,54.9816475195853,55.4813265863684,
55.9810056531514,56.4806847199344,56.9803637867174,57.4800428535005,57.9797219202835,
58.4794009870665,58.9790800538495,59.4787591206325,59.6902604182066),
 .UNSPECIFIED.);
#1350=B_SPLINE_CURVE_WITH_KNOTS('',3,(#57788,#57789,#57790,#57791,#57792,
#57793,#57794,#57795,#57796,#57797,#57798,#57799,#57800,#57801,#57802,#57803),
 .UNSPECIFIED.,.F.,.F.,(4,1,1,1,1,1,1,1,1,1,1,1,1,4),(53.4070751110273,
53.4531542339059,53.9528333006889,54.452512367472,54.952191434255,55.451870501038,
55.951549567821,56.4512286346041,56.9509077013871,57.4505867681701,57.9502658349531,
58.4499449017362,58.9496239685192,59.6902604182069),.UNSPECIFIED.);
#1351=B_SPLINE_CURVE_WITH_KNOTS('',3,(#57808,#57809,#57810,#57811,#57812,
#57813,#57814,#57815,#57816,#57817,#57818,#57819,#57820,#57821,#57822,#57823),
 .UNSPECIFIED.,.F.,.F.,(4,1,1,1,1,1,1,1,1,1,1,1,1,4),(47.1238898038474,
47.48646151784,47.986140584623,48.485819651406,48.9854987181891,49.4851777849721,
49.9848568517551,50.4845359185381,50.9842149853212,51.4838940521042,51.9835731188872,
52.4832521856702,52.9829312524532,53.407075111027),.UNSPECIFIED.);
#1352=B_SPLINE_CURVE_WITH_KNOTS('',3,(#57824,#57825,#57826,#57827,#57828,
#57829,#57830,#57831,#57832,#57833,#57834,#57835,#57836,#57837,#57838,#57839),
 .UNSPECIFIED.,.F.,.F.,(4,1,1,1,1,1,1,1,1,1,1,1,1,4),(47.1238898038477,
47.4570054325096,47.9566844992927,48.4563635660757,48.9560426328587,49.4557216996417,
49.9554007664248,50.4550798332078,50.9547588999908,51.4544379667738,51.9541170335568,
52.4537961003399,52.9534751671229,53.4070751110273),.UNSPECIFIED.);
#1353=B_SPLINE_CURVE_WITH_KNOTS('',3,(#57844,#57845,#57846,#57847,#57848,
#57849,#57850,#57851,#57852,#57853,#57854,#57855,#57856,#57857,#57858,#57859,
#57860),.UNSPECIFIED.,.F.,.F.,(4,1,1,1,1,1,1,1,1,1,1,1,1,1,4),(40.8407044966678,
40.9906336496607,41.4903127164437,41.9899917832267,42.4896708500098,42.9893499167928,
43.4890289835758,43.9887080503588,44.4883871171419,44.9880661839249,45.4877452507079,
45.9874243174909,46.4871033842739,46.986782451057,47.1238898038474),
 .UNSPECIFIED.);
#1354=B_SPLINE_CURVE_WITH_KNOTS('',3,(#57861,#57862,#57863,#57864,#57865,
#57866,#57867,#57868,#57869,#57870,#57871,#57872,#57873,#57874,#57875,#57876,
#57877),.UNSPECIFIED.,.F.,.F.,(4,1,1,1,1,1,1,1,1,1,1,1,1,1,4),(40.8407044966681,
40.9611775643303,41.4608566311134,41.9605356978964,42.4602147646794,42.9598938314624,
43.4595728982454,43.9592519650285,44.4589310318115,44.9586100985945,45.4582891653775,
45.9579682321606,46.4576472989436,46.9573263657266,47.1238898038477),
 .UNSPECIFIED.);
#1355=B_SPLINE_CURVE_WITH_KNOTS('',3,(#57882,#57883,#57884,#57885,#57886,
#57887,#57888,#57889,#57890,#57891,#57892,#57893,#57894,#57895,#57896,#57897),
 .UNSPECIFIED.,.F.,.F.,(4,1,1,1,1,1,1,1,1,1,1,1,1,4),(34.5575191894882,
34.9944848482644,35.4941639150474,35.9938429818305,36.4935220486135,36.9932011153965,
37.4928801821795,37.9925592489626,38.4922383157456,38.9919173825286,39.4915964493116,
39.9912755160946,40.4909545828777,40.8407044966678),.UNSPECIFIED.);
#1356=B_SPLINE_CURVE_WITH_KNOTS('',3,(#57898,#57899,#57900,#57901,#57902,
#57903,#57904,#57905,#57906,#57907,#57908,#57909,#57910,#57911,#57912,#57913),
 .UNSPECIFIED.,.F.,.F.,(4,1,1,1,1,1,1,1,1,1,1,1,1,4),(34.5575191894886,
34.965028762934,35.4647078297171,35.9643868965001,36.4640659632831,36.9637450300661,
37.4634240968492,37.9631031636322,38.4627822304152,38.9624612971982,39.4621403639813,
39.9618194307643,40.4614984975473,40.8407044966681),.UNSPECIFIED.);
#1357=B_SPLINE_CURVE_WITH_KNOTS('',3,(#57918,#57919,#57920,#57921,#57922,
#57923,#57924,#57925,#57926,#57927,#57928,#57929,#57930,#57931,#57932,#57933,
#57934),.UNSPECIFIED.,.F.,.F.,(4,1,1,1,1,1,1,1,1,1,1,1,1,1,4),(28.2743338823086,
28.4986569800851,28.9983360468681,29.4980151136512,29.9976941804342,30.4973732472172,
30.9970523140002,31.4967313807832,31.9964104475663,32.4960895143493,32.9957685811323,
33.4954476479153,33.9951267146984,34.4948057814814,34.5575191894882),
 .UNSPECIFIED.);
#1358=B_SPLINE_CURVE_WITH_KNOTS('',3,(#57935,#57936,#57937,#57938,#57939,
#57940,#57941,#57942,#57943,#57944,#57945,#57946,#57947,#57948,#57949,#57950,
#57951),.UNSPECIFIED.,.F.,.F.,(4,1,1,1,1,1,1,1,1,1,1,1,1,1,4),(28.2743338823089,
28.4692008947547,28.9688799615378,29.4685590283208,29.9682380951038,30.4679171618868,
30.9675962286699,31.4672752954529,31.9669543622359,32.4666334290189,32.966312495802,
33.465991562585,33.965670629368,34.465349696151,34.5575191894886),
 .UNSPECIFIED.);
#1359=B_SPLINE_CURVE_WITH_KNOTS('',3,(#57956,#57957,#57958,#57959,#57960,
#57961,#57962,#57963,#57964,#57965,#57966,#57967,#57968,#57969,#57970,#57971,
#57972),.UNSPECIFIED.,.F.,.F.,(4,1,1,1,1,1,1,1,1,1,1,1,1,1,4),(21.991148575129,
22.0028291119058,22.5025081786888,23.0021872454719,23.5018663122549,24.0015453790379,
24.5012244458209,25.0009035126039,25.500582579387,26.00026164617,26.499940712953,
26.999619779736,27.4992988465191,27.9989779133021,28.2743338823086),
 .UNSPECIFIED.);
#1360=B_SPLINE_CURVE_WITH_KNOTS('',3,(#57973,#57974,#57975,#57976,#57977,
#57978,#57979,#57980,#57981,#57982,#57983,#57984,#57985,#57986,#57987,#57988),
 .UNSPECIFIED.,.F.,.F.,(4,1,1,1,1,1,1,1,1,1,1,1,1,4),(21.9911485751294,
22.4730520933585,22.9727311601415,23.4724102269245,23.9720892937075,24.4717683604905,
24.9714474272736,25.4711264940566,25.9708055608396,26.4704846276226,26.9701636944057,
27.4698427611887,27.9695218279717,28.2743338823089),.UNSPECIFIED.);
#1361=B_SPLINE_CURVE_WITH_KNOTS('',3,(#57993,#57994,#57995,#57996,#57997,
#57998,#57999,#58000,#58001,#58002,#58003,#58004,#58005,#58006,#58007,#58008),
 .UNSPECIFIED.,.F.,.F.,(4,1,1,1,1,1,1,1,1,1,1,1,1,4),(15.7079632679495,
16.0066803105095,16.5063593772925,17.0060384440756,17.5057175108586,18.0053965776416,
18.5050756444246,19.0047547112077,19.5044337779907,20.0041128447737,20.5037919115567,
21.0034709783398,21.5031500451228,21.991148575129),.UNSPECIFIED.);
#1362=B_SPLINE_CURVE_WITH_KNOTS('',3,(#58009,#58010,#58011,#58012,#58013,
#58014,#58015,#58016,#58017,#58018,#58019,#58020,#58021,#58022,#58023,#58024,
#58025),.UNSPECIFIED.,.F.,.F.,(4,1,1,1,1,1,1,1,1,1,1,1,1,1,4),(15.7079632679498,
15.9772242251791,16.4769032919622,16.9765823587452,17.4762614255282,17.9759404923112,
18.4756195590943,18.9752986258773,19.4749776926603,19.9746567594433,20.4743358262264,
20.9740148930094,21.4736939597924,21.9733730265754,21.9911485751294),
 .UNSPECIFIED.);
#1363=B_SPLINE_CURVE_WITH_KNOTS('',3,(#58030,#58031,#58032,#58033,#58034,
#58035,#58036,#58037,#58038,#58039,#58040,#58041,#58042,#58043,#58044,#58045,
#58046,#58047,#58048,#58049,#58050,#58051,#58052,#58053,#58054,#58055,#58056,
#58057,#58058,#58059,#58060,#58061,#58062,#58063,#58064,#58065,#58066),
 .UNSPECIFIED.,.F.,.F.,(4,3,3,3,3,3,3,3,3,3,3,3,4),(0.,0.000373494560508806,
0.0620760815771024,0.112839239637108,0.153038169722591,0.175804963675793,
0.247183842626883,0.319084136954533,0.344742425233931,0.363606980156396,
0.439518700737557,0.51795432283266,0.534785019937482),.UNSPECIFIED.);
#1364=B_SPLINE_CURVE_WITH_KNOTS('',3,(#58068,#58069,#58070,#58071,#58072,
#58073,#58074,#58075,#58076,#58077,#58078,#58079,#58080,#58081,#58082,#58083,
#58084,#58085,#58086,#58087,#58088,#58089,#58090,#58091,#58092,#58093,#58094,
#58095,#58096,#58097,#58098,#58099,#58100,#58101,#58102,#58103,#58104),
 .UNSPECIFIED.,.F.,.F.,(4,3,3,3,3,3,3,3,3,3,3,3,4),(0.,0.000511892384038064,
0.078754853834616,0.155070466132989,0.20164291816609,0.227017770490094,
0.290460834304131,0.352619921814331,0.383703668213755,0.403796492255862,
0.466621120797767,0.52704524650008,0.539097184344933),.UNSPECIFIED.);
#1365=B_SPLINE_CURVE_WITH_KNOTS('',3,(#60104,#60105,#60106,#60107,#60108,
#60109,#60110,#60111,#60112,#60113,#60114,#60115,#60116,#60117,#60118,#60119,
#60120,#60121,#60122,#60123,#60124,#60125,#60126,#60127,#60128,#60129,#60130,
#60131,#60132,#60133,#60134,#60135,#60136,#60137,#60138,#60139,#60140,#60141,
#60142,#60143),.UNSPECIFIED.,.F.,.F.,(4,3,3,3,3,3,3,3,3,3,3,3,3,4),(-0.53478501993692,
-0.534277081309421,-0.456439695901019,-0.38064245929011,-0.348102919117109,
-0.328886681298388,-0.258595553176405,-0.246742105655551,-0.185056579241663,
-0.163339235199672,-0.143463957830519,-0.0808484674142256,-0.0206857924044652,
0.),.UNSPECIFIED.);
#1366=B_SPLINE_CURVE_WITH_KNOTS('',3,(#60144,#60145,#60146,#60147,#60148,
#60149,#60150,#60151,#60152,#60153,#60154,#60155,#60156,#60157,#60158,#60159,
#60160,#60161,#60162,#60163,#60164,#60165,#60166,#60167,#60168),
 .UNSPECIFIED.,.F.,.F.,(4,3,3,3,3,3,3,3,4),(390.000549715688,390.249351157541,
390.749030224325,391.248709291108,391.748388357891,392.248067424674,392.747746491457,
393.24742555824,393.746279249921),.UNSPECIFIED.);
#1367=B_SPLINE_CURVE_WITH_KNOTS('',3,(#60169,#60170,#60171,#60172,#60173,
#60174,#60175,#60176,#60177,#60178,#60179,#60180,#60181,#60182,#60183),
 .UNSPECIFIED.,.F.,.F.,(4,1,1,1,1,1,1,1,1,1,1,1,4),(9.98190079888485,10.4807544905659,
10.9804335573489,11.4801126241319,11.979791690915,12.479470757698,12.979149824481,
13.478828891264,13.9785079580471,14.4781870248301,14.9778660916131,15.4775451583961,
15.7079632679498),.UNSPECIFIED.);
#1368=B_SPLINE_CURVE_WITH_KNOTS('',3,(#60185,#60186,#60187,#60188,#60189,
#60190,#60191,#60192,#60193,#60194,#60195),.UNSPECIFIED.,.F.,.F.,(4,1,1,
1,1,1,1,1,4),(12.0092477762453,12.5089268430284,13.0086059098114,13.5082849765944,
14.0079640433774,14.5076431101605,15.0073221769435,15.5070012437265,15.7079632679495),
 .UNSPECIFIED.);
#1369=B_SPLINE_CURVE_WITH_KNOTS('',3,(#62189,#62190,#62191,#62192,#62193,
#62194,#62195,#62196,#62197,#62198,#62199,#62200,#62201,#62202,#62203,#62204,
#62205,#62206,#62207,#62208,#62209,#62210,#62211,#62212,#62213,#62214,#62215,
#62216,#62217,#62218,#62219,#62220,#62221,#62222,#62223,#62224,#62225,#62226,
#62227,#62228),.UNSPECIFIED.,.F.,.F.,(4,3,3,3,3,3,3,3,3,3,3,3,3,4),(-0.539097184344981,
-0.538720824057998,-0.476544551511477,-0.429912347101587,-0.401091234701428,
-0.381803774975435,-0.313681369269712,-0.290015733871917,-0.24230273417063,
-0.214804629165427,-0.192593514291413,-0.116696500404398,-0.0381316372362206,
0.),.UNSPECIFIED.);
#1370=B_SPLINE_CURVE_WITH_KNOTS('',3,(#62229,#62230,#62231,#62232,#62233,
#62234,#62235,#62236,#62237,#62238),.UNSPECIFIED.,.F.,.F.,(4,3,3,4),(-394.746462758588,
-394.246783691805,-393.747104625022,-393.256204536838),.UNSPECIFIED.);
#1371=B_SPLINE_CURVE_WITH_KNOTS('',3,(#62305,#62306,#62307,#62308,#62309,
#62310,#62311,#62312),.UNSPECIFIED.,.F.,.F.,(4,2,2,4),(0.756005737987019,
0.793568827564653,0.872922520054208,0.952276212543762),.UNSPECIFIED.);
#1372=B_SPLINE_CURVE_WITH_KNOTS('',3,(#62315,#62316,#62317,#62318,#62319,
#62320,#62321,#62322,#62323,#62324,#62325,#62326,#62327,#62328),
 .UNSPECIFIED.,.F.,.F.,(4,2,2,2,2,2,4),(0.121154929624509,0.158718019202145,
0.238071711691699,0.317425404181254,0.396779096670809,0.476132789160363,
0.513695878738001),.UNSPECIFIED.);
#1373=B_SPLINE_CURVE_WITH_KNOTS('',3,(#62329,#62330,#62331,#62332,#62333,
#62334,#62335,#62336),.UNSPECIFIED.,.F.,.F.,(4,2,2,4),(0.952276212543762,
1.03162990503332,1.11098359752287,1.14854668710052),.UNSPECIFIED.);
#1374=B_SPLINE_CURVE_WITH_KNOTS('',3,(#62340,#62341,#62342,#62343,#62344,
#62345,#62346,#62347,#62348,#62349),.UNSPECIFIED.,.F.,.F.,(4,2,2,2,4),(0.,
0.0792165807733642,0.158433161546728,0.237648697074572,0.316864232602417),
 .UNSPECIFIED.);
#1375=B_SPLINE_CURVE_WITH_KNOTS('',3,(#62350,#62351,#62352,#62353,#62354,
#62355,#62356,#62357,#62358,#62359,#62360,#62361,#62362,#62363,#62364,#62365,
#62366,#62367,#62368,#62369,#62370,#62371,#62372,#62373,#62374,#62375),
 .UNSPECIFIED.,.F.,.F.,(4,2,2,2,2,2,2,2,2,2,2,2,4),(0.316864232602417,0.396079768130261,
0.475295303658105,0.554511884431469,0.633728465204833,0.712945045978197,
0.792161626751562,0.871377162279406,0.95059269780725,1.02980823333509,1.10902376886294,
1.1882403496363,1.26745693040967),.UNSPECIFIED.);
#1376=B_SPLINE_CURVE_WITH_KNOTS('',3,(#62407,#62408,#62409,#62410,#62411,
#62412),.UNSPECIFIED.,.F.,.F.,(4,2,4),(0.803821788694078,0.872950991853625,
0.952307212900975),.UNSPECIFIED.);
#1377=B_SPLINE_CURVE_WITH_KNOTS('',3,(#62415,#62416,#62417,#62418,#62419,
#62420,#62421,#62422,#62423,#62424),.UNSPECIFIED.,.F.,.F.,(4,2,2,2,4),(0.168950313426762,
0.238079516586309,0.317435737633658,0.396791958681008,0.465921161840561),
 .UNSPECIFIED.);
#1378=B_SPLINE_CURVE_WITH_KNOTS('',3,(#62425,#62426,#62427,#62428,#62429,
#62430),.UNSPECIFIED.,.F.,.F.,(4,2,4),(0.952307212900975,1.03166343394832,
1.10079263710787),.UNSPECIFIED.);
#1379=B_SPLINE_CURVE_WITH_KNOTS('',3,(#62434,#62435,#62436,#62437,#62438,
#62439,#62440,#62441,#62442,#62443),.UNSPECIFIED.,.F.,.F.,(4,2,2,2,4),(0.,
0.0792165807733642,0.158433161546728,0.237648697074572,0.316864232602417),
 .UNSPECIFIED.);
#1380=B_SPLINE_CURVE_WITH_KNOTS('',3,(#62444,#62445,#62446,#62447,#62448,
#62449,#62450,#62451,#62452,#62453,#62454,#62455,#62456,#62457,#62458,#62459,
#62460,#62461,#62462,#62463,#62464,#62465,#62466,#62467,#62468,#62469),
 .UNSPECIFIED.,.F.,.F.,(4,2,2,2,2,2,2,2,2,2,2,2,4),(0.316864232602417,0.396079768130261,
0.475295303658105,0.554511884431469,0.633728465204833,0.712945045978197,
0.792161626751562,0.871377162279406,0.95059269780725,1.02980823333509,1.10902376886294,
1.1882403496363,1.26745693040967),.UNSPECIFIED.);
#1381=SPHERICAL_SURFACE('',#24327,0.29765);
#1382=SPHERICAL_SURFACE('',#24329,0.29765);
#1383=SPHERICAL_SURFACE('',#24331,0.29765);
#1384=SPHERICAL_SURFACE('',#24333,0.29765);
#1385=SPHERICAL_SURFACE('',#24335,0.29765);
#1386=SPHERICAL_SURFACE('',#24337,0.29765);
#1387=SPHERICAL_SURFACE('',#24339,0.29765);
#1388=SPHERICAL_SURFACE('',#24342,0.309556);
#1389=SPHERICAL_SURFACE('',#24358,0.309556);
#1390=SPHERICAL_SURFACE('',#24363,0.309556);
#1391=SPHERICAL_SURFACE('',#24369,0.309556);
#1392=SPHERICAL_SURFACE('',#24374,0.309556);
#1393=SPHERICAL_SURFACE('',#24379,0.309556);
#1394=SPHERICAL_SURFACE('',#24387,0.309556);
#1395=SPHERICAL_SURFACE('',#24455,0.3969);
#1396=SPHERICAL_SURFACE('',#24457,0.3969);
#1397=SPHERICAL_SURFACE('',#24459,0.3969);
#1398=SPHERICAL_SURFACE('',#24461,0.3969);
#1399=SPHERICAL_SURFACE('',#24463,0.3969);
#1400=SPHERICAL_SURFACE('',#24465,0.3969);
#1401=SPHERICAL_SURFACE('',#24467,0.3969);
#1402=SPHERICAL_SURFACE('',#24469,0.3969);
#1403=SPHERICAL_SURFACE('',#24472,0.412776);
#1404=SPHERICAL_SURFACE('',#24488,0.412776);
#1405=SPHERICAL_SURFACE('',#24493,0.412776);
#1406=SPHERICAL_SURFACE('',#24498,0.412776);
#1407=SPHERICAL_SURFACE('',#24503,0.412776);
#1408=SPHERICAL_SURFACE('',#24508,0.412776);
#1409=SPHERICAL_SURFACE('',#24513,0.412776);
#1410=SPHERICAL_SURFACE('',#24521,0.412776);
#1411=SPHERICAL_SURFACE('',#25572,0.29765);
#1412=SPHERICAL_SURFACE('',#25574,0.29765);
#1413=SPHERICAL_SURFACE('',#25576,0.29765);
#1414=SPHERICAL_SURFACE('',#25578,0.29765);
#1415=SPHERICAL_SURFACE('',#25580,0.29765);
#1416=SPHERICAL_SURFACE('',#25582,0.29765);
#1417=SPHERICAL_SURFACE('',#25584,0.29765);
#1418=SPHERICAL_SURFACE('',#25587,0.309556);
#1419=SPHERICAL_SURFACE('',#25603,0.309556);
#1420=SPHERICAL_SURFACE('',#25608,0.309556);
#1421=SPHERICAL_SURFACE('',#25614,0.309556);
#1422=SPHERICAL_SURFACE('',#25619,0.309556);
#1423=SPHERICAL_SURFACE('',#25624,0.309556);
#1424=SPHERICAL_SURFACE('',#25632,0.309556);
#1425=SPHERICAL_SURFACE('',#25700,0.3969);
#1426=SPHERICAL_SURFACE('',#25702,0.3969);
#1427=SPHERICAL_SURFACE('',#25704,0.3969);
#1428=SPHERICAL_SURFACE('',#25706,0.3969);
#1429=SPHERICAL_SURFACE('',#25708,0.3969);
#1430=SPHERICAL_SURFACE('',#25710,0.3969);
#1431=SPHERICAL_SURFACE('',#25712,0.3969);
#1432=SPHERICAL_SURFACE('',#25714,0.3969);
#1433=SPHERICAL_SURFACE('',#25717,0.412776);
#1434=SPHERICAL_SURFACE('',#25733,0.412776);
#1435=SPHERICAL_SURFACE('',#25738,0.412776);
#1436=SPHERICAL_SURFACE('',#25743,0.412776);
#1437=SPHERICAL_SURFACE('',#25748,0.412776);
#1438=SPHERICAL_SURFACE('',#25753,0.412776);
#1439=SPHERICAL_SURFACE('',#25758,0.412776);
#1440=SPHERICAL_SURFACE('',#25766,0.412776);
#1441=CONICAL_SURFACE('',#24298,0.63,0.785398163397448);
#1442=CONICAL_SURFACE('',#24305,0.63,0.785398163397448);
#1443=CONICAL_SURFACE('',#24318,1.57,0.785398163397449);
#1444=CONICAL_SURFACE('',#24322,1.57,0.785398163397449);
#1445=CONICAL_SURFACE('',#24426,1.05,0.785398163397449);
#1446=CONICAL_SURFACE('',#24433,1.05,0.785398163397449);
#1447=CONICAL_SURFACE('',#24446,2.3,0.785398163397449);
#1448=CONICAL_SURFACE('',#24450,2.3,0.785398163397449);
#1449=CONICAL_SURFACE('',#24714,0.275,0.785398163397449);
#1450=CONICAL_SURFACE('',#24741,0.4,0.785398163397448);
#1451=CONICAL_SURFACE('',#24745,0.41,0.785398163397448);
#1452=CONICAL_SURFACE('',#24749,0.26,0.463647609000806);
#1453=CONICAL_SURFACE('',#24800,0.325,0.785398163397448);
#1454=CONICAL_SURFACE('',#24804,0.335,0.785398163397448);
#1455=CONICAL_SURFACE('',#24808,0.21,0.463647609000806);
#1456=CONICAL_SURFACE('',#24812,0.18,0.785398163397448);
#1457=CONICAL_SURFACE('',#24826,0.4,0.785398163397448);
#1458=CONICAL_SURFACE('',#24830,0.41,0.785398163397448);
#1459=CONICAL_SURFACE('',#24834,0.26,0.463647609000806);
#1460=CONICAL_SURFACE('',#24838,0.225,0.785398163397448);
#1461=CONICAL_SURFACE('',#25111,0.235,0.785398163397448);
#1462=CONICAL_SURFACE('',#25115,0.2125,0.785398163397448);
#1463=CONICAL_SURFACE('',#25130,0.475,0.785398163397449);
#1464=CONICAL_SURFACE('',#25134,0.485,0.785398163397448);
#1465=CONICAL_SURFACE('',#25138,0.31,0.463647609000806);
#1466=CONICAL_SURFACE('',#25142,0.27,0.785398163397448);
#1467=CONICAL_SURFACE('',#25543,0.63,0.785398163397448);
#1468=CONICAL_SURFACE('',#25550,0.63,0.785398163397448);
#1469=CONICAL_SURFACE('',#25563,1.57,0.785398163397449);
#1470=CONICAL_SURFACE('',#25567,1.57,0.785398163397449);
#1471=CONICAL_SURFACE('',#25671,1.05,0.785398163397449);
#1472=CONICAL_SURFACE('',#25678,1.05,0.785398163397449);
#1473=CONICAL_SURFACE('',#25691,2.3,0.785398163397449);
#1474=CONICAL_SURFACE('',#25695,2.3,0.785398163397449);
#1475=CONICAL_SURFACE('',#25805,0.4,0.785398163397448);
#1476=CONICAL_SURFACE('',#25809,0.41,0.785398163397448);
#1477=CONICAL_SURFACE('',#25813,0.26,0.463647609000806);
#1478=CONICAL_SURFACE('',#25971,0.275,0.785398163397449);
#1479=CONICAL_SURFACE('',#25998,0.4,0.785398163397448);
#1480=CONICAL_SURFACE('',#26002,0.41,0.785398163397448);
#1481=CONICAL_SURFACE('',#26006,0.26,0.463647609000806);
#1482=CONICAL_SURFACE('',#26057,0.325,0.785398163397448);
#1483=CONICAL_SURFACE('',#26061,0.335,0.785398163397448);
#1484=CONICAL_SURFACE('',#26065,0.21,0.463647609000806);
#1485=CONICAL_SURFACE('',#26069,0.18,0.785398163397448);
#1486=CONICAL_SURFACE('',#26083,0.4,0.785398163397448);
#1487=CONICAL_SURFACE('',#26087,0.41,0.785398163397448);
#1488=CONICAL_SURFACE('',#26091,0.26,0.463647609000806);
#1489=CONICAL_SURFACE('',#26095,0.225,0.785398163397448);
#1490=CONICAL_SURFACE('',#26368,0.235,0.785398163397448);
#1491=CONICAL_SURFACE('',#26372,0.2125,0.785398163397448);
#1492=CONICAL_SURFACE('',#26387,0.475,0.785398163397449);
#1493=CONICAL_SURFACE('',#26391,0.485,0.785398163397448);
#1494=CONICAL_SURFACE('',#26395,0.31,0.463647609000806);
#1495=CONICAL_SURFACE('',#26399,0.27,0.785398163397448);
#1496=TOROIDAL_SURFACE('',#24287,1.1,0.309556);
#1497=TOROIDAL_SURFACE('',#24307,1.1,0.309556);
#1498=TOROIDAL_SURFACE('',#24415,1.675,0.412776);
#1499=TOROIDAL_SURFACE('',#24435,1.675,0.412776);
#1500=TOROIDAL_SURFACE('',#25532,1.1,0.309556);
#1501=TOROIDAL_SURFACE('',#25552,1.1,0.309556);
#1502=TOROIDAL_SURFACE('',#25660,1.675,0.412776);
#1503=TOROIDAL_SURFACE('',#25680,1.675,0.412776);
#1504=SHAPE_REPRESENTATION_RELATIONSHIP('SRR','None',#63352,#1587);
#1505=SHAPE_REPRESENTATION_RELATIONSHIP('SRR','None',#63353,#1588);
#1506=SHAPE_REPRESENTATION_RELATIONSHIP('SRR','None',#63354,#1589);
#1507=SHAPE_REPRESENTATION_RELATIONSHIP('SRR','None',#63355,#1590);
#1508=SHAPE_REPRESENTATION_RELATIONSHIP('SRR','None',#63356,#1591);
#1509=SHAPE_REPRESENTATION_RELATIONSHIP('SRR','None',#63357,#1592);
#1510=SHAPE_REPRESENTATION_RELATIONSHIP('SRR','None',#63358,#1593);
#1511=SHAPE_REPRESENTATION_RELATIONSHIP('SRR','None',#63359,#1594);
#1512=SHAPE_REPRESENTATION_RELATIONSHIP('SRR','None',#63360,#1595);
#1513=SHAPE_REPRESENTATION_RELATIONSHIP('SRR','None',#63361,#1596);
#1514=SHAPE_REPRESENTATION_RELATIONSHIP('SRR','None',#63362,#1597);
#1515=SHAPE_REPRESENTATION_RELATIONSHIP('SRR','None',#63364,#1598);
#1516=SHAPE_REPRESENTATION_RELATIONSHIP('SRR','None',#63365,#1599);
#1517=SHAPE_REPRESENTATION_RELATIONSHIP('SRR','None',#63366,#1600);
#1518=SHAPE_REPRESENTATION_RELATIONSHIP('SRR','None',#63367,#1601);
#1519=SHAPE_REPRESENTATION_RELATIONSHIP('SRR','None',#63368,#1602);
#1520=SHAPE_REPRESENTATION_RELATIONSHIP('SRR','None',#63370,#1603);
#1521=SHAPE_REPRESENTATION_RELATIONSHIP('SRR','None',#63371,#1604);
#1522=SHAPE_REPRESENTATION_RELATIONSHIP('SRR','None',#63372,#1605);
#1523=SHAPE_REPRESENTATION_RELATIONSHIP('SRR','None',#63373,#1606);
#1524=SHAPE_REPRESENTATION_RELATIONSHIP('SRR','None',#63374,#1607);
#1525=SHAPE_REPRESENTATION_RELATIONSHIP('SRR','None',#63376,#1608);
#1526=SHAPE_REPRESENTATION_RELATIONSHIP('SRR','None',#63377,#1609);
#1527=SHAPE_REPRESENTATION_RELATIONSHIP('SRR','None',#63378,#1610);
#1528=SHAPE_REPRESENTATION_RELATIONSHIP('SRR','None',#63380,#1611);
#1529=SHAPE_REPRESENTATION_RELATIONSHIP('SRR','None',#63381,#1612);
#1530=SHAPE_REPRESENTATION_RELATIONSHIP('SRR','None',#63382,#1613);
#1531=SHAPE_REPRESENTATION_RELATIONSHIP('SRR','None',#63383,#1614);
#1532=SHAPE_REPRESENTATION_RELATIONSHIP('SRR','None',#63384,#1615);
#1533=SHAPE_REPRESENTATION_RELATIONSHIP('SRR','None',#63385,#1616);
#1534=SHAPE_REPRESENTATION_RELATIONSHIP('SRR','None',#63386,#1617);
#1535=SHAPE_REPRESENTATION_RELATIONSHIP('SRR','None',#63387,#1618);
#1536=SHAPE_REPRESENTATION_RELATIONSHIP('SRR','None',#63389,#1619);
#1537=SHAPE_REPRESENTATION_RELATIONSHIP('SRR','None',#63390,#1620);
#1538=SHAPE_REPRESENTATION_RELATIONSHIP('SRR','None',#63391,#1621);
#1539=SHAPE_REPRESENTATION_RELATIONSHIP('SRR','None',#63392,#1622);
#1540=SHAPE_REPRESENTATION_RELATIONSHIP('SRR','None',#63393,#1623);
#1541=SHAPE_REPRESENTATION_RELATIONSHIP('SRR','None',#63394,#1624);
#1542=SHAPE_REPRESENTATION_RELATIONSHIP('SRR','None',#63395,#1625);
#1543=SHAPE_REPRESENTATION_RELATIONSHIP('SRR','None',#63396,#1626);
#1544=SHAPE_REPRESENTATION_RELATIONSHIP('SRR','None',#63397,#1627);
#1545=SHAPE_REPRESENTATION_RELATIONSHIP('SRR','None',#63398,#1628);
#1546=SHAPE_REPRESENTATION_RELATIONSHIP('SRR','None',#63401,#1629);
#1547=SHAPE_REPRESENTATION_RELATIONSHIP('SRR','None',#63402,#1630);
#1548=SHAPE_REPRESENTATION_RELATIONSHIP('SRR','None',#63403,#1631);
#1549=SHAPE_REPRESENTATION_RELATIONSHIP('SRR','None',#63404,#1632);
#1550=SHAPE_REPRESENTATION_RELATIONSHIP('SRR','None',#63405,#1633);
#1551=SHAPE_REPRESENTATION_RELATIONSHIP('SRR','None',#63406,#1634);
#1552=SHAPE_REPRESENTATION_RELATIONSHIP('SRR','None',#63407,#1635);
#1553=SHAPE_REPRESENTATION_RELATIONSHIP('SRR','None',#63408,#1636);
#1554=SHAPE_REPRESENTATION_RELATIONSHIP('SRR','None',#63409,#1637);
#1555=SHAPE_REPRESENTATION_RELATIONSHIP('SRR','None',#63411,#1638);
#1556=SHAPE_REPRESENTATION_RELATIONSHIP('SRR','None',#63412,#1639);
#1557=SHAPE_REPRESENTATION_RELATIONSHIP('SRR','None',#63413,#1640);
#1558=SHAPE_REPRESENTATION_RELATIONSHIP('SRR','None',#63414,#1641);
#1559=SHAPE_REPRESENTATION_RELATIONSHIP('SRR','None',#63415,#1642);
#1560=SHAPE_REPRESENTATION_RELATIONSHIP('SRR','None',#63417,#1643);
#1561=SHAPE_REPRESENTATION_RELATIONSHIP('SRR','None',#63418,#1644);
#1562=SHAPE_REPRESENTATION_RELATIONSHIP('SRR','None',#63419,#1645);
#1563=SHAPE_REPRESENTATION_RELATIONSHIP('SRR','None',#63420,#1646);
#1564=SHAPE_REPRESENTATION_RELATIONSHIP('SRR','None',#63421,#1647);
#1565=SHAPE_REPRESENTATION_RELATIONSHIP('SRR','None',#63422,#1648);
#1566=SHAPE_REPRESENTATION_RELATIONSHIP('SRR','None',#63424,#1649);
#1567=SHAPE_REPRESENTATION_RELATIONSHIP('SRR','None',#63425,#1650);
#1568=SHAPE_REPRESENTATION_RELATIONSHIP('SRR','None',#63426,#1651);
#1569=SHAPE_REPRESENTATION_RELATIONSHIP('SRR','None',#63428,#1652);
#1570=SHAPE_REPRESENTATION_RELATIONSHIP('SRR','None',#63429,#1653);
#1571=SHAPE_REPRESENTATION_RELATIONSHIP('SRR','None',#63430,#1654);
#1572=SHAPE_REPRESENTATION_RELATIONSHIP('SRR','None',#63431,#1655);
#1573=SHAPE_REPRESENTATION_RELATIONSHIP('SRR','None',#63432,#1656);
#1574=SHAPE_REPRESENTATION_RELATIONSHIP('SRR','None',#63433,#1657);
#1575=SHAPE_REPRESENTATION_RELATIONSHIP('SRR','None',#63434,#1658);
#1576=SHAPE_REPRESENTATION_RELATIONSHIP('SRR','None',#63435,#1659);
#1577=SHAPE_REPRESENTATION_RELATIONSHIP('SRR','None',#63437,#1660);
#1578=SHAPE_REPRESENTATION_RELATIONSHIP('SRR','None',#63438,#1661);
#1579=SHAPE_REPRESENTATION_RELATIONSHIP('SRR','None',#63439,#1662);
#1580=SHAPE_REPRESENTATION_RELATIONSHIP('SRR','None',#63440,#1663);
#1581=SHAPE_REPRESENTATION_RELATIONSHIP('SRR','None',#63441,#1664);
#1582=SHAPE_REPRESENTATION_RELATIONSHIP('SRR','None',#63442,#1665);
#1583=SHAPE_REPRESENTATION_RELATIONSHIP('SRR','None',#63443,#1666);
#1584=SHAPE_REPRESENTATION_RELATIONSHIP('SRR','None',#63444,#1667);
#1585=SHAPE_REPRESENTATION_RELATIONSHIP('SRR','None',#63445,#1668);
#1586=SHAPE_REPRESENTATION_RELATIONSHIP('SRR','None',#63446,#1669);
#1587=ADVANCED_BREP_SHAPE_REPRESENTATION('',(#1783),#62889);
#1588=ADVANCED_BREP_SHAPE_REPRESENTATION('',(#1784),#62890);
#1589=ADVANCED_BREP_SHAPE_REPRESENTATION('',(#1785),#62891);
#1590=ADVANCED_BREP_SHAPE_REPRESENTATION('',(#1786),#62892);
#1591=ADVANCED_BREP_SHAPE_REPRESENTATION('',(#1787),#62893);
#1592=ADVANCED_BREP_SHAPE_REPRESENTATION('',(#1788),#62894);
#1593=ADVANCED_BREP_SHAPE_REPRESENTATION('',(#1789),#62895);
#1594=ADVANCED_BREP_SHAPE_REPRESENTATION('',(#1790),#62896);
#1595=ADVANCED_BREP_SHAPE_REPRESENTATION('',(#1791),#62897);
#1596=ADVANCED_BREP_SHAPE_REPRESENTATION('',(#1792),#62898);
#1597=ADVANCED_BREP_SHAPE_REPRESENTATION('',(#1793),#62899);
#1598=ADVANCED_BREP_SHAPE_REPRESENTATION('',(#1794),#62901);
#1599=ADVANCED_BREP_SHAPE_REPRESENTATION('',(#1795),#62902);
#1600=ADVANCED_BREP_SHAPE_REPRESENTATION('',(#1796,#1797,#1798,#1799,#1800,
#1801,#1802),#62903);
#1601=ADVANCED_BREP_SHAPE_REPRESENTATION('',(#1803),#62904);
#1602=ADVANCED_BREP_SHAPE_REPRESENTATION('',(#1804,#1805),#62905);
#1603=ADVANCED_BREP_SHAPE_REPRESENTATION('',(#1806),#62907);
#1604=ADVANCED_BREP_SHAPE_REPRESENTATION('',(#1807),#62908);
#1605=ADVANCED_BREP_SHAPE_REPRESENTATION('',(#1808,#1809,#1810,#1811,#1812,
#1813,#1814,#1815),#62909);
#1606=ADVANCED_BREP_SHAPE_REPRESENTATION('',(#1816),#62910);
#1607=ADVANCED_BREP_SHAPE_REPRESENTATION('',(#1817,#1818),#62911);
#1608=ADVANCED_BREP_SHAPE_REPRESENTATION('',(#1819),#62913);
#1609=ADVANCED_BREP_SHAPE_REPRESENTATION('',(#1820),#62914);
#1610=ADVANCED_BREP_SHAPE_REPRESENTATION('',(#1821),#62915);
#1611=ADVANCED_BREP_SHAPE_REPRESENTATION('',(#1822),#62917);
#1612=ADVANCED_BREP_SHAPE_REPRESENTATION('',(#1823),#62918);
#1613=ADVANCED_BREP_SHAPE_REPRESENTATION('',(#1824),#62919);
#1614=ADVANCED_BREP_SHAPE_REPRESENTATION('',(#1825),#62920);
#1615=ADVANCED_BREP_SHAPE_REPRESENTATION('',(#28),#62921);
#1616=ADVANCED_BREP_SHAPE_REPRESENTATION('',(#1826),#62922);
#1617=ADVANCED_BREP_SHAPE_REPRESENTATION('',(#29),#62923);
#1618=ADVANCED_BREP_SHAPE_REPRESENTATION('',(#30),#62924);
#1619=ADVANCED_BREP_SHAPE_REPRESENTATION('',(#1827),#62926);
#1620=ADVANCED_BREP_SHAPE_REPRESENTATION('',(#1828),#62927);
#1621=ADVANCED_BREP_SHAPE_REPRESENTATION('',(#1829),#62928);
#1622=ADVANCED_BREP_SHAPE_REPRESENTATION('',(#1830),#62929);
#1623=ADVANCED_BREP_SHAPE_REPRESENTATION('',(#1831),#62930);
#1624=ADVANCED_BREP_SHAPE_REPRESENTATION('',(#1832),#62931);
#1625=ADVANCED_BREP_SHAPE_REPRESENTATION('',(#1833),#62932);
#1626=ADVANCED_BREP_SHAPE_REPRESENTATION('',(#1834),#62933);
#1627=ADVANCED_BREP_SHAPE_REPRESENTATION('',(#1835),#62934);
#1628=ADVANCED_BREP_SHAPE_REPRESENTATION('',(#31),#62935);
#1629=ADVANCED_BREP_SHAPE_REPRESENTATION('',(#1836),#62938);
#1630=ADVANCED_BREP_SHAPE_REPRESENTATION('',(#1837),#62939);
#1631=ADVANCED_BREP_SHAPE_REPRESENTATION('',(#1838),#62940);
#1632=ADVANCED_BREP_SHAPE_REPRESENTATION('',(#1839),#62941);
#1633=ADVANCED_BREP_SHAPE_REPRESENTATION('',(#1840),#62942);
#1634=ADVANCED_BREP_SHAPE_REPRESENTATION('',(#1841),#62943);
#1635=ADVANCED_BREP_SHAPE_REPRESENTATION('',(#1842),#62944);
#1636=ADVANCED_BREP_SHAPE_REPRESENTATION('',(#1843),#62945);
#1637=ADVANCED_BREP_SHAPE_REPRESENTATION('',(#1844),#62946);
#1638=ADVANCED_BREP_SHAPE_REPRESENTATION('',(#1845),#62948);
#1639=ADVANCED_BREP_SHAPE_REPRESENTATION('',(#1846),#62949);
#1640=ADVANCED_BREP_SHAPE_REPRESENTATION('',(#1847,#1848,#1849,#1850,#1851,
#1852,#1853),#62950);
#1641=ADVANCED_BREP_SHAPE_REPRESENTATION('',(#1854),#62951);
#1642=ADVANCED_BREP_SHAPE_REPRESENTATION('',(#1855,#1856),#62952);
#1643=ADVANCED_BREP_SHAPE_REPRESENTATION('',(#1857),#62954);
#1644=ADVANCED_BREP_SHAPE_REPRESENTATION('',(#1858),#62955);
#1645=ADVANCED_BREP_SHAPE_REPRESENTATION('',(#1859,#1860,#1861,#1862,#1863,
#1864,#1865,#1866),#62956);
#1646=ADVANCED_BREP_SHAPE_REPRESENTATION('',(#1867),#62957);
#1647=ADVANCED_BREP_SHAPE_REPRESENTATION('',(#1868,#1869),#62958);
#1648=ADVANCED_BREP_SHAPE_REPRESENTATION('',(#32),#62959);
#1649=ADVANCED_BREP_SHAPE_REPRESENTATION('',(#1870),#62961);
#1650=ADVANCED_BREP_SHAPE_REPRESENTATION('',(#1871),#62962);
#1651=ADVANCED_BREP_SHAPE_REPRESENTATION('',(#1872),#62963);
#1652=ADVANCED_BREP_SHAPE_REPRESENTATION('',(#1873),#62965);
#1653=ADVANCED_BREP_SHAPE_REPRESENTATION('',(#1874),#62966);
#1654=ADVANCED_BREP_SHAPE_REPRESENTATION('',(#1875),#62967);
#1655=ADVANCED_BREP_SHAPE_REPRESENTATION('',(#1876),#62968);
#1656=ADVANCED_BREP_SHAPE_REPRESENTATION('',(#33),#62969);
#1657=ADVANCED_BREP_SHAPE_REPRESENTATION('',(#1877),#62970);
#1658=ADVANCED_BREP_SHAPE_REPRESENTATION('',(#34),#62971);
#1659=ADVANCED_BREP_SHAPE_REPRESENTATION('',(#35),#62972);
#1660=ADVANCED_BREP_SHAPE_REPRESENTATION('',(#1878),#62974);
#1661=ADVANCED_BREP_SHAPE_REPRESENTATION('',(#1879),#62975);
#1662=ADVANCED_BREP_SHAPE_REPRESENTATION('',(#1880),#62976);
#1663=ADVANCED_BREP_SHAPE_REPRESENTATION('',(#1881),#62977);
#1664=ADVANCED_BREP_SHAPE_REPRESENTATION('',(#1882),#62978);
#1665=ADVANCED_BREP_SHAPE_REPRESENTATION('',(#1883),#62979);
#1666=ADVANCED_BREP_SHAPE_REPRESENTATION('',(#1884),#62980);
#1667=ADVANCED_BREP_SHAPE_REPRESENTATION('',(#1885),#62981);
#1668=ADVANCED_BREP_SHAPE_REPRESENTATION('',(#1886),#62982);
#1669=ADVANCED_BREP_SHAPE_REPRESENTATION('',(#36),#62983);
#1670=STYLED_ITEM('',(#63891),#1783);
#1671=STYLED_ITEM('',(#63898),#1784);
#1672=STYLED_ITEM('',(#63898),#1785);
#1673=STYLED_ITEM('',(#63898),#1786);
#1674=STYLED_ITEM('',(#63912),#1787);
#1675=STYLED_ITEM('',(#63926),#1788);
#1676=STYLED_ITEM('',(#63912),#1789);
#1677=STYLED_ITEM('',(#63926),#1790);
#1678=STYLED_ITEM('',(#63905),#1791);
#1679=STYLED_ITEM('',(#63905),#1792);
#1680=STYLED_ITEM('',(#63905),#1793);
#1681=STYLED_ITEM('',(#63912),#1794);
#1682=STYLED_ITEM('',(#63912),#1795);
#1683=STYLED_ITEM('',(#63912),#1796);
#1684=STYLED_ITEM('',(#63912),#1797);
#1685=STYLED_ITEM('',(#63912),#1798);
#1686=STYLED_ITEM('',(#63912),#1799);
#1687=STYLED_ITEM('',(#63912),#1800);
#1688=STYLED_ITEM('',(#63912),#1801);
#1689=STYLED_ITEM('',(#63912),#1802);
#1690=STYLED_ITEM('',(#63912),#1803);
#1691=STYLED_ITEM('',(#63912),#1804);
#1692=STYLED_ITEM('',(#63912),#1805);
#1693=STYLED_ITEM('',(#63912),#1806);
#1694=STYLED_ITEM('',(#63912),#1807);
#1695=STYLED_ITEM('',(#63912),#1808);
#1696=STYLED_ITEM('',(#63912),#1809);
#1697=STYLED_ITEM('',(#63912),#1810);
#1698=STYLED_ITEM('',(#63912),#1811);
#1699=STYLED_ITEM('',(#63912),#1812);
#1700=STYLED_ITEM('',(#63912),#1813);
#1701=STYLED_ITEM('',(#63912),#1814);
#1702=STYLED_ITEM('',(#63912),#1815);
#1703=STYLED_ITEM('',(#63912),#1816);
#1704=STYLED_ITEM('',(#63912),#1817);
#1705=STYLED_ITEM('',(#63912),#1818);
#1706=STYLED_ITEM('',(#63898),#1819);
#1707=STYLED_ITEM('',(#63898),#1820);
#1708=STYLED_ITEM('',(#63919),#1821);
#1709=STYLED_ITEM('',(#63891),#1822);
#1710=STYLED_ITEM('',(#63905),#1823);
#1711=STYLED_ITEM('',(#63926),#1824);
#1712=STYLED_ITEM('',(#63919),#1825);
#1713=STYLED_ITEM('',(#63919),#28);
#1714=STYLED_ITEM('',(#63919),#1826);
#1715=STYLED_ITEM('',(#63919),#29);
#1716=STYLED_ITEM('',(#63919),#30);
#1717=STYLED_ITEM('',(#63919),#1827);
#1718=STYLED_ITEM('',(#63912),#1828);
#1719=STYLED_ITEM('',(#63912),#1829);
#1720=STYLED_ITEM('',(#63905),#1830);
#1721=STYLED_ITEM('',(#63905),#1831);
#1722=STYLED_ITEM('',(#63905),#1832);
#1723=STYLED_ITEM('',(#63912),#1833);
#1724=STYLED_ITEM('',(#63919),#1834);
#1725=STYLED_ITEM('',(#63919),#1835);
#1726=STYLED_ITEM('',(#63919),#31);
#1727=STYLED_ITEM('',(#63891),#1836);
#1728=STYLED_ITEM('',(#63905),#1837);
#1729=STYLED_ITEM('',(#63912),#1838);
#1730=STYLED_ITEM('',(#63898),#1839);
#1731=STYLED_ITEM('',(#63912),#1840);
#1732=STYLED_ITEM('',(#63926),#1841);
#1733=STYLED_ITEM('',(#63905),#1842);
#1734=STYLED_ITEM('',(#63905),#1843);
#1735=STYLED_ITEM('',(#63905),#1844);
#1736=STYLED_ITEM('',(#63912),#1845);
#1737=STYLED_ITEM('',(#63912),#1846);
#1738=STYLED_ITEM('',(#63912),#1847);
#1739=STYLED_ITEM('',(#63912),#1848);
#1740=STYLED_ITEM('',(#63912),#1849);
#1741=STYLED_ITEM('',(#63912),#1850);
#1742=STYLED_ITEM('',(#63912),#1851);
#1743=STYLED_ITEM('',(#63912),#1852);
#1744=STYLED_ITEM('',(#63912),#1853);
#1745=STYLED_ITEM('',(#63912),#1854);
#1746=STYLED_ITEM('',(#63912),#1855);
#1747=STYLED_ITEM('',(#63912),#1856);
#1748=STYLED_ITEM('',(#63912),#1857);
#1749=STYLED_ITEM('',(#63912),#1858);
#1750=STYLED_ITEM('',(#63905),#1859);
#1751=STYLED_ITEM('',(#63905),#1860);
#1752=STYLED_ITEM('',(#63905),#1861);
#1753=STYLED_ITEM('',(#63905),#1862);
#1754=STYLED_ITEM('',(#63905),#1863);
#1755=STYLED_ITEM('',(#63905),#1864);
#1756=STYLED_ITEM('',(#63905),#1865);
#1757=STYLED_ITEM('',(#63905),#1866);
#1758=STYLED_ITEM('',(#63926),#1867);
#1759=STYLED_ITEM('',(#63919),#1868);
#1760=STYLED_ITEM('',(#63919),#1869);
#1761=STYLED_ITEM('',(#63919),#32);
#1762=STYLED_ITEM('',(#63898),#1870);
#1763=STYLED_ITEM('',(#63905),#1871);
#1764=STYLED_ITEM('',(#63919),#1872);
#1765=STYLED_ITEM('',(#63891),#1873);
#1766=STYLED_ITEM('',(#63905),#1874);
#1767=STYLED_ITEM('',(#63926),#1875);
#1768=STYLED_ITEM('',(#63919),#1876);
#1769=STYLED_ITEM('',(#63919),#33);
#1770=STYLED_ITEM('',(#63919),#1877);
#1771=STYLED_ITEM('',(#63919),#34);
#1772=STYLED_ITEM('',(#63919),#35);
#1773=STYLED_ITEM('',(#63919),#1878);
#1774=STYLED_ITEM('',(#63912),#1879);
#1775=STYLED_ITEM('',(#63912),#1880);
#1776=STYLED_ITEM('',(#63905),#1881);
#1777=STYLED_ITEM('',(#63905),#1882);
#1778=STYLED_ITEM('',(#63905),#1883);
#1779=STYLED_ITEM('',(#63912),#1884);
#1780=STYLED_ITEM('',(#63919),#1885);
#1781=STYLED_ITEM('',(#63919),#1886);
#1782=STYLED_ITEM('',(#63919),#36);
#1783=MANIFOLD_SOLID_BREP('Body1',#22964);
#1784=MANIFOLD_SOLID_BREP('Body1',#22965);
#1785=MANIFOLD_SOLID_BREP('Body1',#22966);
#1786=MANIFOLD_SOLID_BREP('Body1',#22967);
#1787=MANIFOLD_SOLID_BREP('Body1',#22968);
#1788=MANIFOLD_SOLID_BREP('Body1',#22969);
#1789=MANIFOLD_SOLID_BREP('Body1',#22970);
#1790=MANIFOLD_SOLID_BREP('Body1',#22971);
#1791=MANIFOLD_SOLID_BREP('Body1',#22972);
#1792=MANIFOLD_SOLID_BREP('Body1',#22973);
#1793=MANIFOLD_SOLID_BREP('Body1',#22974);
#1794=MANIFOLD_SOLID_BREP('Body1',#22975);
#1795=MANIFOLD_SOLID_BREP('Body1',#22976);
#1796=MANIFOLD_SOLID_BREP('Body1',#22977);
#1797=MANIFOLD_SOLID_BREP('Body2',#22978);
#1798=MANIFOLD_SOLID_BREP('Body3',#22979);
#1799=MANIFOLD_SOLID_BREP('Body4',#22980);
#1800=MANIFOLD_SOLID_BREP('Body5',#22981);
#1801=MANIFOLD_SOLID_BREP('Body6',#22982);
#1802=MANIFOLD_SOLID_BREP('Body7',#22983);
#1803=MANIFOLD_SOLID_BREP('Continuous crown cage',#22984);
#1804=MANIFOLD_SOLID_BREP('Body1',#22985);
#1805=MANIFOLD_SOLID_BREP('Body2',#22986);
#1806=MANIFOLD_SOLID_BREP('Body1',#22987);
#1807=MANIFOLD_SOLID_BREP('Body1',#22988);
#1808=MANIFOLD_SOLID_BREP('Body1',#22989);
#1809=MANIFOLD_SOLID_BREP('Body2',#22990);
#1810=MANIFOLD_SOLID_BREP('Body3',#22991);
#1811=MANIFOLD_SOLID_BREP('Body4',#22992);
#1812=MANIFOLD_SOLID_BREP('Body5',#22993);
#1813=MANIFOLD_SOLID_BREP('Body6',#22994);
#1814=MANIFOLD_SOLID_BREP('Body7',#22995);
#1815=MANIFOLD_SOLID_BREP('Body8',#22996);
#1816=MANIFOLD_SOLID_BREP('Continuous crown cage',#22997);
#1817=MANIFOLD_SOLID_BREP('Body1',#22998);
#1818=MANIFOLD_SOLID_BREP('Body2',#22999);
#1819=MANIFOLD_SOLID_BREP('Body1',#23000);
#1820=MANIFOLD_SOLID_BREP('Body1',#23001);
#1821=MANIFOLD_SOLID_BREP('Body1',#23002);
#1822=MANIFOLD_SOLID_BREP('Body1',#23003);
#1823=MANIFOLD_SOLID_BREP('Body1',#23004);
#1824=MANIFOLD_SOLID_BREP('Body1',#23005);
#1825=MANIFOLD_SOLID_BREP('Body1',#23006);
#1826=MANIFOLD_SOLID_BREP('Body1',#23009);
#1827=MANIFOLD_SOLID_BREP('Body1',#23014);
#1828=MANIFOLD_SOLID_BREP('Body1',#23015);
#1829=MANIFOLD_SOLID_BREP('Body1',#23016);
#1830=MANIFOLD_SOLID_BREP('Body1',#23017);
#1831=MANIFOLD_SOLID_BREP('Body1',#23018);
#1832=MANIFOLD_SOLID_BREP('Body1',#23019);
#1833=MANIFOLD_SOLID_BREP('Body1',#23020);
#1834=MANIFOLD_SOLID_BREP('Body1',#23021);
#1835=MANIFOLD_SOLID_BREP('Body1',#23022);
#1836=MANIFOLD_SOLID_BREP('Body1',#23025);
#1837=MANIFOLD_SOLID_BREP('Body1',#23026);
#1838=MANIFOLD_SOLID_BREP('Body1',#23027);
#1839=MANIFOLD_SOLID_BREP('Body1',#23028);
#1840=MANIFOLD_SOLID_BREP('Body1',#23029);
#1841=MANIFOLD_SOLID_BREP('Body1',#23030);
#1842=MANIFOLD_SOLID_BREP('Body1',#23031);
#1843=MANIFOLD_SOLID_BREP('Body1',#23032);
#1844=MANIFOLD_SOLID_BREP('Body1',#23033);
#1845=MANIFOLD_SOLID_BREP('Body1',#23034);
#1846=MANIFOLD_SOLID_BREP('Body1',#23035);
#1847=MANIFOLD_SOLID_BREP('Body1',#23036);
#1848=MANIFOLD_SOLID_BREP('Body2',#23037);
#1849=MANIFOLD_SOLID_BREP('Body3',#23038);
#1850=MANIFOLD_SOLID_BREP('Body4',#23039);
#1851=MANIFOLD_SOLID_BREP('Body5',#23040);
#1852=MANIFOLD_SOLID_BREP('Body6',#23041);
#1853=MANIFOLD_SOLID_BREP('Body7',#23042);
#1854=MANIFOLD_SOLID_BREP('Continuous crown cage',#23043);
#1855=MANIFOLD_SOLID_BREP('Body1',#23044);
#1856=MANIFOLD_SOLID_BREP('Body2',#23045);
#1857=MANIFOLD_SOLID_BREP('Body1',#23046);
#1858=MANIFOLD_SOLID_BREP('Body1',#23047);
#1859=MANIFOLD_SOLID_BREP('Body1',#23048);
#1860=MANIFOLD_SOLID_BREP('Body2',#23049);
#1861=MANIFOLD_SOLID_BREP('Body3',#23050);
#1862=MANIFOLD_SOLID_BREP('Body4',#23051);
#1863=MANIFOLD_SOLID_BREP('Body5',#23052);
#1864=MANIFOLD_SOLID_BREP('Body6',#23053);
#1865=MANIFOLD_SOLID_BREP('Body7',#23054);
#1866=MANIFOLD_SOLID_BREP('Body8',#23055);
#1867=MANIFOLD_SOLID_BREP('Continuous crown cage',#23056);
#1868=MANIFOLD_SOLID_BREP('Body1',#23057);
#1869=MANIFOLD_SOLID_BREP('Body2',#23058);
#1870=MANIFOLD_SOLID_BREP('Body1',#23061);
#1871=MANIFOLD_SOLID_BREP('Body1',#23062);
#1872=MANIFOLD_SOLID_BREP('Body1',#23063);
#1873=MANIFOLD_SOLID_BREP('Body1',#23064);
#1874=MANIFOLD_SOLID_BREP('Body1',#23065);
#1875=MANIFOLD_SOLID_BREP('Body1',#23066);
#1876=MANIFOLD_SOLID_BREP('Body1',#23067);
#1877=MANIFOLD_SOLID_BREP('Body1',#23070);
#1878=MANIFOLD_SOLID_BREP('Body1',#23075);
#1879=MANIFOLD_SOLID_BREP('Body1',#23076);
#1880=MANIFOLD_SOLID_BREP('Body1',#23077);
#1881=MANIFOLD_SOLID_BREP('Body1',#23078);
#1882=MANIFOLD_SOLID_BREP('Body1',#23079);
#1883=MANIFOLD_SOLID_BREP('Body1',#23080);
#1884=MANIFOLD_SOLID_BREP('Body1',#23081);
#1885=MANIFOLD_SOLID_BREP('Body1',#23082);
#1886=MANIFOLD_SOLID_BREP('Body1',#23083);
#1887=FACE_BOUND('',#4198,.T.);
#1888=FACE_BOUND('',#4199,.T.);
#1889=FACE_BOUND('',#4200,.T.);
#1890=FACE_BOUND('',#4201,.T.);
#1891=FACE_BOUND('',#4202,.T.);
#1892=FACE_BOUND('',#4203,.T.);
#1893=FACE_BOUND('',#4204,.T.);
#1894=FACE_BOUND('',#4205,.T.);
#1895=FACE_BOUND('',#4206,.T.);
#1896=FACE_BOUND('',#4207,.T.);
#1897=FACE_BOUND('',#4209,.T.);
#1898=FACE_BOUND('',#4210,.T.);
#1899=FACE_BOUND('',#4211,.T.);
#1900=FACE_BOUND('',#4212,.T.);
#1901=FACE_BOUND('',#4213,.T.);
#1902=FACE_BOUND('',#4214,.T.);
#1903=FACE_BOUND('',#4215,.T.);
#1904=FACE_BOUND('',#4216,.T.);
#1905=FACE_BOUND('',#4217,.T.);
#1906=FACE_BOUND('',#4218,.T.);
#1907=FACE_BOUND('',#4239,.T.);
#1908=FACE_BOUND('',#4242,.T.);
#1909=FACE_BOUND('',#4245,.T.);
#1910=FACE_BOUND('',#4248,.T.);
#1911=FACE_BOUND('',#4250,.T.);
#1912=FACE_BOUND('',#4251,.T.);
#1913=FACE_BOUND('',#4252,.T.);
#1914=FACE_BOUND('',#4253,.T.);
#1915=FACE_BOUND('',#4254,.T.);
#1916=FACE_BOUND('',#4255,.T.);
#1917=FACE_BOUND('',#4265,.T.);
#1918=FACE_BOUND('',#4266,.T.);
#1919=FACE_BOUND('',#4267,.T.);
#1920=FACE_BOUND('',#4268,.T.);
#1921=FACE_BOUND('',#4269,.T.);
#1922=FACE_BOUND('',#4270,.T.);
#1923=FACE_BOUND('',#4271,.T.);
#1924=FACE_BOUND('',#4272,.T.);
#1925=FACE_BOUND('',#4278,.T.);
#1926=FACE_BOUND('',#4286,.T.);
#1927=FACE_BOUND('',#4287,.T.);
#1928=FACE_BOUND('',#4288,.T.);
#1929=FACE_BOUND('',#4289,.T.);
#1930=FACE_BOUND('',#4292,.T.);
#1931=FACE_BOUND('',#4293,.T.);
#1932=FACE_BOUND('',#4294,.T.);
#1933=FACE_BOUND('',#4295,.T.);
#1934=FACE_BOUND('',#4298,.T.);
#1935=FACE_BOUND('',#4299,.T.);
#1936=FACE_BOUND('',#4305,.T.);
#1937=FACE_BOUND('',#4309,.T.);
#1938=FACE_BOUND('',#4310,.T.);
#1939=FACE_BOUND('',#4311,.T.);
#1940=FACE_BOUND('',#4312,.T.);
#1941=FACE_BOUND('',#4314,.T.);
#1942=FACE_BOUND('',#4315,.T.);
#1943=FACE_BOUND('',#4316,.T.);
#1944=FACE_BOUND('',#4317,.T.);
#1945=FACE_BOUND('',#4323,.T.);
#1946=FACE_BOUND('',#4331,.T.);
#1947=FACE_BOUND('',#4332,.T.);
#1948=FACE_BOUND('',#4333,.T.);
#1949=FACE_BOUND('',#4334,.T.);
#1950=FACE_BOUND('',#4337,.T.);
#1951=FACE_BOUND('',#4338,.T.);
#1952=FACE_BOUND('',#4339,.T.);
#1953=FACE_BOUND('',#4340,.T.);
#1954=FACE_BOUND('',#4343,.T.);
#1955=FACE_BOUND('',#4344,.T.);
#1956=FACE_BOUND('',#4350,.T.);
#1957=FACE_BOUND('',#4351,.T.);
#1958=FACE_BOUND('',#4352,.T.);
#1959=FACE_BOUND('',#4353,.T.);
#1960=FACE_BOUND('',#4357,.T.);
#1961=FACE_BOUND('',#4360,.T.);
#1962=FACE_BOUND('',#4361,.T.);
#1963=FACE_BOUND('',#4362,.T.);
#1964=FACE_BOUND('',#4363,.T.);
#1965=FACE_BOUND('',#4366,.T.);
#1966=FACE_BOUND('',#4373,.T.);
#1967=FACE_BOUND('',#4375,.T.);
#1968=FACE_BOUND('',#4378,.T.);
#1969=FACE_BOUND('',#4385,.T.);
#1970=FACE_BOUND('',#4387,.T.);
#1971=FACE_BOUND('',#4390,.T.);
#1972=FACE_BOUND('',#4393,.T.);
#1973=FACE_BOUND('',#4396,.T.);
#1974=FACE_BOUND('',#4399,.T.);
#1975=FACE_BOUND('',#4409,.T.);
#1976=FACE_BOUND('',#4410,.T.);
#1977=FACE_BOUND('',#4411,.T.);
#1978=FACE_BOUND('',#4412,.T.);
#1979=FACE_BOUND('',#4419,.T.);
#1980=FACE_BOUND('',#4420,.T.);
#1981=FACE_BOUND('',#4421,.T.);
#1982=FACE_BOUND('',#4422,.T.);
#1983=FACE_BOUND('',#4431,.T.);
#1984=FACE_BOUND('',#4434,.T.);
#1985=FACE_BOUND('',#4439,.T.);
#1986=FACE_BOUND('',#4444,.T.);
#1987=FACE_BOUND('',#4469,.T.);
#1988=FACE_BOUND('',#4472,.T.);
#1989=FACE_BOUND('',#4475,.T.);
#1990=FACE_BOUND('',#4478,.T.);
#1991=FACE_BOUND('',#4481,.T.);
#1992=FACE_BOUND('',#4488,.T.);
#1993=FACE_BOUND('',#4491,.T.);
#1994=FACE_BOUND('',#4496,.T.);
#1995=FACE_BOUND('',#4501,.T.);
#1996=FACE_BOUND('',#4529,.T.);
#1997=FACE_BOUND('',#4532,.T.);
#1998=FACE_BOUND('',#4535,.T.);
#1999=FACE_BOUND('',#4538,.T.);
#2000=FACE_BOUND('',#4541,.T.);
#2001=FACE_BOUND('',#4552,.T.);
#2002=FACE_BOUND('',#4553,.T.);
#2003=FACE_BOUND('',#4554,.T.);
#2004=FACE_BOUND('',#4555,.T.);
#2005=FACE_BOUND('',#4557,.T.);
#2006=FACE_BOUND('',#4558,.T.);
#2007=FACE_BOUND('',#4559,.T.);
#2008=FACE_BOUND('',#4560,.T.);
#2009=FACE_BOUND('',#4578,.T.);
#2010=FACE_BOUND('',#4579,.T.);
#2011=FACE_BOUND('',#4580,.T.);
#2012=FACE_BOUND('',#4581,.T.);
#2013=FACE_BOUND('',#4582,.T.);
#2014=FACE_BOUND('',#4583,.T.);
#2015=FACE_BOUND('',#4584,.T.);
#2016=FACE_BOUND('',#4585,.T.);
#2017=FACE_BOUND('',#4586,.T.);
#2018=FACE_BOUND('',#4587,.T.);
#2019=FACE_BOUND('',#4588,.T.);
#2020=FACE_BOUND('',#4589,.T.);
#2021=FACE_BOUND('',#4591,.T.);
#2022=FACE_BOUND('',#4592,.T.);
#2023=FACE_BOUND('',#4593,.T.);
#2024=FACE_BOUND('',#4594,.T.);
#2025=FACE_BOUND('',#4595,.T.);
#2026=FACE_BOUND('',#4596,.T.);
#2027=FACE_BOUND('',#4597,.T.);
#2028=FACE_BOUND('',#4598,.T.);
#2029=FACE_BOUND('',#4599,.T.);
#2030=FACE_BOUND('',#4600,.T.);
#2031=FACE_BOUND('',#4601,.T.);
#2032=FACE_BOUND('',#4602,.T.);
#2033=FACE_BOUND('',#4620,.T.);
#2034=FACE_BOUND('',#4621,.T.);
#2035=FACE_BOUND('',#4622,.T.);
#2036=FACE_BOUND('',#4623,.T.);
#2037=FACE_BOUND('',#4626,.T.);
#2038=FACE_BOUND('',#4628,.T.);
#2039=FACE_BOUND('',#4629,.T.);
#2040=FACE_BOUND('',#4630,.T.);
#2041=FACE_BOUND('',#4631,.T.);
#2042=FACE_BOUND('',#4647,.T.);
#2043=FACE_BOUND('',#4648,.T.);
#2044=FACE_BOUND('',#4649,.T.);
#2045=FACE_BOUND('',#4650,.T.);
#2046=FACE_BOUND('',#4682,.T.);
#2047=FACE_BOUND('',#4685,.T.);
#2048=FACE_BOUND('',#4695,.T.);
#2049=FACE_BOUND('',#4703,.T.);
#2050=FACE_BOUND('',#4728,.T.);
#2051=FACE_BOUND('',#4729,.T.);
#2052=FACE_BOUND('',#4730,.T.);
#2053=FACE_BOUND('',#4731,.T.);
#2054=FACE_BOUND('',#4737,.T.);
#2055=FACE_BOUND('',#4738,.T.);
#2056=FACE_BOUND('',#4739,.T.);
#2057=FACE_BOUND('',#4740,.T.);
#2058=FACE_BOUND('',#4745,.T.);
#2059=FACE_BOUND('',#4751,.T.);
#2060=FACE_BOUND('',#4769,.T.);
#2061=FACE_BOUND('',#4909,.T.);
#2062=FACE_BOUND('',#4921,.T.);
#2063=FACE_BOUND('',#4924,.T.);
#2064=FACE_BOUND('',#4927,.T.);
#2065=FACE_BOUND('',#4932,.T.);
#2066=FACE_BOUND('',#4934,.T.);
#2067=FACE_BOUND('',#4939,.T.);
#2068=FACE_BOUND('',#4941,.T.);
#2069=FACE_BOUND('',#4943,.T.);
#2070=FACE_BOUND('',#4945,.T.);
#2071=FACE_BOUND('',#4954,.T.);
#2072=FACE_BOUND('',#4955,.T.);
#2073=FACE_BOUND('',#4957,.T.);
#2074=FACE_BOUND('',#4958,.T.);
#2075=FACE_BOUND('',#4961,.T.);
#2076=FACE_BOUND('',#4963,.T.);
#2077=FACE_BOUND('',#4968,.T.);
#2078=FACE_BOUND('',#4970,.T.);
#2079=FACE_BOUND('',#4974,.T.);
#2080=FACE_BOUND('',#4976,.T.);
#2081=FACE_BOUND('',#4995,.T.);
#2082=FACE_BOUND('',#5003,.T.);
#2083=FACE_BOUND('',#5005,.T.);
#2084=FACE_BOUND('',#5011,.T.);
#2085=FACE_BOUND('',#5042,.T.);
#2086=FACE_BOUND('',#5045,.T.);
#2087=FACE_BOUND('',#5048,.T.);
#2088=FACE_BOUND('',#5051,.T.);
#2089=FACE_BOUND('',#5071,.T.);
#2090=FACE_BOUND('',#5072,.T.);
#2091=FACE_BOUND('',#5073,.T.);
#2092=FACE_BOUND('',#5074,.T.);
#2093=FACE_BOUND('',#5075,.T.);
#2094=FACE_BOUND('',#5076,.T.);
#2095=FACE_BOUND('',#5077,.T.);
#2096=FACE_BOUND('',#5078,.T.);
#2097=FACE_BOUND('',#5079,.T.);
#2098=FACE_BOUND('',#5080,.T.);
#2099=FACE_BOUND('',#5081,.T.);
#2100=FACE_BOUND('',#5082,.T.);
#2101=FACE_BOUND('',#5083,.T.);
#2102=FACE_BOUND('',#5084,.T.);
#2103=FACE_BOUND('',#5086,.T.);
#2104=FACE_BOUND('',#5087,.T.);
#2105=FACE_BOUND('',#5088,.T.);
#2106=FACE_BOUND('',#5089,.T.);
#2107=FACE_BOUND('',#5090,.T.);
#2108=FACE_BOUND('',#5091,.T.);
#2109=FACE_BOUND('',#5092,.T.);
#2110=FACE_BOUND('',#5093,.T.);
#2111=FACE_BOUND('',#5094,.T.);
#2112=FACE_BOUND('',#5095,.T.);
#2113=FACE_BOUND('',#5096,.T.);
#2114=FACE_BOUND('',#5097,.T.);
#2115=FACE_BOUND('',#5098,.T.);
#2116=FACE_BOUND('',#5099,.T.);
#2117=FACE_BOUND('',#5100,.T.);
#2118=FACE_BOUND('',#5101,.T.);
#2119=FACE_BOUND('',#5102,.T.);
#2120=FACE_BOUND('',#5103,.T.);
#2121=FACE_BOUND('',#5104,.T.);
#2122=FACE_BOUND('',#5105,.T.);
#2123=FACE_BOUND('',#5106,.T.);
#2124=FACE_BOUND('',#5107,.T.);
#2125=FACE_BOUND('',#5116,.T.);
#2126=FACE_BOUND('',#5119,.T.);
#2127=FACE_BOUND('',#5122,.T.);
#2128=FACE_BOUND('',#5125,.T.);
#2129=FACE_BOUND('',#5127,.T.);
#2130=FACE_BOUND('',#5128,.T.);
#2131=FACE_BOUND('',#5129,.T.);
#2132=FACE_BOUND('',#5130,.T.);
#2133=FACE_BOUND('',#5131,.T.);
#2134=FACE_BOUND('',#5132,.T.);
#2135=FACE_BOUND('',#5142,.T.);
#2136=FACE_BOUND('',#5143,.T.);
#2137=FACE_BOUND('',#5144,.T.);
#2138=FACE_BOUND('',#5145,.T.);
#2139=FACE_BOUND('',#5146,.T.);
#2140=FACE_BOUND('',#5147,.T.);
#2141=FACE_BOUND('',#5148,.T.);
#2142=FACE_BOUND('',#5149,.T.);
#2143=FACE_BOUND('',#5155,.T.);
#2144=FACE_BOUND('',#5163,.T.);
#2145=FACE_BOUND('',#5164,.T.);
#2146=FACE_BOUND('',#5165,.T.);
#2147=FACE_BOUND('',#5166,.T.);
#2148=FACE_BOUND('',#5169,.T.);
#2149=FACE_BOUND('',#5170,.T.);
#2150=FACE_BOUND('',#5171,.T.);
#2151=FACE_BOUND('',#5172,.T.);
#2152=FACE_BOUND('',#5175,.T.);
#2153=FACE_BOUND('',#5176,.T.);
#2154=FACE_BOUND('',#5182,.T.);
#2155=FACE_BOUND('',#5186,.T.);
#2156=FACE_BOUND('',#5187,.T.);
#2157=FACE_BOUND('',#5188,.T.);
#2158=FACE_BOUND('',#5189,.T.);
#2159=FACE_BOUND('',#5191,.T.);
#2160=FACE_BOUND('',#5192,.T.);
#2161=FACE_BOUND('',#5193,.T.);
#2162=FACE_BOUND('',#5194,.T.);
#2163=FACE_BOUND('',#5200,.T.);
#2164=FACE_BOUND('',#5208,.T.);
#2165=FACE_BOUND('',#5209,.T.);
#2166=FACE_BOUND('',#5210,.T.);
#2167=FACE_BOUND('',#5211,.T.);
#2168=FACE_BOUND('',#5214,.T.);
#2169=FACE_BOUND('',#5215,.T.);
#2170=FACE_BOUND('',#5216,.T.);
#2171=FACE_BOUND('',#5217,.T.);
#2172=FACE_BOUND('',#5220,.T.);
#2173=FACE_BOUND('',#5221,.T.);
#2174=FACE_BOUND('',#5227,.T.);
#2175=FACE_BOUND('',#5228,.T.);
#2176=FACE_BOUND('',#5229,.T.);
#2177=FACE_BOUND('',#5230,.T.);
#2178=FACE_BOUND('',#5234,.T.);
#2179=FACE_BOUND('',#5237,.T.);
#2180=FACE_BOUND('',#5238,.T.);
#2181=FACE_BOUND('',#5239,.T.);
#2182=FACE_BOUND('',#5240,.T.);
#2183=FACE_BOUND('',#5243,.T.);
#2184=FACE_BOUND('',#5250,.T.);
#2185=FACE_BOUND('',#5252,.T.);
#2186=FACE_BOUND('',#5255,.T.);
#2187=FACE_BOUND('',#5262,.T.);
#2188=FACE_BOUND('',#5264,.T.);
#2189=FACE_BOUND('',#5267,.T.);
#2190=FACE_BOUND('',#5270,.T.);
#2191=FACE_BOUND('',#5273,.T.);
#2192=FACE_BOUND('',#5276,.T.);
#2193=FACE_BOUND('',#5286,.T.);
#2194=FACE_BOUND('',#5287,.T.);
#2195=FACE_BOUND('',#5288,.T.);
#2196=FACE_BOUND('',#5289,.T.);
#2197=FACE_BOUND('',#5296,.T.);
#2198=FACE_BOUND('',#5297,.T.);
#2199=FACE_BOUND('',#5298,.T.);
#2200=FACE_BOUND('',#5299,.T.);
#2201=FACE_BOUND('',#5308,.T.);
#2202=FACE_BOUND('',#5311,.T.);
#2203=FACE_BOUND('',#5316,.T.);
#2204=FACE_BOUND('',#5321,.T.);
#2205=FACE_BOUND('',#5346,.T.);
#2206=FACE_BOUND('',#5349,.T.);
#2207=FACE_BOUND('',#5352,.T.);
#2208=FACE_BOUND('',#5355,.T.);
#2209=FACE_BOUND('',#5358,.T.);
#2210=FACE_BOUND('',#5365,.T.);
#2211=FACE_BOUND('',#5368,.T.);
#2212=FACE_BOUND('',#5373,.T.);
#2213=FACE_BOUND('',#5378,.T.);
#2214=FACE_BOUND('',#5406,.T.);
#2215=FACE_BOUND('',#5409,.T.);
#2216=FACE_BOUND('',#5412,.T.);
#2217=FACE_BOUND('',#5415,.T.);
#2218=FACE_BOUND('',#5418,.T.);
#2219=FACE_BOUND('',#5434,.T.);
#2220=FACE_BOUND('',#5446,.T.);
#2221=FACE_BOUND('',#5447,.T.);
#2222=FACE_BOUND('',#5448,.T.);
#2223=FACE_BOUND('',#5449,.T.);
#2224=FACE_BOUND('',#5451,.T.);
#2225=FACE_BOUND('',#5452,.T.);
#2226=FACE_BOUND('',#5453,.T.);
#2227=FACE_BOUND('',#5454,.T.);
#2228=FACE_BOUND('',#5468,.T.);
#2229=FACE_BOUND('',#5469,.T.);
#2230=FACE_BOUND('',#5470,.T.);
#2231=FACE_BOUND('',#5471,.T.);
#2232=FACE_BOUND('',#5472,.T.);
#2233=FACE_BOUND('',#5473,.T.);
#2234=FACE_BOUND('',#5474,.T.);
#2235=FACE_BOUND('',#5475,.T.);
#2236=FACE_BOUND('',#5477,.T.);
#2237=FACE_BOUND('',#5478,.T.);
#2238=FACE_BOUND('',#5479,.T.);
#2239=FACE_BOUND('',#5480,.T.);
#2240=FACE_BOUND('',#5481,.T.);
#2241=FACE_BOUND('',#5482,.T.);
#2242=FACE_BOUND('',#5483,.T.);
#2243=FACE_BOUND('',#5484,.T.);
#2244=FACE_BOUND('',#5502,.T.);
#2245=FACE_BOUND('',#5503,.T.);
#2246=FACE_BOUND('',#5504,.T.);
#2247=FACE_BOUND('',#5505,.T.);
#2248=FACE_BOUND('',#5508,.T.);
#2249=FACE_BOUND('',#5510,.T.);
#2250=FACE_BOUND('',#5511,.T.);
#2251=FACE_BOUND('',#5512,.T.);
#2252=FACE_BOUND('',#5513,.T.);
#2253=FACE_BOUND('',#5529,.T.);
#2254=FACE_BOUND('',#5530,.T.);
#2255=FACE_BOUND('',#5531,.T.);
#2256=FACE_BOUND('',#5532,.T.);
#2257=FACE_BOUND('',#5564,.T.);
#2258=FACE_BOUND('',#5567,.T.);
#2259=FACE_BOUND('',#5577,.T.);
#2260=FACE_BOUND('',#5585,.T.);
#2261=FACE_BOUND('',#5610,.T.);
#2262=FACE_BOUND('',#5611,.T.);
#2263=FACE_BOUND('',#5612,.T.);
#2264=FACE_BOUND('',#5613,.T.);
#2265=FACE_BOUND('',#5619,.T.);
#2266=FACE_BOUND('',#5620,.T.);
#2267=FACE_BOUND('',#5621,.T.);
#2268=FACE_BOUND('',#5622,.T.);
#2269=FACE_BOUND('',#5627,.T.);
#2270=FACE_BOUND('',#5633,.T.);
#2271=FACE_BOUND('',#5651,.T.);
#2272=FACE_BOUND('',#5791,.T.);
#2273=FACE_BOUND('',#5803,.T.);
#2274=FACE_BOUND('',#5806,.T.);
#2275=FACE_BOUND('',#5809,.T.);
#2276=FACE_BOUND('',#5814,.T.);
#2277=FACE_BOUND('',#5816,.T.);
#2278=FACE_BOUND('',#5821,.T.);
#2279=FACE_BOUND('',#5823,.T.);
#2280=FACE_BOUND('',#5825,.T.);
#2281=FACE_BOUND('',#5827,.T.);
#2282=FACE_BOUND('',#5836,.T.);
#2283=FACE_BOUND('',#5837,.T.);
#2284=FACE_BOUND('',#5839,.T.);
#2285=FACE_BOUND('',#5840,.T.);
#2286=FACE_BOUND('',#5843,.T.);
#2287=FACE_BOUND('',#5845,.T.);
#2288=FACE_BOUND('',#5850,.T.);
#2289=FACE_BOUND('',#5852,.T.);
#2290=FACE_BOUND('',#5856,.T.);
#2291=FACE_BOUND('',#5858,.T.);
#2292=FACE_BOUND('',#5877,.T.);
#2293=FACE_BOUND('',#5885,.T.);
#2294=FACE_BOUND('',#5887,.T.);
#2295=FACE_BOUND('',#5893,.T.);
#2296=PLANE('',#24034);
#2297=PLANE('',#24035);
#2298=PLANE('',#24036);
#2299=PLANE('',#24037);
#2300=PLANE('',#24038);
#2301=PLANE('',#24039);
#2302=PLANE('',#24041);
#2303=PLANE('',#24042);
#2304=PLANE('',#24043);
#2305=PLANE('',#24044);
#2306=PLANE('',#24045);
#2307=PLANE('',#24046);
#2308=PLANE('',#24048);
#2309=PLANE('',#24049);
#2310=PLANE('',#24050);
#2311=PLANE('',#24051);
#2312=PLANE('',#24052);
#2313=PLANE('',#24053);
#2314=PLANE('',#24076);
#2315=PLANE('',#24081);
#2316=PLANE('',#24086);
#2317=PLANE('',#24091);
#2318=PLANE('',#24093);
#2319=PLANE('',#24102);
#2320=PLANE('',#24103);
#2321=PLANE('',#24104);
#2322=PLANE('',#24105);
#2323=PLANE('',#24106);
#2324=PLANE('',#24120);
#2325=PLANE('',#24127);
#2326=PLANE('',#24131);
#2327=PLANE('',#24132);
#2328=PLANE('',#24133);
#2329=PLANE('',#24134);
#2330=PLANE('',#24135);
#2331=PLANE('',#24136);
#2332=PLANE('',#24137);
#2333=PLANE('',#24151);
#2334=PLANE('',#24158);
#2335=PLANE('',#24159);
#2336=PLANE('',#24173);
#2337=PLANE('',#24180);
#2338=PLANE('',#24184);
#2339=PLANE('',#24185);
#2340=PLANE('',#24186);
#2341=PLANE('',#24187);
#2342=PLANE('',#24188);
#2343=PLANE('',#24189);
#2344=PLANE('',#24190);
#2345=PLANE('',#24201);
#2346=PLANE('',#24202);
#2347=PLANE('',#24209);
#2348=PLANE('',#24213);
#2349=PLANE('',#24218);
#2350=PLANE('',#24222);
#2351=PLANE('',#24223);
#2352=PLANE('',#24224);
#2353=PLANE('',#24225);
#2354=PLANE('',#24226);
#2355=PLANE('',#24227);
#2356=PLANE('',#24232);
#2357=PLANE('',#24236);
#2358=PLANE('',#24237);
#2359=PLANE('',#24238);
#2360=PLANE('',#24239);
#2361=PLANE('',#24240);
#2362=PLANE('',#24241);
#2363=PLANE('',#24246);
#2364=PLANE('',#24251);
#2365=PLANE('',#24256);
#2366=PLANE('',#24261);
#2367=PLANE('',#24271);
#2368=PLANE('',#24272);
#2369=PLANE('',#24273);
#2370=PLANE('',#24274);
#2371=PLANE('',#24275);
#2372=PLANE('',#24276);
#2373=PLANE('',#24277);
#2374=PLANE('',#24278);
#2375=PLANE('',#24279);
#2376=PLANE('',#24280);
#2377=PLANE('',#24281);
#2378=PLANE('',#24282);
#2379=PLANE('',#24283);
#2380=PLANE('',#24284);
#2381=PLANE('',#24300);
#2382=PLANE('',#24303);
#2383=PLANE('',#24315);
#2384=PLANE('',#24324);
#2385=PLANE('',#24355);
#2386=PLANE('',#24360);
#2387=PLANE('',#24365);
#2388=PLANE('',#24371);
#2389=PLANE('',#24376);
#2390=PLANE('',#24385);
#2391=PLANE('',#24389);
#2392=PLANE('',#24390);
#2393=PLANE('',#24392);
#2394=PLANE('',#24397);
#2395=PLANE('',#24400);
#2396=PLANE('',#24405);
#2397=PLANE('',#24428);
#2398=PLANE('',#24431);
#2399=PLANE('',#24443);
#2400=PLANE('',#24452);
#2401=PLANE('',#24485);
#2402=PLANE('',#24490);
#2403=PLANE('',#24495);
#2404=PLANE('',#24500);
#2405=PLANE('',#24505);
#2406=PLANE('',#24510);
#2407=PLANE('',#24519);
#2408=PLANE('',#24523);
#2409=PLANE('',#24524);
#2410=PLANE('',#24526);
#2411=PLANE('',#24531);
#2412=PLANE('',#24534);
#2413=PLANE('',#24539);
#2414=PLANE('',#24561);
#2415=PLANE('',#24562);
#2416=PLANE('',#24563);
#2417=PLANE('',#24564);
#2418=PLANE('',#24565);
#2419=PLANE('',#24566);
#2420=PLANE('',#24604);
#2421=PLANE('',#24605);
#2422=PLANE('',#24606);
#2423=PLANE('',#24607);
#2424=PLANE('',#24608);
#2425=PLANE('',#24609);
#2426=PLANE('',#24614);
#2427=PLANE('',#24618);
#2428=PLANE('',#24622);
#2429=PLANE('',#24626);
#2430=PLANE('',#24630);
#2431=PLANE('',#24634);
#2432=PLANE('',#24638);
#2433=PLANE('',#24642);
#2434=PLANE('',#24643);
#2435=PLANE('',#24644);
#2436=PLANE('',#24645);
#2437=PLANE('',#24646);
#2438=PLANE('',#24647);
#2439=PLANE('',#24650);
#2440=PLANE('',#24656);
#2441=PLANE('',#24662);
#2442=PLANE('',#24668);
#2443=PLANE('',#24674);
#2444=PLANE('',#24675);
#2445=PLANE('',#24676);
#2446=PLANE('',#24677);
#2447=PLANE('',#24678);
#2448=PLANE('',#24679);
#2449=PLANE('',#24680);
#2450=PLANE('',#24681);
#2451=PLANE('',#24682);
#2452=PLANE('',#24683);
#2453=PLANE('',#24684);
#2454=PLANE('',#24685);
#2455=PLANE('',#24686);
#2456=PLANE('',#24687);
#2457=PLANE('',#24689);
#2458=PLANE('',#24690);
#2459=PLANE('',#24691);
#2460=PLANE('',#24692);
#2461=PLANE('',#24693);
#2462=PLANE('',#24694);
#2463=PLANE('',#24695);
#2464=PLANE('',#24696);
#2465=PLANE('',#24697);
#2466=PLANE('',#24698);
#2467=PLANE('',#24700);
#2468=PLANE('',#24701);
#2469=PLANE('',#24702);
#2470=PLANE('',#24703);
#2471=PLANE('',#24704);
#2472=PLANE('',#24705);
#2473=PLANE('',#24706);
#2474=PLANE('',#24707);
#2475=PLANE('',#24708);
#2476=PLANE('',#24709);
#2477=PLANE('',#24719);
#2478=PLANE('',#24723);
#2479=PLANE('',#24725);
#2480=PLANE('',#24726);
#2481=PLANE('',#24727);
#2482=PLANE('',#24728);
#2483=PLANE('',#24729);
#2484=PLANE('',#24730);
#2485=PLANE('',#24731);
#2486=PLANE('',#24732);
#2487=PLANE('',#24733);
#2488=PLANE('',#24738);
#2489=PLANE('',#24739);
#2490=PLANE('',#24747);
#2491=PLANE('',#24776);
#2492=PLANE('',#24788);
#2493=PLANE('',#24789);
#2494=PLANE('',#24796);
#2495=PLANE('',#24798);
#2496=PLANE('',#24806);
#2497=PLANE('',#24814);
#2498=PLANE('',#24815);
#2499=PLANE('',#24816);
#2500=PLANE('',#24817);
#2501=PLANE('',#24818);
#2502=PLANE('',#24819);
#2503=PLANE('',#24820);
#2504=PLANE('',#24821);
#2505=PLANE('',#24822);
#2506=PLANE('',#24824);
#2507=PLANE('',#24832);
#2508=PLANE('',#24840);
#2509=PLANE('',#24841);
#2510=PLANE('',#24842);
#2511=PLANE('',#24843);
#2512=PLANE('',#24844);
#2513=PLANE('',#24845);
#2514=PLANE('',#24846);
#2515=PLANE('',#24847);
#2516=PLANE('',#24848);
#2517=PLANE('',#25000);
#2518=PLANE('',#25005);
#2519=PLANE('',#25007);
#2520=PLANE('',#25008);
#2521=PLANE('',#25010);
#2522=PLANE('',#25011);
#2523=PLANE('',#25012);
#2524=PLANE('',#25017);
#2525=PLANE('',#25018);
#2526=PLANE('',#25023);
#2527=PLANE('',#25032);
#2528=PLANE('',#25033);
#2529=PLANE('',#25035);
#2530=PLANE('',#25039);
#2531=PLANE('',#25046);
#2532=PLANE('',#25047);
#2533=PLANE('',#25052);
#2534=PLANE('',#25056);
#2535=PLANE('',#25057);
#2536=PLANE('',#25058);
#2537=PLANE('',#25059);
#2538=PLANE('',#25060);
#2539=PLANE('',#25063);
#2540=PLANE('',#25071);
#2541=PLANE('',#25079);
#2542=PLANE('',#25080);
#2543=PLANE('',#25088);
#2544=PLANE('',#25089);
#2545=PLANE('',#25091);
#2546=PLANE('',#25092);
#2547=PLANE('',#25093);
#2548=PLANE('',#25094);
#2549=PLANE('',#25095);
#2550=PLANE('',#25096);
#2551=PLANE('',#25097);
#2552=PLANE('',#25098);
#2553=PLANE('',#25099);
#2554=PLANE('',#25100);
#2555=PLANE('',#25102);
#2556=PLANE('',#25103);
#2557=PLANE('',#25104);
#2558=PLANE('',#25105);
#2559=PLANE('',#25106);
#2560=PLANE('',#25107);
#2561=PLANE('',#25108);
#2562=PLANE('',#25109);
#2563=PLANE('',#25117);
#2564=PLANE('',#25125);
#2565=PLANE('',#25126);
#2566=PLANE('',#25128);
#2567=PLANE('',#25136);
#2568=PLANE('',#25144);
#2569=PLANE('',#25145);
#2570=PLANE('',#25146);
#2571=PLANE('',#25147);
#2572=PLANE('',#25148);
#2573=PLANE('',#25149);
#2574=PLANE('',#25150);
#2575=PLANE('',#25151);
#2576=PLANE('',#25152);
#2577=PLANE('',#25206);
#2578=PLANE('',#25210);
#2579=PLANE('',#25214);
#2580=PLANE('',#25218);
#2581=PLANE('',#25222);
#2582=PLANE('',#25226);
#2583=PLANE('',#25230);
#2584=PLANE('',#25234);
#2585=PLANE('',#25238);
#2586=PLANE('',#25243);
#2587=PLANE('',#25248);
#2588=PLANE('',#25253);
#2589=PLANE('',#25293);
#2590=PLANE('',#25294);
#2591=PLANE('',#25295);
#2592=PLANE('',#25296);
#2593=PLANE('',#25297);
#2594=PLANE('',#25298);
#2595=PLANE('',#25321);
#2596=PLANE('',#25326);
#2597=PLANE('',#25331);
#2598=PLANE('',#25336);
#2599=PLANE('',#25338);
#2600=PLANE('',#25347);
#2601=PLANE('',#25348);
#2602=PLANE('',#25349);
#2603=PLANE('',#25350);
#2604=PLANE('',#25351);
#2605=PLANE('',#25365);
#2606=PLANE('',#25372);
#2607=PLANE('',#25376);
#2608=PLANE('',#25377);
#2609=PLANE('',#25378);
#2610=PLANE('',#25379);
#2611=PLANE('',#25380);
#2612=PLANE('',#25381);
#2613=PLANE('',#25382);
#2614=PLANE('',#25396);
#2615=PLANE('',#25403);
#2616=PLANE('',#25404);
#2617=PLANE('',#25418);
#2618=PLANE('',#25425);
#2619=PLANE('',#25429);
#2620=PLANE('',#25430);
#2621=PLANE('',#25431);
#2622=PLANE('',#25432);
#2623=PLANE('',#25433);
#2624=PLANE('',#25434);
#2625=PLANE('',#25435);
#2626=PLANE('',#25446);
#2627=PLANE('',#25447);
#2628=PLANE('',#25454);
#2629=PLANE('',#25458);
#2630=PLANE('',#25463);
#2631=PLANE('',#25467);
#2632=PLANE('',#25468);
#2633=PLANE('',#25469);
#2634=PLANE('',#25470);
#2635=PLANE('',#25471);
#2636=PLANE('',#25472);
#2637=PLANE('',#25477);
#2638=PLANE('',#25481);
#2639=PLANE('',#25482);
#2640=PLANE('',#25483);
#2641=PLANE('',#25484);
#2642=PLANE('',#25485);
#2643=PLANE('',#25486);
#2644=PLANE('',#25491);
#2645=PLANE('',#25496);
#2646=PLANE('',#25501);
#2647=PLANE('',#25506);
#2648=PLANE('',#25516);
#2649=PLANE('',#25517);
#2650=PLANE('',#25518);
#2651=PLANE('',#25519);
#2652=PLANE('',#25520);
#2653=PLANE('',#25521);
#2654=PLANE('',#25522);
#2655=PLANE('',#25523);
#2656=PLANE('',#25524);
#2657=PLANE('',#25525);
#2658=PLANE('',#25526);
#2659=PLANE('',#25527);
#2660=PLANE('',#25528);
#2661=PLANE('',#25529);
#2662=PLANE('',#25545);
#2663=PLANE('',#25548);
#2664=PLANE('',#25560);
#2665=PLANE('',#25569);
#2666=PLANE('',#25600);
#2667=PLANE('',#25605);
#2668=PLANE('',#25610);
#2669=PLANE('',#25616);
#2670=PLANE('',#25621);
#2671=PLANE('',#25630);
#2672=PLANE('',#25634);
#2673=PLANE('',#25635);
#2674=PLANE('',#25637);
#2675=PLANE('',#25642);
#2676=PLANE('',#25645);
#2677=PLANE('',#25650);
#2678=PLANE('',#25673);
#2679=PLANE('',#25676);
#2680=PLANE('',#25688);
#2681=PLANE('',#25697);
#2682=PLANE('',#25730);
#2683=PLANE('',#25735);
#2684=PLANE('',#25740);
#2685=PLANE('',#25745);
#2686=PLANE('',#25750);
#2687=PLANE('',#25755);
#2688=PLANE('',#25764);
#2689=PLANE('',#25768);
#2690=PLANE('',#25769);
#2691=PLANE('',#25771);
#2692=PLANE('',#25776);
#2693=PLANE('',#25779);
#2694=PLANE('',#25784);
#2695=PLANE('',#25793);
#2696=PLANE('',#25794);
#2697=PLANE('',#25795);
#2698=PLANE('',#25796);
#2699=PLANE('',#25797);
#2700=PLANE('',#25798);
#2701=PLANE('',#25799);
#2702=PLANE('',#25800);
#2703=PLANE('',#25801);
#2704=PLANE('',#25803);
#2705=PLANE('',#25811);
#2706=PLANE('',#25830);
#2707=PLANE('',#25831);
#2708=PLANE('',#25832);
#2709=PLANE('',#25833);
#2710=PLANE('',#25834);
#2711=PLANE('',#25835);
#2712=PLANE('',#25861);
#2713=PLANE('',#25862);
#2714=PLANE('',#25863);
#2715=PLANE('',#25864);
#2716=PLANE('',#25865);
#2717=PLANE('',#25866);
#2718=PLANE('',#25871);
#2719=PLANE('',#25875);
#2720=PLANE('',#25879);
#2721=PLANE('',#25883);
#2722=PLANE('',#25887);
#2723=PLANE('',#25891);
#2724=PLANE('',#25895);
#2725=PLANE('',#25899);
#2726=PLANE('',#25900);
#2727=PLANE('',#25901);
#2728=PLANE('',#25902);
#2729=PLANE('',#25903);
#2730=PLANE('',#25904);
#2731=PLANE('',#25907);
#2732=PLANE('',#25913);
#2733=PLANE('',#25919);
#2734=PLANE('',#25925);
#2735=PLANE('',#25931);
#2736=PLANE('',#25932);
#2737=PLANE('',#25933);
#2738=PLANE('',#25934);
#2739=PLANE('',#25935);
#2740=PLANE('',#25936);
#2741=PLANE('',#25937);
#2742=PLANE('',#25938);
#2743=PLANE('',#25939);
#2744=PLANE('',#25940);
#2745=PLANE('',#25941);
#2746=PLANE('',#25942);
#2747=PLANE('',#25943);
#2748=PLANE('',#25944);
#2749=PLANE('',#25946);
#2750=PLANE('',#25947);
#2751=PLANE('',#25948);
#2752=PLANE('',#25949);
#2753=PLANE('',#25950);
#2754=PLANE('',#25951);
#2755=PLANE('',#25952);
#2756=PLANE('',#25953);
#2757=PLANE('',#25954);
#2758=PLANE('',#25955);
#2759=PLANE('',#25957);
#2760=PLANE('',#25958);
#2761=PLANE('',#25959);
#2762=PLANE('',#25960);
#2763=PLANE('',#25961);
#2764=PLANE('',#25962);
#2765=PLANE('',#25963);
#2766=PLANE('',#25964);
#2767=PLANE('',#25965);
#2768=PLANE('',#25966);
#2769=PLANE('',#25976);
#2770=PLANE('',#25980);
#2771=PLANE('',#25982);
#2772=PLANE('',#25983);
#2773=PLANE('',#25984);
#2774=PLANE('',#25985);
#2775=PLANE('',#25986);
#2776=PLANE('',#25987);
#2777=PLANE('',#25988);
#2778=PLANE('',#25989);
#2779=PLANE('',#25990);
#2780=PLANE('',#25995);
#2781=PLANE('',#25996);
#2782=PLANE('',#26004);
#2783=PLANE('',#26033);
#2784=PLANE('',#26045);
#2785=PLANE('',#26046);
#2786=PLANE('',#26053);
#2787=PLANE('',#26055);
#2788=PLANE('',#26063);
#2789=PLANE('',#26071);
#2790=PLANE('',#26072);
#2791=PLANE('',#26073);
#2792=PLANE('',#26074);
#2793=PLANE('',#26075);
#2794=PLANE('',#26076);
#2795=PLANE('',#26077);
#2796=PLANE('',#26078);
#2797=PLANE('',#26079);
#2798=PLANE('',#26081);
#2799=PLANE('',#26089);
#2800=PLANE('',#26097);
#2801=PLANE('',#26098);
#2802=PLANE('',#26099);
#2803=PLANE('',#26100);
#2804=PLANE('',#26101);
#2805=PLANE('',#26102);
#2806=PLANE('',#26103);
#2807=PLANE('',#26104);
#2808=PLANE('',#26105);
#2809=PLANE('',#26257);
#2810=PLANE('',#26262);
#2811=PLANE('',#26264);
#2812=PLANE('',#26265);
#2813=PLANE('',#26267);
#2814=PLANE('',#26268);
#2815=PLANE('',#26269);
#2816=PLANE('',#26274);
#2817=PLANE('',#26275);
#2818=PLANE('',#26280);
#2819=PLANE('',#26289);
#2820=PLANE('',#26290);
#2821=PLANE('',#26292);
#2822=PLANE('',#26296);
#2823=PLANE('',#26303);
#2824=PLANE('',#26304);
#2825=PLANE('',#26309);
#2826=PLANE('',#26313);
#2827=PLANE('',#26314);
#2828=PLANE('',#26315);
#2829=PLANE('',#26316);
#2830=PLANE('',#26317);
#2831=PLANE('',#26320);
#2832=PLANE('',#26328);
#2833=PLANE('',#26336);
#2834=PLANE('',#26337);
#2835=PLANE('',#26345);
#2836=PLANE('',#26346);
#2837=PLANE('',#26348);
#2838=PLANE('',#26349);
#2839=PLANE('',#26350);
#2840=PLANE('',#26351);
#2841=PLANE('',#26352);
#2842=PLANE('',#26353);
#2843=PLANE('',#26354);
#2844=PLANE('',#26355);
#2845=PLANE('',#26356);
#2846=PLANE('',#26357);
#2847=PLANE('',#26359);
#2848=PLANE('',#26360);
#2849=PLANE('',#26361);
#2850=PLANE('',#26362);
#2851=PLANE('',#26363);
#2852=PLANE('',#26364);
#2853=PLANE('',#26365);
#2854=PLANE('',#26366);
#2855=PLANE('',#26374);
#2856=PLANE('',#26382);
#2857=PLANE('',#26383);
#2858=PLANE('',#26385);
#2859=PLANE('',#26393);
#2860=PLANE('',#26401);
#2861=PLANE('',#26402);
#2862=PLANE('',#26403);
#2863=PLANE('',#26404);
#2864=PLANE('',#26405);
#2865=PLANE('',#26406);
#2866=PLANE('',#26407);
#2867=PLANE('',#26408);
#2868=PLANE('',#26409);
#2869=FACE_OUTER_BOUND('',#4183,.T.);
#2870=FACE_OUTER_BOUND('',#4184,.T.);
#2871=FACE_OUTER_BOUND('',#4185,.T.);
#2872=FACE_OUTER_BOUND('',#4186,.T.);
#2873=FACE_OUTER_BOUND('',#4187,.T.);
#2874=FACE_OUTER_BOUND('',#4188,.T.);
#2875=FACE_OUTER_BOUND('',#4189,.T.);
#2876=FACE_OUTER_BOUND('',#4190,.T.);
#2877=FACE_OUTER_BOUND('',#4191,.T.);
#2878=FACE_OUTER_BOUND('',#4192,.T.);
#2879=FACE_OUTER_BOUND('',#4193,.T.);
#2880=FACE_OUTER_BOUND('',#4194,.T.);
#2881=FACE_OUTER_BOUND('',#4195,.T.);
#2882=FACE_OUTER_BOUND('',#4196,.T.);
#2883=FACE_OUTER_BOUND('',#4197,.T.);
#2884=FACE_OUTER_BOUND('',#4208,.T.);
#2885=FACE_OUTER_BOUND('',#4219,.T.);
#2886=FACE_OUTER_BOUND('',#4220,.T.);
#2887=FACE_OUTER_BOUND('',#4221,.T.);
#2888=FACE_OUTER_BOUND('',#4222,.T.);
#2889=FACE_OUTER_BOUND('',#4223,.T.);
#2890=FACE_OUTER_BOUND('',#4224,.T.);
#2891=FACE_OUTER_BOUND('',#4225,.T.);
#2892=FACE_OUTER_BOUND('',#4226,.T.);
#2893=FACE_OUTER_BOUND('',#4227,.T.);
#2894=FACE_OUTER_BOUND('',#4228,.T.);
#2895=FACE_OUTER_BOUND('',#4229,.T.);
#2896=FACE_OUTER_BOUND('',#4230,.T.);
#2897=FACE_OUTER_BOUND('',#4231,.T.);
#2898=FACE_OUTER_BOUND('',#4232,.T.);
#2899=FACE_OUTER_BOUND('',#4233,.T.);
#2900=FACE_OUTER_BOUND('',#4234,.T.);
#2901=FACE_OUTER_BOUND('',#4235,.T.);
#2902=FACE_OUTER_BOUND('',#4236,.T.);
#2903=FACE_OUTER_BOUND('',#4237,.T.);
#2904=FACE_OUTER_BOUND('',#4238,.T.);
#2905=FACE_OUTER_BOUND('',#4240,.T.);
#2906=FACE_OUTER_BOUND('',#4241,.T.);
#2907=FACE_OUTER_BOUND('',#4243,.T.);
#2908=FACE_OUTER_BOUND('',#4244,.T.);
#2909=FACE_OUTER_BOUND('',#4246,.T.);
#2910=FACE_OUTER_BOUND('',#4247,.T.);
#2911=FACE_OUTER_BOUND('',#4249,.T.);
#2912=FACE_OUTER_BOUND('',#4256,.T.);
#2913=FACE_OUTER_BOUND('',#4257,.T.);
#2914=FACE_OUTER_BOUND('',#4258,.T.);
#2915=FACE_OUTER_BOUND('',#4259,.T.);
#2916=FACE_OUTER_BOUND('',#4260,.T.);
#2917=FACE_OUTER_BOUND('',#4261,.T.);
#2918=FACE_OUTER_BOUND('',#4262,.T.);
#2919=FACE_OUTER_BOUND('',#4263,.T.);
#2920=FACE_OUTER_BOUND('',#4264,.T.);
#2921=FACE_OUTER_BOUND('',#4273,.T.);
#2922=FACE_OUTER_BOUND('',#4274,.T.);
#2923=FACE_OUTER_BOUND('',#4275,.T.);
#2924=FACE_OUTER_BOUND('',#4276,.T.);
#2925=FACE_OUTER_BOUND('',#4277,.T.);
#2926=FACE_OUTER_BOUND('',#4279,.T.);
#2927=FACE_OUTER_BOUND('',#4280,.T.);
#2928=FACE_OUTER_BOUND('',#4281,.T.);
#2929=FACE_OUTER_BOUND('',#4282,.T.);
#2930=FACE_OUTER_BOUND('',#4283,.T.);
#2931=FACE_OUTER_BOUND('',#4284,.T.);
#2932=FACE_OUTER_BOUND('',#4285,.T.);
#2933=FACE_OUTER_BOUND('',#4290,.T.);
#2934=FACE_OUTER_BOUND('',#4291,.T.);
#2935=FACE_OUTER_BOUND('',#4296,.T.);
#2936=FACE_OUTER_BOUND('',#4297,.T.);
#2937=FACE_OUTER_BOUND('',#4300,.T.);
#2938=FACE_OUTER_BOUND('',#4301,.T.);
#2939=FACE_OUTER_BOUND('',#4302,.T.);
#2940=FACE_OUTER_BOUND('',#4303,.T.);
#2941=FACE_OUTER_BOUND('',#4304,.T.);
#2942=FACE_OUTER_BOUND('',#4306,.T.);
#2943=FACE_OUTER_BOUND('',#4307,.T.);
#2944=FACE_OUTER_BOUND('',#4308,.T.);
#2945=FACE_OUTER_BOUND('',#4313,.T.);
#2946=FACE_OUTER_BOUND('',#4318,.T.);
#2947=FACE_OUTER_BOUND('',#4319,.T.);
#2948=FACE_OUTER_BOUND('',#4320,.T.);
#2949=FACE_OUTER_BOUND('',#4321,.T.);
#2950=FACE_OUTER_BOUND('',#4322,.T.);
#2951=FACE_OUTER_BOUND('',#4324,.T.);
#2952=FACE_OUTER_BOUND('',#4325,.T.);
#2953=FACE_OUTER_BOUND('',#4326,.T.);
#2954=FACE_OUTER_BOUND('',#4327,.T.);
#2955=FACE_OUTER_BOUND('',#4328,.T.);
#2956=FACE_OUTER_BOUND('',#4329,.T.);
#2957=FACE_OUTER_BOUND('',#4330,.T.);
#2958=FACE_OUTER_BOUND('',#4335,.T.);
#2959=FACE_OUTER_BOUND('',#4336,.T.);
#2960=FACE_OUTER_BOUND('',#4341,.T.);
#2961=FACE_OUTER_BOUND('',#4342,.T.);
#2962=FACE_OUTER_BOUND('',#4345,.T.);
#2963=FACE_OUTER_BOUND('',#4346,.T.);
#2964=FACE_OUTER_BOUND('',#4347,.T.);
#2965=FACE_OUTER_BOUND('',#4348,.T.);
#2966=FACE_OUTER_BOUND('',#4349,.T.);
#2967=FACE_OUTER_BOUND('',#4354,.T.);
#2968=FACE_OUTER_BOUND('',#4355,.T.);
#2969=FACE_OUTER_BOUND('',#4356,.T.);
#2970=FACE_OUTER_BOUND('',#4358,.T.);
#2971=FACE_OUTER_BOUND('',#4359,.T.);
#2972=FACE_OUTER_BOUND('',#4364,.T.);
#2973=FACE_OUTER_BOUND('',#4365,.T.);
#2974=FACE_OUTER_BOUND('',#4367,.T.);
#2975=FACE_OUTER_BOUND('',#4368,.T.);
#2976=FACE_OUTER_BOUND('',#4369,.T.);
#2977=FACE_OUTER_BOUND('',#4370,.T.);
#2978=FACE_OUTER_BOUND('',#4371,.T.);
#2979=FACE_OUTER_BOUND('',#4372,.T.);
#2980=FACE_OUTER_BOUND('',#4374,.T.);
#2981=FACE_OUTER_BOUND('',#4376,.T.);
#2982=FACE_OUTER_BOUND('',#4377,.T.);
#2983=FACE_OUTER_BOUND('',#4379,.T.);
#2984=FACE_OUTER_BOUND('',#4380,.T.);
#2985=FACE_OUTER_BOUND('',#4381,.T.);
#2986=FACE_OUTER_BOUND('',#4382,.T.);
#2987=FACE_OUTER_BOUND('',#4383,.T.);
#2988=FACE_OUTER_BOUND('',#4384,.T.);
#2989=FACE_OUTER_BOUND('',#4386,.T.);
#2990=FACE_OUTER_BOUND('',#4388,.T.);
#2991=FACE_OUTER_BOUND('',#4389,.T.);
#2992=FACE_OUTER_BOUND('',#4391,.T.);
#2993=FACE_OUTER_BOUND('',#4392,.T.);
#2994=FACE_OUTER_BOUND('',#4394,.T.);
#2995=FACE_OUTER_BOUND('',#4395,.T.);
#2996=FACE_OUTER_BOUND('',#4397,.T.);
#2997=FACE_OUTER_BOUND('',#4398,.T.);
#2998=FACE_OUTER_BOUND('',#4400,.T.);
#2999=FACE_OUTER_BOUND('',#4401,.T.);
#3000=FACE_OUTER_BOUND('',#4402,.T.);
#3001=FACE_OUTER_BOUND('',#4403,.T.);
#3002=FACE_OUTER_BOUND('',#4404,.T.);
#3003=FACE_OUTER_BOUND('',#4405,.T.);
#3004=FACE_OUTER_BOUND('',#4406,.T.);
#3005=FACE_OUTER_BOUND('',#4407,.T.);
#3006=FACE_OUTER_BOUND('',#4408,.T.);
#3007=FACE_OUTER_BOUND('',#4413,.T.);
#3008=FACE_OUTER_BOUND('',#4414,.T.);
#3009=FACE_OUTER_BOUND('',#4415,.T.);
#3010=FACE_OUTER_BOUND('',#4416,.T.);
#3011=FACE_OUTER_BOUND('',#4417,.T.);
#3012=FACE_OUTER_BOUND('',#4418,.T.);
#3013=FACE_OUTER_BOUND('',#4423,.T.);
#3014=FACE_OUTER_BOUND('',#4424,.T.);
#3015=FACE_OUTER_BOUND('',#4425,.T.);
#3016=FACE_OUTER_BOUND('',#4426,.T.);
#3017=FACE_OUTER_BOUND('',#4427,.T.);
#3018=FACE_OUTER_BOUND('',#4428,.T.);
#3019=FACE_OUTER_BOUND('',#4429,.T.);
#3020=FACE_OUTER_BOUND('',#4430,.T.);
#3021=FACE_OUTER_BOUND('',#4432,.T.);
#3022=FACE_OUTER_BOUND('',#4433,.T.);
#3023=FACE_OUTER_BOUND('',#4435,.T.);
#3024=FACE_OUTER_BOUND('',#4436,.T.);
#3025=FACE_OUTER_BOUND('',#4437,.T.);
#3026=FACE_OUTER_BOUND('',#4438,.T.);
#3027=FACE_OUTER_BOUND('',#4440,.T.);
#3028=FACE_OUTER_BOUND('',#4441,.T.);
#3029=FACE_OUTER_BOUND('',#4442,.T.);
#3030=FACE_OUTER_BOUND('',#4443,.T.);
#3031=FACE_OUTER_BOUND('',#4445,.T.);
#3032=FACE_OUTER_BOUND('',#4446,.T.);
#3033=FACE_OUTER_BOUND('',#4447,.T.);
#3034=FACE_OUTER_BOUND('',#4448,.T.);
#3035=FACE_OUTER_BOUND('',#4449,.T.);
#3036=FACE_OUTER_BOUND('',#4450,.T.);
#3037=FACE_OUTER_BOUND('',#4451,.T.);
#3038=FACE_OUTER_BOUND('',#4452,.T.);
#3039=FACE_OUTER_BOUND('',#4453,.T.);
#3040=FACE_OUTER_BOUND('',#4454,.T.);
#3041=FACE_OUTER_BOUND('',#4455,.T.);
#3042=FACE_OUTER_BOUND('',#4456,.T.);
#3043=FACE_OUTER_BOUND('',#4457,.T.);
#3044=FACE_OUTER_BOUND('',#4458,.T.);
#3045=FACE_OUTER_BOUND('',#4459,.T.);
#3046=FACE_OUTER_BOUND('',#4460,.T.);
#3047=FACE_OUTER_BOUND('',#4461,.T.);
#3048=FACE_OUTER_BOUND('',#4462,.T.);
#3049=FACE_OUTER_BOUND('',#4463,.T.);
#3050=FACE_OUTER_BOUND('',#4464,.T.);
#3051=FACE_OUTER_BOUND('',#4465,.T.);
#3052=FACE_OUTER_BOUND('',#4466,.T.);
#3053=FACE_OUTER_BOUND('',#4467,.T.);
#3054=FACE_OUTER_BOUND('',#4468,.T.);
#3055=FACE_OUTER_BOUND('',#4470,.T.);
#3056=FACE_OUTER_BOUND('',#4471,.T.);
#3057=FACE_OUTER_BOUND('',#4473,.T.);
#3058=FACE_OUTER_BOUND('',#4474,.T.);
#3059=FACE_OUTER_BOUND('',#4476,.T.);
#3060=FACE_OUTER_BOUND('',#4477,.T.);
#3061=FACE_OUTER_BOUND('',#4479,.T.);
#3062=FACE_OUTER_BOUND('',#4480,.T.);
#3063=FACE_OUTER_BOUND('',#4482,.T.);
#3064=FACE_OUTER_BOUND('',#4483,.T.);
#3065=FACE_OUTER_BOUND('',#4484,.T.);
#3066=FACE_OUTER_BOUND('',#4485,.T.);
#3067=FACE_OUTER_BOUND('',#4486,.T.);
#3068=FACE_OUTER_BOUND('',#4487,.T.);
#3069=FACE_OUTER_BOUND('',#4489,.T.);
#3070=FACE_OUTER_BOUND('',#4490,.T.);
#3071=FACE_OUTER_BOUND('',#4492,.T.);
#3072=FACE_OUTER_BOUND('',#4493,.T.);
#3073=FACE_OUTER_BOUND('',#4494,.T.);
#3074=FACE_OUTER_BOUND('',#4495,.T.);
#3075=FACE_OUTER_BOUND('',#4497,.T.);
#3076=FACE_OUTER_BOUND('',#4498,.T.);
#3077=FACE_OUTER_BOUND('',#4499,.T.);
#3078=FACE_OUTER_BOUND('',#4500,.T.);
#3079=FACE_OUTER_BOUND('',#4502,.T.);
#3080=FACE_OUTER_BOUND('',#4503,.T.);
#3081=FACE_OUTER_BOUND('',#4504,.T.);
#3082=FACE_OUTER_BOUND('',#4505,.T.);
#3083=FACE_OUTER_BOUND('',#4506,.T.);
#3084=FACE_OUTER_BOUND('',#4507,.T.);
#3085=FACE_OUTER_BOUND('',#4508,.T.);
#3086=FACE_OUTER_BOUND('',#4509,.T.);
#3087=FACE_OUTER_BOUND('',#4510,.T.);
#3088=FACE_OUTER_BOUND('',#4511,.T.);
#3089=FACE_OUTER_BOUND('',#4512,.T.);
#3090=FACE_OUTER_BOUND('',#4513,.T.);
#3091=FACE_OUTER_BOUND('',#4514,.T.);
#3092=FACE_OUTER_BOUND('',#4515,.T.);
#3093=FACE_OUTER_BOUND('',#4516,.T.);
#3094=FACE_OUTER_BOUND('',#4517,.T.);
#3095=FACE_OUTER_BOUND('',#4518,.T.);
#3096=FACE_OUTER_BOUND('',#4519,.T.);
#3097=FACE_OUTER_BOUND('',#4520,.T.);
#3098=FACE_OUTER_BOUND('',#4521,.T.);
#3099=FACE_OUTER_BOUND('',#4522,.T.);
#3100=FACE_OUTER_BOUND('',#4523,.T.);
#3101=FACE_OUTER_BOUND('',#4524,.T.);
#3102=FACE_OUTER_BOUND('',#4525,.T.);
#3103=FACE_OUTER_BOUND('',#4526,.T.);
#3104=FACE_OUTER_BOUND('',#4527,.T.);
#3105=FACE_OUTER_BOUND('',#4528,.T.);
#3106=FACE_OUTER_BOUND('',#4530,.T.);
#3107=FACE_OUTER_BOUND('',#4531,.T.);
#3108=FACE_OUTER_BOUND('',#4533,.T.);
#3109=FACE_OUTER_BOUND('',#4534,.T.);
#3110=FACE_OUTER_BOUND('',#4536,.T.);
#3111=FACE_OUTER_BOUND('',#4537,.T.);
#3112=FACE_OUTER_BOUND('',#4539,.T.);
#3113=FACE_OUTER_BOUND('',#4540,.T.);
#3114=FACE_OUTER_BOUND('',#4542,.T.);
#3115=FACE_OUTER_BOUND('',#4543,.T.);
#3116=FACE_OUTER_BOUND('',#4544,.T.);
#3117=FACE_OUTER_BOUND('',#4545,.T.);
#3118=FACE_OUTER_BOUND('',#4546,.T.);
#3119=FACE_OUTER_BOUND('',#4547,.T.);
#3120=FACE_OUTER_BOUND('',#4548,.T.);
#3121=FACE_OUTER_BOUND('',#4549,.T.);
#3122=FACE_OUTER_BOUND('',#4550,.T.);
#3123=FACE_OUTER_BOUND('',#4551,.T.);
#3124=FACE_OUTER_BOUND('',#4556,.T.);
#3125=FACE_OUTER_BOUND('',#4561,.T.);
#3126=FACE_OUTER_BOUND('',#4562,.T.);
#3127=FACE_OUTER_BOUND('',#4563,.T.);
#3128=FACE_OUTER_BOUND('',#4564,.T.);
#3129=FACE_OUTER_BOUND('',#4565,.T.);
#3130=FACE_OUTER_BOUND('',#4566,.T.);
#3131=FACE_OUTER_BOUND('',#4567,.T.);
#3132=FACE_OUTER_BOUND('',#4568,.T.);
#3133=FACE_OUTER_BOUND('',#4569,.T.);
#3134=FACE_OUTER_BOUND('',#4570,.T.);
#3135=FACE_OUTER_BOUND('',#4571,.T.);
#3136=FACE_OUTER_BOUND('',#4572,.T.);
#3137=FACE_OUTER_BOUND('',#4573,.T.);
#3138=FACE_OUTER_BOUND('',#4574,.T.);
#3139=FACE_OUTER_BOUND('',#4575,.T.);
#3140=FACE_OUTER_BOUND('',#4576,.T.);
#3141=FACE_OUTER_BOUND('',#4577,.T.);
#3142=FACE_OUTER_BOUND('',#4590,.T.);
#3143=FACE_OUTER_BOUND('',#4603,.T.);
#3144=FACE_OUTER_BOUND('',#4604,.T.);
#3145=FACE_OUTER_BOUND('',#4605,.T.);
#3146=FACE_OUTER_BOUND('',#4606,.T.);
#3147=FACE_OUTER_BOUND('',#4607,.T.);
#3148=FACE_OUTER_BOUND('',#4608,.T.);
#3149=FACE_OUTER_BOUND('',#4609,.T.);
#3150=FACE_OUTER_BOUND('',#4610,.T.);
#3151=FACE_OUTER_BOUND('',#4611,.T.);
#3152=FACE_OUTER_BOUND('',#4612,.T.);
#3153=FACE_OUTER_BOUND('',#4613,.T.);
#3154=FACE_OUTER_BOUND('',#4614,.T.);
#3155=FACE_OUTER_BOUND('',#4615,.T.);
#3156=FACE_OUTER_BOUND('',#4616,.T.);
#3157=FACE_OUTER_BOUND('',#4617,.T.);
#3158=FACE_OUTER_BOUND('',#4618,.T.);
#3159=FACE_OUTER_BOUND('',#4619,.T.);
#3160=FACE_OUTER_BOUND('',#4624,.T.);
#3161=FACE_OUTER_BOUND('',#4625,.T.);
#3162=FACE_OUTER_BOUND('',#4627,.T.);
#3163=FACE_OUTER_BOUND('',#4632,.T.);
#3164=FACE_OUTER_BOUND('',#4633,.T.);
#3165=FACE_OUTER_BOUND('',#4634,.T.);
#3166=FACE_OUTER_BOUND('',#4635,.T.);
#3167=FACE_OUTER_BOUND('',#4636,.T.);
#3168=FACE_OUTER_BOUND('',#4637,.T.);
#3169=FACE_OUTER_BOUND('',#4638,.T.);
#3170=FACE_OUTER_BOUND('',#4639,.T.);
#3171=FACE_OUTER_BOUND('',#4640,.T.);
#3172=FACE_OUTER_BOUND('',#4641,.T.);
#3173=FACE_OUTER_BOUND('',#4642,.T.);
#3174=FACE_OUTER_BOUND('',#4643,.T.);
#3175=FACE_OUTER_BOUND('',#4644,.T.);
#3176=FACE_OUTER_BOUND('',#4645,.T.);
#3177=FACE_OUTER_BOUND('',#4646,.T.);
#3178=FACE_OUTER_BOUND('',#4651,.T.);
#3179=FACE_OUTER_BOUND('',#4652,.T.);
#3180=FACE_OUTER_BOUND('',#4653,.T.);
#3181=FACE_OUTER_BOUND('',#4654,.T.);
#3182=FACE_OUTER_BOUND('',#4655,.T.);
#3183=FACE_OUTER_BOUND('',#4656,.T.);
#3184=FACE_OUTER_BOUND('',#4657,.T.);
#3185=FACE_OUTER_BOUND('',#4658,.T.);
#3186=FACE_OUTER_BOUND('',#4659,.T.);
#3187=FACE_OUTER_BOUND('',#4660,.T.);
#3188=FACE_OUTER_BOUND('',#4661,.T.);
#3189=FACE_OUTER_BOUND('',#4662,.T.);
#3190=FACE_OUTER_BOUND('',#4663,.T.);
#3191=FACE_OUTER_BOUND('',#4664,.T.);
#3192=FACE_OUTER_BOUND('',#4665,.T.);
#3193=FACE_OUTER_BOUND('',#4666,.T.);
#3194=FACE_OUTER_BOUND('',#4667,.T.);
#3195=FACE_OUTER_BOUND('',#4668,.T.);
#3196=FACE_OUTER_BOUND('',#4669,.T.);
#3197=FACE_OUTER_BOUND('',#4670,.T.);
#3198=FACE_OUTER_BOUND('',#4671,.T.);
#3199=FACE_OUTER_BOUND('',#4672,.T.);
#3200=FACE_OUTER_BOUND('',#4673,.T.);
#3201=FACE_OUTER_BOUND('',#4674,.T.);
#3202=FACE_OUTER_BOUND('',#4675,.T.);
#3203=FACE_OUTER_BOUND('',#4676,.T.);
#3204=FACE_OUTER_BOUND('',#4677,.T.);
#3205=FACE_OUTER_BOUND('',#4678,.T.);
#3206=FACE_OUTER_BOUND('',#4679,.T.);
#3207=FACE_OUTER_BOUND('',#4680,.T.);
#3208=FACE_OUTER_BOUND('',#4681,.T.);
#3209=FACE_OUTER_BOUND('',#4683,.T.);
#3210=FACE_OUTER_BOUND('',#4684,.T.);
#3211=FACE_OUTER_BOUND('',#4686,.T.);
#3212=FACE_OUTER_BOUND('',#4687,.T.);
#3213=FACE_OUTER_BOUND('',#4688,.T.);
#3214=FACE_OUTER_BOUND('',#4689,.T.);
#3215=FACE_OUTER_BOUND('',#4690,.T.);
#3216=FACE_OUTER_BOUND('',#4691,.T.);
#3217=FACE_OUTER_BOUND('',#4692,.T.);
#3218=FACE_OUTER_BOUND('',#4693,.T.);
#3219=FACE_OUTER_BOUND('',#4694,.T.);
#3220=FACE_OUTER_BOUND('',#4696,.T.);
#3221=FACE_OUTER_BOUND('',#4697,.T.);
#3222=FACE_OUTER_BOUND('',#4698,.T.);
#3223=FACE_OUTER_BOUND('',#4699,.T.);
#3224=FACE_OUTER_BOUND('',#4700,.T.);
#3225=FACE_OUTER_BOUND('',#4701,.T.);
#3226=FACE_OUTER_BOUND('',#4702,.T.);
#3227=FACE_OUTER_BOUND('',#4704,.T.);
#3228=FACE_OUTER_BOUND('',#4705,.T.);
#3229=FACE_OUTER_BOUND('',#4706,.T.);
#3230=FACE_OUTER_BOUND('',#4707,.T.);
#3231=FACE_OUTER_BOUND('',#4708,.T.);
#3232=FACE_OUTER_BOUND('',#4709,.T.);
#3233=FACE_OUTER_BOUND('',#4710,.T.);
#3234=FACE_OUTER_BOUND('',#4711,.T.);
#3235=FACE_OUTER_BOUND('',#4712,.T.);
#3236=FACE_OUTER_BOUND('',#4713,.T.);
#3237=FACE_OUTER_BOUND('',#4714,.T.);
#3238=FACE_OUTER_BOUND('',#4715,.T.);
#3239=FACE_OUTER_BOUND('',#4716,.T.);
#3240=FACE_OUTER_BOUND('',#4717,.T.);
#3241=FACE_OUTER_BOUND('',#4718,.T.);
#3242=FACE_OUTER_BOUND('',#4719,.T.);
#3243=FACE_OUTER_BOUND('',#4720,.T.);
#3244=FACE_OUTER_BOUND('',#4721,.T.);
#3245=FACE_OUTER_BOUND('',#4722,.T.);
#3246=FACE_OUTER_BOUND('',#4723,.T.);
#3247=FACE_OUTER_BOUND('',#4724,.T.);
#3248=FACE_OUTER_BOUND('',#4725,.T.);
#3249=FACE_OUTER_BOUND('',#4726,.T.);
#3250=FACE_OUTER_BOUND('',#4727,.T.);
#3251=FACE_OUTER_BOUND('',#4732,.T.);
#3252=FACE_OUTER_BOUND('',#4733,.T.);
#3253=FACE_OUTER_BOUND('',#4734,.T.);
#3254=FACE_OUTER_BOUND('',#4735,.T.);
#3255=FACE_OUTER_BOUND('',#4736,.T.);
#3256=FACE_OUTER_BOUND('',#4741,.T.);
#3257=FACE_OUTER_BOUND('',#4742,.T.);
#3258=FACE_OUTER_BOUND('',#4743,.T.);
#3259=FACE_OUTER_BOUND('',#4744,.T.);
#3260=FACE_OUTER_BOUND('',#4746,.T.);
#3261=FACE_OUTER_BOUND('',#4747,.T.);
#3262=FACE_OUTER_BOUND('',#4748,.T.);
#3263=FACE_OUTER_BOUND('',#4749,.T.);
#3264=FACE_OUTER_BOUND('',#4750,.T.);
#3265=FACE_OUTER_BOUND('',#4752,.T.);
#3266=FACE_OUTER_BOUND('',#4753,.T.);
#3267=FACE_OUTER_BOUND('',#4754,.T.);
#3268=FACE_OUTER_BOUND('',#4755,.T.);
#3269=FACE_OUTER_BOUND('',#4756,.T.);
#3270=FACE_OUTER_BOUND('',#4757,.T.);
#3271=FACE_OUTER_BOUND('',#4758,.T.);
#3272=FACE_OUTER_BOUND('',#4759,.T.);
#3273=FACE_OUTER_BOUND('',#4760,.T.);
#3274=FACE_OUTER_BOUND('',#4761,.T.);
#3275=FACE_OUTER_BOUND('',#4762,.T.);
#3276=FACE_OUTER_BOUND('',#4763,.T.);
#3277=FACE_OUTER_BOUND('',#4764,.T.);
#3278=FACE_OUTER_BOUND('',#4765,.T.);
#3279=FACE_OUTER_BOUND('',#4766,.T.);
#3280=FACE_OUTER_BOUND('',#4767,.T.);
#3281=FACE_OUTER_BOUND('',#4768,.T.);
#3282=FACE_OUTER_BOUND('',#4770,.T.);
#3283=FACE_OUTER_BOUND('',#4771,.T.);
#3284=FACE_OUTER_BOUND('',#4772,.T.);
#3285=FACE_OUTER_BOUND('',#4773,.T.);
#3286=FACE_OUTER_BOUND('',#4774,.T.);
#3287=FACE_OUTER_BOUND('',#4775,.T.);
#3288=FACE_OUTER_BOUND('',#4776,.T.);
#3289=FACE_OUTER_BOUND('',#4777,.T.);
#3290=FACE_OUTER_BOUND('',#4778,.T.);
#3291=FACE_OUTER_BOUND('',#4779,.T.);
#3292=FACE_OUTER_BOUND('',#4780,.T.);
#3293=FACE_OUTER_BOUND('',#4781,.T.);
#3294=FACE_OUTER_BOUND('',#4782,.T.);
#3295=FACE_OUTER_BOUND('',#4783,.T.);
#3296=FACE_OUTER_BOUND('',#4784,.T.);
#3297=FACE_OUTER_BOUND('',#4785,.T.);
#3298=FACE_OUTER_BOUND('',#4786,.T.);
#3299=FACE_OUTER_BOUND('',#4787,.T.);
#3300=FACE_OUTER_BOUND('',#4788,.T.);
#3301=FACE_OUTER_BOUND('',#4789,.T.);
#3302=FACE_OUTER_BOUND('',#4790,.T.);
#3303=FACE_OUTER_BOUND('',#4791,.T.);
#3304=FACE_OUTER_BOUND('',#4792,.T.);
#3305=FACE_OUTER_BOUND('',#4793,.T.);
#3306=FACE_OUTER_BOUND('',#4794,.T.);
#3307=FACE_OUTER_BOUND('',#4795,.T.);
#3308=FACE_OUTER_BOUND('',#4796,.T.);
#3309=FACE_OUTER_BOUND('',#4797,.T.);
#3310=FACE_OUTER_BOUND('',#4798,.T.);
#3311=FACE_OUTER_BOUND('',#4799,.T.);
#3312=FACE_OUTER_BOUND('',#4800,.T.);
#3313=FACE_OUTER_BOUND('',#4801,.T.);
#3314=FACE_OUTER_BOUND('',#4802,.T.);
#3315=FACE_OUTER_BOUND('',#4803,.T.);
#3316=FACE_OUTER_BOUND('',#4804,.T.);
#3317=FACE_OUTER_BOUND('',#4805,.T.);
#3318=FACE_OUTER_BOUND('',#4806,.T.);
#3319=FACE_OUTER_BOUND('',#4807,.T.);
#3320=FACE_OUTER_BOUND('',#4808,.T.);
#3321=FACE_OUTER_BOUND('',#4809,.T.);
#3322=FACE_OUTER_BOUND('',#4810,.T.);
#3323=FACE_OUTER_BOUND('',#4811,.T.);
#3324=FACE_OUTER_BOUND('',#4812,.T.);
#3325=FACE_OUTER_BOUND('',#4813,.T.);
#3326=FACE_OUTER_BOUND('',#4814,.T.);
#3327=FACE_OUTER_BOUND('',#4815,.T.);
#3328=FACE_OUTER_BOUND('',#4816,.T.);
#3329=FACE_OUTER_BOUND('',#4817,.T.);
#3330=FACE_OUTER_BOUND('',#4818,.T.);
#3331=FACE_OUTER_BOUND('',#4819,.T.);
#3332=FACE_OUTER_BOUND('',#4820,.T.);
#3333=FACE_OUTER_BOUND('',#4821,.T.);
#3334=FACE_OUTER_BOUND('',#4822,.T.);
#3335=FACE_OUTER_BOUND('',#4823,.T.);
#3336=FACE_OUTER_BOUND('',#4824,.T.);
#3337=FACE_OUTER_BOUND('',#4825,.T.);
#3338=FACE_OUTER_BOUND('',#4826,.T.);
#3339=FACE_OUTER_BOUND('',#4827,.T.);
#3340=FACE_OUTER_BOUND('',#4828,.T.);
#3341=FACE_OUTER_BOUND('',#4829,.T.);
#3342=FACE_OUTER_BOUND('',#4830,.T.);
#3343=FACE_OUTER_BOUND('',#4831,.T.);
#3344=FACE_OUTER_BOUND('',#4832,.T.);
#3345=FACE_OUTER_BOUND('',#4833,.T.);
#3346=FACE_OUTER_BOUND('',#4834,.T.);
#3347=FACE_OUTER_BOUND('',#4835,.T.);
#3348=FACE_OUTER_BOUND('',#4836,.T.);
#3349=FACE_OUTER_BOUND('',#4837,.T.);
#3350=FACE_OUTER_BOUND('',#4838,.T.);
#3351=FACE_OUTER_BOUND('',#4839,.T.);
#3352=FACE_OUTER_BOUND('',#4840,.T.);
#3353=FACE_OUTER_BOUND('',#4841,.T.);
#3354=FACE_OUTER_BOUND('',#4842,.T.);
#3355=FACE_OUTER_BOUND('',#4843,.T.);
#3356=FACE_OUTER_BOUND('',#4844,.T.);
#3357=FACE_OUTER_BOUND('',#4845,.T.);
#3358=FACE_OUTER_BOUND('',#4846,.T.);
#3359=FACE_OUTER_BOUND('',#4847,.T.);
#3360=FACE_OUTER_BOUND('',#4848,.T.);
#3361=FACE_OUTER_BOUND('',#4849,.T.);
#3362=FACE_OUTER_BOUND('',#4850,.T.);
#3363=FACE_OUTER_BOUND('',#4851,.T.);
#3364=FACE_OUTER_BOUND('',#4852,.T.);
#3365=FACE_OUTER_BOUND('',#4853,.T.);
#3366=FACE_OUTER_BOUND('',#4854,.T.);
#3367=FACE_OUTER_BOUND('',#4855,.T.);
#3368=FACE_OUTER_BOUND('',#4856,.T.);
#3369=FACE_OUTER_BOUND('',#4857,.T.);
#3370=FACE_OUTER_BOUND('',#4858,.T.);
#3371=FACE_OUTER_BOUND('',#4859,.T.);
#3372=FACE_OUTER_BOUND('',#4860,.T.);
#3373=FACE_OUTER_BOUND('',#4861,.T.);
#3374=FACE_OUTER_BOUND('',#4862,.T.);
#3375=FACE_OUTER_BOUND('',#4863,.T.);
#3376=FACE_OUTER_BOUND('',#4864,.T.);
#3377=FACE_OUTER_BOUND('',#4865,.T.);
#3378=FACE_OUTER_BOUND('',#4866,.T.);
#3379=FACE_OUTER_BOUND('',#4867,.T.);
#3380=FACE_OUTER_BOUND('',#4868,.T.);
#3381=FACE_OUTER_BOUND('',#4869,.T.);
#3382=FACE_OUTER_BOUND('',#4870,.T.);
#3383=FACE_OUTER_BOUND('',#4871,.T.);
#3384=FACE_OUTER_BOUND('',#4872,.T.);
#3385=FACE_OUTER_BOUND('',#4873,.T.);
#3386=FACE_OUTER_BOUND('',#4874,.T.);
#3387=FACE_OUTER_BOUND('',#4875,.T.);
#3388=FACE_OUTER_BOUND('',#4876,.T.);
#3389=FACE_OUTER_BOUND('',#4877,.T.);
#3390=FACE_OUTER_BOUND('',#4878,.T.);
#3391=FACE_OUTER_BOUND('',#4879,.T.);
#3392=FACE_OUTER_BOUND('',#4880,.T.);
#3393=FACE_OUTER_BOUND('',#4881,.T.);
#3394=FACE_OUTER_BOUND('',#4882,.T.);
#3395=FACE_OUTER_BOUND('',#4883,.T.);
#3396=FACE_OUTER_BOUND('',#4884,.T.);
#3397=FACE_OUTER_BOUND('',#4885,.T.);
#3398=FACE_OUTER_BOUND('',#4886,.T.);
#3399=FACE_OUTER_BOUND('',#4887,.T.);
#3400=FACE_OUTER_BOUND('',#4888,.T.);
#3401=FACE_OUTER_BOUND('',#4889,.T.);
#3402=FACE_OUTER_BOUND('',#4890,.T.);
#3403=FACE_OUTER_BOUND('',#4891,.T.);
#3404=FACE_OUTER_BOUND('',#4892,.T.);
#3405=FACE_OUTER_BOUND('',#4893,.T.);
#3406=FACE_OUTER_BOUND('',#4894,.T.);
#3407=FACE_OUTER_BOUND('',#4895,.T.);
#3408=FACE_OUTER_BOUND('',#4896,.T.);
#3409=FACE_OUTER_BOUND('',#4897,.T.);
#3410=FACE_OUTER_BOUND('',#4898,.T.);
#3411=FACE_OUTER_BOUND('',#4899,.T.);
#3412=FACE_OUTER_BOUND('',#4900,.T.);
#3413=FACE_OUTER_BOUND('',#4901,.T.);
#3414=FACE_OUTER_BOUND('',#4902,.T.);
#3415=FACE_OUTER_BOUND('',#4903,.T.);
#3416=FACE_OUTER_BOUND('',#4904,.T.);
#3417=FACE_OUTER_BOUND('',#4905,.T.);
#3418=FACE_OUTER_BOUND('',#4906,.T.);
#3419=FACE_OUTER_BOUND('',#4907,.T.);
#3420=FACE_OUTER_BOUND('',#4908,.T.);
#3421=FACE_OUTER_BOUND('',#4910,.T.);
#3422=FACE_OUTER_BOUND('',#4911,.T.);
#3423=FACE_OUTER_BOUND('',#4912,.T.);
#3424=FACE_OUTER_BOUND('',#4913,.T.);
#3425=FACE_OUTER_BOUND('',#4914,.T.);
#3426=FACE_OUTER_BOUND('',#4915,.T.);
#3427=FACE_OUTER_BOUND('',#4916,.T.);
#3428=FACE_OUTER_BOUND('',#4917,.T.);
#3429=FACE_OUTER_BOUND('',#4918,.T.);
#3430=FACE_OUTER_BOUND('',#4919,.T.);
#3431=FACE_OUTER_BOUND('',#4920,.T.);
#3432=FACE_OUTER_BOUND('',#4922,.T.);
#3433=FACE_OUTER_BOUND('',#4923,.T.);
#3434=FACE_OUTER_BOUND('',#4925,.T.);
#3435=FACE_OUTER_BOUND('',#4926,.T.);
#3436=FACE_OUTER_BOUND('',#4928,.T.);
#3437=FACE_OUTER_BOUND('',#4929,.T.);
#3438=FACE_OUTER_BOUND('',#4930,.T.);
#3439=FACE_OUTER_BOUND('',#4931,.T.);
#3440=FACE_OUTER_BOUND('',#4933,.T.);
#3441=FACE_OUTER_BOUND('',#4935,.T.);
#3442=FACE_OUTER_BOUND('',#4936,.T.);
#3443=FACE_OUTER_BOUND('',#4937,.T.);
#3444=FACE_OUTER_BOUND('',#4938,.T.);
#3445=FACE_OUTER_BOUND('',#4940,.T.);
#3446=FACE_OUTER_BOUND('',#4942,.T.);
#3447=FACE_OUTER_BOUND('',#4944,.T.);
#3448=FACE_OUTER_BOUND('',#4946,.T.);
#3449=FACE_OUTER_BOUND('',#4947,.T.);
#3450=FACE_OUTER_BOUND('',#4948,.T.);
#3451=FACE_OUTER_BOUND('',#4949,.T.);
#3452=FACE_OUTER_BOUND('',#4950,.T.);
#3453=FACE_OUTER_BOUND('',#4951,.T.);
#3454=FACE_OUTER_BOUND('',#4952,.T.);
#3455=FACE_OUTER_BOUND('',#4953,.T.);
#3456=FACE_OUTER_BOUND('',#4956,.T.);
#3457=FACE_OUTER_BOUND('',#4959,.T.);
#3458=FACE_OUTER_BOUND('',#4960,.T.);
#3459=FACE_OUTER_BOUND('',#4962,.T.);
#3460=FACE_OUTER_BOUND('',#4964,.T.);
#3461=FACE_OUTER_BOUND('',#4965,.T.);
#3462=FACE_OUTER_BOUND('',#4966,.T.);
#3463=FACE_OUTER_BOUND('',#4967,.T.);
#3464=FACE_OUTER_BOUND('',#4969,.T.);
#3465=FACE_OUTER_BOUND('',#4971,.T.);
#3466=FACE_OUTER_BOUND('',#4972,.T.);
#3467=FACE_OUTER_BOUND('',#4973,.T.);
#3468=FACE_OUTER_BOUND('',#4975,.T.);
#3469=FACE_OUTER_BOUND('',#4977,.T.);
#3470=FACE_OUTER_BOUND('',#4978,.T.);
#3471=FACE_OUTER_BOUND('',#4979,.T.);
#3472=FACE_OUTER_BOUND('',#4980,.T.);
#3473=FACE_OUTER_BOUND('',#4981,.T.);
#3474=FACE_OUTER_BOUND('',#4982,.T.);
#3475=FACE_OUTER_BOUND('',#4983,.T.);
#3476=FACE_OUTER_BOUND('',#4984,.T.);
#3477=FACE_OUTER_BOUND('',#4985,.T.);
#3478=FACE_OUTER_BOUND('',#4986,.T.);
#3479=FACE_OUTER_BOUND('',#4987,.T.);
#3480=FACE_OUTER_BOUND('',#4988,.T.);
#3481=FACE_OUTER_BOUND('',#4989,.T.);
#3482=FACE_OUTER_BOUND('',#4990,.T.);
#3483=FACE_OUTER_BOUND('',#4991,.T.);
#3484=FACE_OUTER_BOUND('',#4992,.T.);
#3485=FACE_OUTER_BOUND('',#4993,.T.);
#3486=FACE_OUTER_BOUND('',#4994,.T.);
#3487=FACE_OUTER_BOUND('',#4996,.T.);
#3488=FACE_OUTER_BOUND('',#4997,.T.);
#3489=FACE_OUTER_BOUND('',#4998,.T.);
#3490=FACE_OUTER_BOUND('',#4999,.T.);
#3491=FACE_OUTER_BOUND('',#5000,.T.);
#3492=FACE_OUTER_BOUND('',#5001,.T.);
#3493=FACE_OUTER_BOUND('',#5002,.T.);
#3494=FACE_OUTER_BOUND('',#5004,.T.);
#3495=FACE_OUTER_BOUND('',#5006,.T.);
#3496=FACE_OUTER_BOUND('',#5007,.T.);
#3497=FACE_OUTER_BOUND('',#5008,.T.);
#3498=FACE_OUTER_BOUND('',#5009,.T.);
#3499=FACE_OUTER_BOUND('',#5010,.T.);
#3500=FACE_OUTER_BOUND('',#5012,.T.);
#3501=FACE_OUTER_BOUND('',#5013,.T.);
#3502=FACE_OUTER_BOUND('',#5014,.T.);
#3503=FACE_OUTER_BOUND('',#5015,.T.);
#3504=FACE_OUTER_BOUND('',#5016,.T.);
#3505=FACE_OUTER_BOUND('',#5017,.T.);
#3506=FACE_OUTER_BOUND('',#5018,.T.);
#3507=FACE_OUTER_BOUND('',#5019,.T.);
#3508=FACE_OUTER_BOUND('',#5020,.T.);
#3509=FACE_OUTER_BOUND('',#5021,.T.);
#3510=FACE_OUTER_BOUND('',#5022,.T.);
#3511=FACE_OUTER_BOUND('',#5023,.T.);
#3512=FACE_OUTER_BOUND('',#5024,.T.);
#3513=FACE_OUTER_BOUND('',#5025,.T.);
#3514=FACE_OUTER_BOUND('',#5026,.T.);
#3515=FACE_OUTER_BOUND('',#5027,.T.);
#3516=FACE_OUTER_BOUND('',#5028,.T.);
#3517=FACE_OUTER_BOUND('',#5029,.T.);
#3518=FACE_OUTER_BOUND('',#5030,.T.);
#3519=FACE_OUTER_BOUND('',#5031,.T.);
#3520=FACE_OUTER_BOUND('',#5032,.T.);
#3521=FACE_OUTER_BOUND('',#5033,.T.);
#3522=FACE_OUTER_BOUND('',#5034,.T.);
#3523=FACE_OUTER_BOUND('',#5035,.T.);
#3524=FACE_OUTER_BOUND('',#5036,.T.);
#3525=FACE_OUTER_BOUND('',#5037,.T.);
#3526=FACE_OUTER_BOUND('',#5038,.T.);
#3527=FACE_OUTER_BOUND('',#5039,.T.);
#3528=FACE_OUTER_BOUND('',#5040,.T.);
#3529=FACE_OUTER_BOUND('',#5041,.T.);
#3530=FACE_OUTER_BOUND('',#5043,.T.);
#3531=FACE_OUTER_BOUND('',#5044,.T.);
#3532=FACE_OUTER_BOUND('',#5046,.T.);
#3533=FACE_OUTER_BOUND('',#5047,.T.);
#3534=FACE_OUTER_BOUND('',#5049,.T.);
#3535=FACE_OUTER_BOUND('',#5050,.T.);
#3536=FACE_OUTER_BOUND('',#5052,.T.);
#3537=FACE_OUTER_BOUND('',#5053,.T.);
#3538=FACE_OUTER_BOUND('',#5054,.T.);
#3539=FACE_OUTER_BOUND('',#5055,.T.);
#3540=FACE_OUTER_BOUND('',#5056,.T.);
#3541=FACE_OUTER_BOUND('',#5057,.T.);
#3542=FACE_OUTER_BOUND('',#5058,.T.);
#3543=FACE_OUTER_BOUND('',#5059,.T.);
#3544=FACE_OUTER_BOUND('',#5060,.T.);
#3545=FACE_OUTER_BOUND('',#5061,.T.);
#3546=FACE_OUTER_BOUND('',#5062,.T.);
#3547=FACE_OUTER_BOUND('',#5063,.T.);
#3548=FACE_OUTER_BOUND('',#5064,.T.);
#3549=FACE_OUTER_BOUND('',#5065,.T.);
#3550=FACE_OUTER_BOUND('',#5066,.T.);
#3551=FACE_OUTER_BOUND('',#5067,.T.);
#3552=FACE_OUTER_BOUND('',#5068,.T.);
#3553=FACE_OUTER_BOUND('',#5069,.T.);
#3554=FACE_OUTER_BOUND('',#5070,.T.);
#3555=FACE_OUTER_BOUND('',#5085,.T.);
#3556=FACE_OUTER_BOUND('',#5108,.T.);
#3557=FACE_OUTER_BOUND('',#5109,.T.);
#3558=FACE_OUTER_BOUND('',#5110,.T.);
#3559=FACE_OUTER_BOUND('',#5111,.T.);
#3560=FACE_OUTER_BOUND('',#5112,.T.);
#3561=FACE_OUTER_BOUND('',#5113,.T.);
#3562=FACE_OUTER_BOUND('',#5114,.T.);
#3563=FACE_OUTER_BOUND('',#5115,.T.);
#3564=FACE_OUTER_BOUND('',#5117,.T.);
#3565=FACE_OUTER_BOUND('',#5118,.T.);
#3566=FACE_OUTER_BOUND('',#5120,.T.);
#3567=FACE_OUTER_BOUND('',#5121,.T.);
#3568=FACE_OUTER_BOUND('',#5123,.T.);
#3569=FACE_OUTER_BOUND('',#5124,.T.);
#3570=FACE_OUTER_BOUND('',#5126,.T.);
#3571=FACE_OUTER_BOUND('',#5133,.T.);
#3572=FACE_OUTER_BOUND('',#5134,.T.);
#3573=FACE_OUTER_BOUND('',#5135,.T.);
#3574=FACE_OUTER_BOUND('',#5136,.T.);
#3575=FACE_OUTER_BOUND('',#5137,.T.);
#3576=FACE_OUTER_BOUND('',#5138,.T.);
#3577=FACE_OUTER_BOUND('',#5139,.T.);
#3578=FACE_OUTER_BOUND('',#5140,.T.);
#3579=FACE_OUTER_BOUND('',#5141,.T.);
#3580=FACE_OUTER_BOUND('',#5150,.T.);
#3581=FACE_OUTER_BOUND('',#5151,.T.);
#3582=FACE_OUTER_BOUND('',#5152,.T.);
#3583=FACE_OUTER_BOUND('',#5153,.T.);
#3584=FACE_OUTER_BOUND('',#5154,.T.);
#3585=FACE_OUTER_BOUND('',#5156,.T.);
#3586=FACE_OUTER_BOUND('',#5157,.T.);
#3587=FACE_OUTER_BOUND('',#5158,.T.);
#3588=FACE_OUTER_BOUND('',#5159,.T.);
#3589=FACE_OUTER_BOUND('',#5160,.T.);
#3590=FACE_OUTER_BOUND('',#5161,.T.);
#3591=FACE_OUTER_BOUND('',#5162,.T.);
#3592=FACE_OUTER_BOUND('',#5167,.T.);
#3593=FACE_OUTER_BOUND('',#5168,.T.);
#3594=FACE_OUTER_BOUND('',#5173,.T.);
#3595=FACE_OUTER_BOUND('',#5174,.T.);
#3596=FACE_OUTER_BOUND('',#5177,.T.);
#3597=FACE_OUTER_BOUND('',#5178,.T.);
#3598=FACE_OUTER_BOUND('',#5179,.T.);
#3599=FACE_OUTER_BOUND('',#5180,.T.);
#3600=FACE_OUTER_BOUND('',#5181,.T.);
#3601=FACE_OUTER_BOUND('',#5183,.T.);
#3602=FACE_OUTER_BOUND('',#5184,.T.);
#3603=FACE_OUTER_BOUND('',#5185,.T.);
#3604=FACE_OUTER_BOUND('',#5190,.T.);
#3605=FACE_OUTER_BOUND('',#5195,.T.);
#3606=FACE_OUTER_BOUND('',#5196,.T.);
#3607=FACE_OUTER_BOUND('',#5197,.T.);
#3608=FACE_OUTER_BOUND('',#5198,.T.);
#3609=FACE_OUTER_BOUND('',#5199,.T.);
#3610=FACE_OUTER_BOUND('',#5201,.T.);
#3611=FACE_OUTER_BOUND('',#5202,.T.);
#3612=FACE_OUTER_BOUND('',#5203,.T.);
#3613=FACE_OUTER_BOUND('',#5204,.T.);
#3614=FACE_OUTER_BOUND('',#5205,.T.);
#3615=FACE_OUTER_BOUND('',#5206,.T.);
#3616=FACE_OUTER_BOUND('',#5207,.T.);
#3617=FACE_OUTER_BOUND('',#5212,.T.);
#3618=FACE_OUTER_BOUND('',#5213,.T.);
#3619=FACE_OUTER_BOUND('',#5218,.T.);
#3620=FACE_OUTER_BOUND('',#5219,.T.);
#3621=FACE_OUTER_BOUND('',#5222,.T.);
#3622=FACE_OUTER_BOUND('',#5223,.T.);
#3623=FACE_OUTER_BOUND('',#5224,.T.);
#3624=FACE_OUTER_BOUND('',#5225,.T.);
#3625=FACE_OUTER_BOUND('',#5226,.T.);
#3626=FACE_OUTER_BOUND('',#5231,.T.);
#3627=FACE_OUTER_BOUND('',#5232,.T.);
#3628=FACE_OUTER_BOUND('',#5233,.T.);
#3629=FACE_OUTER_BOUND('',#5235,.T.);
#3630=FACE_OUTER_BOUND('',#5236,.T.);
#3631=FACE_OUTER_BOUND('',#5241,.T.);
#3632=FACE_OUTER_BOUND('',#5242,.T.);
#3633=FACE_OUTER_BOUND('',#5244,.T.);
#3634=FACE_OUTER_BOUND('',#5245,.T.);
#3635=FACE_OUTER_BOUND('',#5246,.T.);
#3636=FACE_OUTER_BOUND('',#5247,.T.);
#3637=FACE_OUTER_BOUND('',#5248,.T.);
#3638=FACE_OUTER_BOUND('',#5249,.T.);
#3639=FACE_OUTER_BOUND('',#5251,.T.);
#3640=FACE_OUTER_BOUND('',#5253,.T.);
#3641=FACE_OUTER_BOUND('',#5254,.T.);
#3642=FACE_OUTER_BOUND('',#5256,.T.);
#3643=FACE_OUTER_BOUND('',#5257,.T.);
#3644=FACE_OUTER_BOUND('',#5258,.T.);
#3645=FACE_OUTER_BOUND('',#5259,.T.);
#3646=FACE_OUTER_BOUND('',#5260,.T.);
#3647=FACE_OUTER_BOUND('',#5261,.T.);
#3648=FACE_OUTER_BOUND('',#5263,.T.);
#3649=FACE_OUTER_BOUND('',#5265,.T.);
#3650=FACE_OUTER_BOUND('',#5266,.T.);
#3651=FACE_OUTER_BOUND('',#5268,.T.);
#3652=FACE_OUTER_BOUND('',#5269,.T.);
#3653=FACE_OUTER_BOUND('',#5271,.T.);
#3654=FACE_OUTER_BOUND('',#5272,.T.);
#3655=FACE_OUTER_BOUND('',#5274,.T.);
#3656=FACE_OUTER_BOUND('',#5275,.T.);
#3657=FACE_OUTER_BOUND('',#5277,.T.);
#3658=FACE_OUTER_BOUND('',#5278,.T.);
#3659=FACE_OUTER_BOUND('',#5279,.T.);
#3660=FACE_OUTER_BOUND('',#5280,.T.);
#3661=FACE_OUTER_BOUND('',#5281,.T.);
#3662=FACE_OUTER_BOUND('',#5282,.T.);
#3663=FACE_OUTER_BOUND('',#5283,.T.);
#3664=FACE_OUTER_BOUND('',#5284,.T.);
#3665=FACE_OUTER_BOUND('',#5285,.T.);
#3666=FACE_OUTER_BOUND('',#5290,.T.);
#3667=FACE_OUTER_BOUND('',#5291,.T.);
#3668=FACE_OUTER_BOUND('',#5292,.T.);
#3669=FACE_OUTER_BOUND('',#5293,.T.);
#3670=FACE_OUTER_BOUND('',#5294,.T.);
#3671=FACE_OUTER_BOUND('',#5295,.T.);
#3672=FACE_OUTER_BOUND('',#5300,.T.);
#3673=FACE_OUTER_BOUND('',#5301,.T.);
#3674=FACE_OUTER_BOUND('',#5302,.T.);
#3675=FACE_OUTER_BOUND('',#5303,.T.);
#3676=FACE_OUTER_BOUND('',#5304,.T.);
#3677=FACE_OUTER_BOUND('',#5305,.T.);
#3678=FACE_OUTER_BOUND('',#5306,.T.);
#3679=FACE_OUTER_BOUND('',#5307,.T.);
#3680=FACE_OUTER_BOUND('',#5309,.T.);
#3681=FACE_OUTER_BOUND('',#5310,.T.);
#3682=FACE_OUTER_BOUND('',#5312,.T.);
#3683=FACE_OUTER_BOUND('',#5313,.T.);
#3684=FACE_OUTER_BOUND('',#5314,.T.);
#3685=FACE_OUTER_BOUND('',#5315,.T.);
#3686=FACE_OUTER_BOUND('',#5317,.T.);
#3687=FACE_OUTER_BOUND('',#5318,.T.);
#3688=FACE_OUTER_BOUND('',#5319,.T.);
#3689=FACE_OUTER_BOUND('',#5320,.T.);
#3690=FACE_OUTER_BOUND('',#5322,.T.);
#3691=FACE_OUTER_BOUND('',#5323,.T.);
#3692=FACE_OUTER_BOUND('',#5324,.T.);
#3693=FACE_OUTER_BOUND('',#5325,.T.);
#3694=FACE_OUTER_BOUND('',#5326,.T.);
#3695=FACE_OUTER_BOUND('',#5327,.T.);
#3696=FACE_OUTER_BOUND('',#5328,.T.);
#3697=FACE_OUTER_BOUND('',#5329,.T.);
#3698=FACE_OUTER_BOUND('',#5330,.T.);
#3699=FACE_OUTER_BOUND('',#5331,.T.);
#3700=FACE_OUTER_BOUND('',#5332,.T.);
#3701=FACE_OUTER_BOUND('',#5333,.T.);
#3702=FACE_OUTER_BOUND('',#5334,.T.);
#3703=FACE_OUTER_BOUND('',#5335,.T.);
#3704=FACE_OUTER_BOUND('',#5336,.T.);
#3705=FACE_OUTER_BOUND('',#5337,.T.);
#3706=FACE_OUTER_BOUND('',#5338,.T.);
#3707=FACE_OUTER_BOUND('',#5339,.T.);
#3708=FACE_OUTER_BOUND('',#5340,.T.);
#3709=FACE_OUTER_BOUND('',#5341,.T.);
#3710=FACE_OUTER_BOUND('',#5342,.T.);
#3711=FACE_OUTER_BOUND('',#5343,.T.);
#3712=FACE_OUTER_BOUND('',#5344,.T.);
#3713=FACE_OUTER_BOUND('',#5345,.T.);
#3714=FACE_OUTER_BOUND('',#5347,.T.);
#3715=FACE_OUTER_BOUND('',#5348,.T.);
#3716=FACE_OUTER_BOUND('',#5350,.T.);
#3717=FACE_OUTER_BOUND('',#5351,.T.);
#3718=FACE_OUTER_BOUND('',#5353,.T.);
#3719=FACE_OUTER_BOUND('',#5354,.T.);
#3720=FACE_OUTER_BOUND('',#5356,.T.);
#3721=FACE_OUTER_BOUND('',#5357,.T.);
#3722=FACE_OUTER_BOUND('',#5359,.T.);
#3723=FACE_OUTER_BOUND('',#5360,.T.);
#3724=FACE_OUTER_BOUND('',#5361,.T.);
#3725=FACE_OUTER_BOUND('',#5362,.T.);
#3726=FACE_OUTER_BOUND('',#5363,.T.);
#3727=FACE_OUTER_BOUND('',#5364,.T.);
#3728=FACE_OUTER_BOUND('',#5366,.T.);
#3729=FACE_OUTER_BOUND('',#5367,.T.);
#3730=FACE_OUTER_BOUND('',#5369,.T.);
#3731=FACE_OUTER_BOUND('',#5370,.T.);
#3732=FACE_OUTER_BOUND('',#5371,.T.);
#3733=FACE_OUTER_BOUND('',#5372,.T.);
#3734=FACE_OUTER_BOUND('',#5374,.T.);
#3735=FACE_OUTER_BOUND('',#5375,.T.);
#3736=FACE_OUTER_BOUND('',#5376,.T.);
#3737=FACE_OUTER_BOUND('',#5377,.T.);
#3738=FACE_OUTER_BOUND('',#5379,.T.);
#3739=FACE_OUTER_BOUND('',#5380,.T.);
#3740=FACE_OUTER_BOUND('',#5381,.T.);
#3741=FACE_OUTER_BOUND('',#5382,.T.);
#3742=FACE_OUTER_BOUND('',#5383,.T.);
#3743=FACE_OUTER_BOUND('',#5384,.T.);
#3744=FACE_OUTER_BOUND('',#5385,.T.);
#3745=FACE_OUTER_BOUND('',#5386,.T.);
#3746=FACE_OUTER_BOUND('',#5387,.T.);
#3747=FACE_OUTER_BOUND('',#5388,.T.);
#3748=FACE_OUTER_BOUND('',#5389,.T.);
#3749=FACE_OUTER_BOUND('',#5390,.T.);
#3750=FACE_OUTER_BOUND('',#5391,.T.);
#3751=FACE_OUTER_BOUND('',#5392,.T.);
#3752=FACE_OUTER_BOUND('',#5393,.T.);
#3753=FACE_OUTER_BOUND('',#5394,.T.);
#3754=FACE_OUTER_BOUND('',#5395,.T.);
#3755=FACE_OUTER_BOUND('',#5396,.T.);
#3756=FACE_OUTER_BOUND('',#5397,.T.);
#3757=FACE_OUTER_BOUND('',#5398,.T.);
#3758=FACE_OUTER_BOUND('',#5399,.T.);
#3759=FACE_OUTER_BOUND('',#5400,.T.);
#3760=FACE_OUTER_BOUND('',#5401,.T.);
#3761=FACE_OUTER_BOUND('',#5402,.T.);
#3762=FACE_OUTER_BOUND('',#5403,.T.);
#3763=FACE_OUTER_BOUND('',#5404,.T.);
#3764=FACE_OUTER_BOUND('',#5405,.T.);
#3765=FACE_OUTER_BOUND('',#5407,.T.);
#3766=FACE_OUTER_BOUND('',#5408,.T.);
#3767=FACE_OUTER_BOUND('',#5410,.T.);
#3768=FACE_OUTER_BOUND('',#5411,.T.);
#3769=FACE_OUTER_BOUND('',#5413,.T.);
#3770=FACE_OUTER_BOUND('',#5414,.T.);
#3771=FACE_OUTER_BOUND('',#5416,.T.);
#3772=FACE_OUTER_BOUND('',#5417,.T.);
#3773=FACE_OUTER_BOUND('',#5419,.T.);
#3774=FACE_OUTER_BOUND('',#5420,.T.);
#3775=FACE_OUTER_BOUND('',#5421,.T.);
#3776=FACE_OUTER_BOUND('',#5422,.T.);
#3777=FACE_OUTER_BOUND('',#5423,.T.);
#3778=FACE_OUTER_BOUND('',#5424,.T.);
#3779=FACE_OUTER_BOUND('',#5425,.T.);
#3780=FACE_OUTER_BOUND('',#5426,.T.);
#3781=FACE_OUTER_BOUND('',#5427,.T.);
#3782=FACE_OUTER_BOUND('',#5428,.T.);
#3783=FACE_OUTER_BOUND('',#5429,.T.);
#3784=FACE_OUTER_BOUND('',#5430,.T.);
#3785=FACE_OUTER_BOUND('',#5431,.T.);
#3786=FACE_OUTER_BOUND('',#5432,.T.);
#3787=FACE_OUTER_BOUND('',#5433,.T.);
#3788=FACE_OUTER_BOUND('',#5435,.T.);
#3789=FACE_OUTER_BOUND('',#5436,.T.);
#3790=FACE_OUTER_BOUND('',#5437,.T.);
#3791=FACE_OUTER_BOUND('',#5438,.T.);
#3792=FACE_OUTER_BOUND('',#5439,.T.);
#3793=FACE_OUTER_BOUND('',#5440,.T.);
#3794=FACE_OUTER_BOUND('',#5441,.T.);
#3795=FACE_OUTER_BOUND('',#5442,.T.);
#3796=FACE_OUTER_BOUND('',#5443,.T.);
#3797=FACE_OUTER_BOUND('',#5444,.T.);
#3798=FACE_OUTER_BOUND('',#5445,.T.);
#3799=FACE_OUTER_BOUND('',#5450,.T.);
#3800=FACE_OUTER_BOUND('',#5455,.T.);
#3801=FACE_OUTER_BOUND('',#5456,.T.);
#3802=FACE_OUTER_BOUND('',#5457,.T.);
#3803=FACE_OUTER_BOUND('',#5458,.T.);
#3804=FACE_OUTER_BOUND('',#5459,.T.);
#3805=FACE_OUTER_BOUND('',#5460,.T.);
#3806=FACE_OUTER_BOUND('',#5461,.T.);
#3807=FACE_OUTER_BOUND('',#5462,.T.);
#3808=FACE_OUTER_BOUND('',#5463,.T.);
#3809=FACE_OUTER_BOUND('',#5464,.T.);
#3810=FACE_OUTER_BOUND('',#5465,.T.);
#3811=FACE_OUTER_BOUND('',#5466,.T.);
#3812=FACE_OUTER_BOUND('',#5467,.T.);
#3813=FACE_OUTER_BOUND('',#5476,.T.);
#3814=FACE_OUTER_BOUND('',#5485,.T.);
#3815=FACE_OUTER_BOUND('',#5486,.T.);
#3816=FACE_OUTER_BOUND('',#5487,.T.);
#3817=FACE_OUTER_BOUND('',#5488,.T.);
#3818=FACE_OUTER_BOUND('',#5489,.T.);
#3819=FACE_OUTER_BOUND('',#5490,.T.);
#3820=FACE_OUTER_BOUND('',#5491,.T.);
#3821=FACE_OUTER_BOUND('',#5492,.T.);
#3822=FACE_OUTER_BOUND('',#5493,.T.);
#3823=FACE_OUTER_BOUND('',#5494,.T.);
#3824=FACE_OUTER_BOUND('',#5495,.T.);
#3825=FACE_OUTER_BOUND('',#5496,.T.);
#3826=FACE_OUTER_BOUND('',#5497,.T.);
#3827=FACE_OUTER_BOUND('',#5498,.T.);
#3828=FACE_OUTER_BOUND('',#5499,.T.);
#3829=FACE_OUTER_BOUND('',#5500,.T.);
#3830=FACE_OUTER_BOUND('',#5501,.T.);
#3831=FACE_OUTER_BOUND('',#5506,.T.);
#3832=FACE_OUTER_BOUND('',#5507,.T.);
#3833=FACE_OUTER_BOUND('',#5509,.T.);
#3834=FACE_OUTER_BOUND('',#5514,.T.);
#3835=FACE_OUTER_BOUND('',#5515,.T.);
#3836=FACE_OUTER_BOUND('',#5516,.T.);
#3837=FACE_OUTER_BOUND('',#5517,.T.);
#3838=FACE_OUTER_BOUND('',#5518,.T.);
#3839=FACE_OUTER_BOUND('',#5519,.T.);
#3840=FACE_OUTER_BOUND('',#5520,.T.);
#3841=FACE_OUTER_BOUND('',#5521,.T.);
#3842=FACE_OUTER_BOUND('',#5522,.T.);
#3843=FACE_OUTER_BOUND('',#5523,.T.);
#3844=FACE_OUTER_BOUND('',#5524,.T.);
#3845=FACE_OUTER_BOUND('',#5525,.T.);
#3846=FACE_OUTER_BOUND('',#5526,.T.);
#3847=FACE_OUTER_BOUND('',#5527,.T.);
#3848=FACE_OUTER_BOUND('',#5528,.T.);
#3849=FACE_OUTER_BOUND('',#5533,.T.);
#3850=FACE_OUTER_BOUND('',#5534,.T.);
#3851=FACE_OUTER_BOUND('',#5535,.T.);
#3852=FACE_OUTER_BOUND('',#5536,.T.);
#3853=FACE_OUTER_BOUND('',#5537,.T.);
#3854=FACE_OUTER_BOUND('',#5538,.T.);
#3855=FACE_OUTER_BOUND('',#5539,.T.);
#3856=FACE_OUTER_BOUND('',#5540,.T.);
#3857=FACE_OUTER_BOUND('',#5541,.T.);
#3858=FACE_OUTER_BOUND('',#5542,.T.);
#3859=FACE_OUTER_BOUND('',#5543,.T.);
#3860=FACE_OUTER_BOUND('',#5544,.T.);
#3861=FACE_OUTER_BOUND('',#5545,.T.);
#3862=FACE_OUTER_BOUND('',#5546,.T.);
#3863=FACE_OUTER_BOUND('',#5547,.T.);
#3864=FACE_OUTER_BOUND('',#5548,.T.);
#3865=FACE_OUTER_BOUND('',#5549,.T.);
#3866=FACE_OUTER_BOUND('',#5550,.T.);
#3867=FACE_OUTER_BOUND('',#5551,.T.);
#3868=FACE_OUTER_BOUND('',#5552,.T.);
#3869=FACE_OUTER_BOUND('',#5553,.T.);
#3870=FACE_OUTER_BOUND('',#5554,.T.);
#3871=FACE_OUTER_BOUND('',#5555,.T.);
#3872=FACE_OUTER_BOUND('',#5556,.T.);
#3873=FACE_OUTER_BOUND('',#5557,.T.);
#3874=FACE_OUTER_BOUND('',#5558,.T.);
#3875=FACE_OUTER_BOUND('',#5559,.T.);
#3876=FACE_OUTER_BOUND('',#5560,.T.);
#3877=FACE_OUTER_BOUND('',#5561,.T.);
#3878=FACE_OUTER_BOUND('',#5562,.T.);
#3879=FACE_OUTER_BOUND('',#5563,.T.);
#3880=FACE_OUTER_BOUND('',#5565,.T.);
#3881=FACE_OUTER_BOUND('',#5566,.T.);
#3882=FACE_OUTER_BOUND('',#5568,.T.);
#3883=FACE_OUTER_BOUND('',#5569,.T.);
#3884=FACE_OUTER_BOUND('',#5570,.T.);
#3885=FACE_OUTER_BOUND('',#5571,.T.);
#3886=FACE_OUTER_BOUND('',#5572,.T.);
#3887=FACE_OUTER_BOUND('',#5573,.T.);
#3888=FACE_OUTER_BOUND('',#5574,.T.);
#3889=FACE_OUTER_BOUND('',#5575,.T.);
#3890=FACE_OUTER_BOUND('',#5576,.T.);
#3891=FACE_OUTER_BOUND('',#5578,.T.);
#3892=FACE_OUTER_BOUND('',#5579,.T.);
#3893=FACE_OUTER_BOUND('',#5580,.T.);
#3894=FACE_OUTER_BOUND('',#5581,.T.);
#3895=FACE_OUTER_BOUND('',#5582,.T.);
#3896=FACE_OUTER_BOUND('',#5583,.T.);
#3897=FACE_OUTER_BOUND('',#5584,.T.);
#3898=FACE_OUTER_BOUND('',#5586,.T.);
#3899=FACE_OUTER_BOUND('',#5587,.T.);
#3900=FACE_OUTER_BOUND('',#5588,.T.);
#3901=FACE_OUTER_BOUND('',#5589,.T.);
#3902=FACE_OUTER_BOUND('',#5590,.T.);
#3903=FACE_OUTER_BOUND('',#5591,.T.);
#3904=FACE_OUTER_BOUND('',#5592,.T.);
#3905=FACE_OUTER_BOUND('',#5593,.T.);
#3906=FACE_OUTER_BOUND('',#5594,.T.);
#3907=FACE_OUTER_BOUND('',#5595,.T.);
#3908=FACE_OUTER_BOUND('',#5596,.T.);
#3909=FACE_OUTER_BOUND('',#5597,.T.);
#3910=FACE_OUTER_BOUND('',#5598,.T.);
#3911=FACE_OUTER_BOUND('',#5599,.T.);
#3912=FACE_OUTER_BOUND('',#5600,.T.);
#3913=FACE_OUTER_BOUND('',#5601,.T.);
#3914=FACE_OUTER_BOUND('',#5602,.T.);
#3915=FACE_OUTER_BOUND('',#5603,.T.);
#3916=FACE_OUTER_BOUND('',#5604,.T.);
#3917=FACE_OUTER_BOUND('',#5605,.T.);
#3918=FACE_OUTER_BOUND('',#5606,.T.);
#3919=FACE_OUTER_BOUND('',#5607,.T.);
#3920=FACE_OUTER_BOUND('',#5608,.T.);
#3921=FACE_OUTER_BOUND('',#5609,.T.);
#3922=FACE_OUTER_BOUND('',#5614,.T.);
#3923=FACE_OUTER_BOUND('',#5615,.T.);
#3924=FACE_OUTER_BOUND('',#5616,.T.);
#3925=FACE_OUTER_BOUND('',#5617,.T.);
#3926=FACE_OUTER_BOUND('',#5618,.T.);
#3927=FACE_OUTER_BOUND('',#5623,.T.);
#3928=FACE_OUTER_BOUND('',#5624,.T.);
#3929=FACE_OUTER_BOUND('',#5625,.T.);
#3930=FACE_OUTER_BOUND('',#5626,.T.);
#3931=FACE_OUTER_BOUND('',#5628,.T.);
#3932=FACE_OUTER_BOUND('',#5629,.T.);
#3933=FACE_OUTER_BOUND('',#5630,.T.);
#3934=FACE_OUTER_BOUND('',#5631,.T.);
#3935=FACE_OUTER_BOUND('',#5632,.T.);
#3936=FACE_OUTER_BOUND('',#5634,.T.);
#3937=FACE_OUTER_BOUND('',#5635,.T.);
#3938=FACE_OUTER_BOUND('',#5636,.T.);
#3939=FACE_OUTER_BOUND('',#5637,.T.);
#3940=FACE_OUTER_BOUND('',#5638,.T.);
#3941=FACE_OUTER_BOUND('',#5639,.T.);
#3942=FACE_OUTER_BOUND('',#5640,.T.);
#3943=FACE_OUTER_BOUND('',#5641,.T.);
#3944=FACE_OUTER_BOUND('',#5642,.T.);
#3945=FACE_OUTER_BOUND('',#5643,.T.);
#3946=FACE_OUTER_BOUND('',#5644,.T.);
#3947=FACE_OUTER_BOUND('',#5645,.T.);
#3948=FACE_OUTER_BOUND('',#5646,.T.);
#3949=FACE_OUTER_BOUND('',#5647,.T.);
#3950=FACE_OUTER_BOUND('',#5648,.T.);
#3951=FACE_OUTER_BOUND('',#5649,.T.);
#3952=FACE_OUTER_BOUND('',#5650,.T.);
#3953=FACE_OUTER_BOUND('',#5652,.T.);
#3954=FACE_OUTER_BOUND('',#5653,.T.);
#3955=FACE_OUTER_BOUND('',#5654,.T.);
#3956=FACE_OUTER_BOUND('',#5655,.T.);
#3957=FACE_OUTER_BOUND('',#5656,.T.);
#3958=FACE_OUTER_BOUND('',#5657,.T.);
#3959=FACE_OUTER_BOUND('',#5658,.T.);
#3960=FACE_OUTER_BOUND('',#5659,.T.);
#3961=FACE_OUTER_BOUND('',#5660,.T.);
#3962=FACE_OUTER_BOUND('',#5661,.T.);
#3963=FACE_OUTER_BOUND('',#5662,.T.);
#3964=FACE_OUTER_BOUND('',#5663,.T.);
#3965=FACE_OUTER_BOUND('',#5664,.T.);
#3966=FACE_OUTER_BOUND('',#5665,.T.);
#3967=FACE_OUTER_BOUND('',#5666,.T.);
#3968=FACE_OUTER_BOUND('',#5667,.T.);
#3969=FACE_OUTER_BOUND('',#5668,.T.);
#3970=FACE_OUTER_BOUND('',#5669,.T.);
#3971=FACE_OUTER_BOUND('',#5670,.T.);
#3972=FACE_OUTER_BOUND('',#5671,.T.);
#3973=FACE_OUTER_BOUND('',#5672,.T.);
#3974=FACE_OUTER_BOUND('',#5673,.T.);
#3975=FACE_OUTER_BOUND('',#5674,.T.);
#3976=FACE_OUTER_BOUND('',#5675,.T.);
#3977=FACE_OUTER_BOUND('',#5676,.T.);
#3978=FACE_OUTER_BOUND('',#5677,.T.);
#3979=FACE_OUTER_BOUND('',#5678,.T.);
#3980=FACE_OUTER_BOUND('',#5679,.T.);
#3981=FACE_OUTER_BOUND('',#5680,.T.);
#3982=FACE_OUTER_BOUND('',#5681,.T.);
#3983=FACE_OUTER_BOUND('',#5682,.T.);
#3984=FACE_OUTER_BOUND('',#5683,.T.);
#3985=FACE_OUTER_BOUND('',#5684,.T.);
#3986=FACE_OUTER_BOUND('',#5685,.T.);
#3987=FACE_OUTER_BOUND('',#5686,.T.);
#3988=FACE_OUTER_BOUND('',#5687,.T.);
#3989=FACE_OUTER_BOUND('',#5688,.T.);
#3990=FACE_OUTER_BOUND('',#5689,.T.);
#3991=FACE_OUTER_BOUND('',#5690,.T.);
#3992=FACE_OUTER_BOUND('',#5691,.T.);
#3993=FACE_OUTER_BOUND('',#5692,.T.);
#3994=FACE_OUTER_BOUND('',#5693,.T.);
#3995=FACE_OUTER_BOUND('',#5694,.T.);
#3996=FACE_OUTER_BOUND('',#5695,.T.);
#3997=FACE_OUTER_BOUND('',#5696,.T.);
#3998=FACE_OUTER_BOUND('',#5697,.T.);
#3999=FACE_OUTER_BOUND('',#5698,.T.);
#4000=FACE_OUTER_BOUND('',#5699,.T.);
#4001=FACE_OUTER_BOUND('',#5700,.T.);
#4002=FACE_OUTER_BOUND('',#5701,.T.);
#4003=FACE_OUTER_BOUND('',#5702,.T.);
#4004=FACE_OUTER_BOUND('',#5703,.T.);
#4005=FACE_OUTER_BOUND('',#5704,.T.);
#4006=FACE_OUTER_BOUND('',#5705,.T.);
#4007=FACE_OUTER_BOUND('',#5706,.T.);
#4008=FACE_OUTER_BOUND('',#5707,.T.);
#4009=FACE_OUTER_BOUND('',#5708,.T.);
#4010=FACE_OUTER_BOUND('',#5709,.T.);
#4011=FACE_OUTER_BOUND('',#5710,.T.);
#4012=FACE_OUTER_BOUND('',#5711,.T.);
#4013=FACE_OUTER_BOUND('',#5712,.T.);
#4014=FACE_OUTER_BOUND('',#5713,.T.);
#4015=FACE_OUTER_BOUND('',#5714,.T.);
#4016=FACE_OUTER_BOUND('',#5715,.T.);
#4017=FACE_OUTER_BOUND('',#5716,.T.);
#4018=FACE_OUTER_BOUND('',#5717,.T.);
#4019=FACE_OUTER_BOUND('',#5718,.T.);
#4020=FACE_OUTER_BOUND('',#5719,.T.);
#4021=FACE_OUTER_BOUND('',#5720,.T.);
#4022=FACE_OUTER_BOUND('',#5721,.T.);
#4023=FACE_OUTER_BOUND('',#5722,.T.);
#4024=FACE_OUTER_BOUND('',#5723,.T.);
#4025=FACE_OUTER_BOUND('',#5724,.T.);
#4026=FACE_OUTER_BOUND('',#5725,.T.);
#4027=FACE_OUTER_BOUND('',#5726,.T.);
#4028=FACE_OUTER_BOUND('',#5727,.T.);
#4029=FACE_OUTER_BOUND('',#5728,.T.);
#4030=FACE_OUTER_BOUND('',#5729,.T.);
#4031=FACE_OUTER_BOUND('',#5730,.T.);
#4032=FACE_OUTER_BOUND('',#5731,.T.);
#4033=FACE_OUTER_BOUND('',#5732,.T.);
#4034=FACE_OUTER_BOUND('',#5733,.T.);
#4035=FACE_OUTER_BOUND('',#5734,.T.);
#4036=FACE_OUTER_BOUND('',#5735,.T.);
#4037=FACE_OUTER_BOUND('',#5736,.T.);
#4038=FACE_OUTER_BOUND('',#5737,.T.);
#4039=FACE_OUTER_BOUND('',#5738,.T.);
#4040=FACE_OUTER_BOUND('',#5739,.T.);
#4041=FACE_OUTER_BOUND('',#5740,.T.);
#4042=FACE_OUTER_BOUND('',#5741,.T.);
#4043=FACE_OUTER_BOUND('',#5742,.T.);
#4044=FACE_OUTER_BOUND('',#5743,.T.);
#4045=FACE_OUTER_BOUND('',#5744,.T.);
#4046=FACE_OUTER_BOUND('',#5745,.T.);
#4047=FACE_OUTER_BOUND('',#5746,.T.);
#4048=FACE_OUTER_BOUND('',#5747,.T.);
#4049=FACE_OUTER_BOUND('',#5748,.T.);
#4050=FACE_OUTER_BOUND('',#5749,.T.);
#4051=FACE_OUTER_BOUND('',#5750,.T.);
#4052=FACE_OUTER_BOUND('',#5751,.T.);
#4053=FACE_OUTER_BOUND('',#5752,.T.);
#4054=FACE_OUTER_BOUND('',#5753,.T.);
#4055=FACE_OUTER_BOUND('',#5754,.T.);
#4056=FACE_OUTER_BOUND('',#5755,.T.);
#4057=FACE_OUTER_BOUND('',#5756,.T.);
#4058=FACE_OUTER_BOUND('',#5757,.T.);
#4059=FACE_OUTER_BOUND('',#5758,.T.);
#4060=FACE_OUTER_BOUND('',#5759,.T.);
#4061=FACE_OUTER_BOUND('',#5760,.T.);
#4062=FACE_OUTER_BOUND('',#5761,.T.);
#4063=FACE_OUTER_BOUND('',#5762,.T.);
#4064=FACE_OUTER_BOUND('',#5763,.T.);
#4065=FACE_OUTER_BOUND('',#5764,.T.);
#4066=FACE_OUTER_BOUND('',#5765,.T.);
#4067=FACE_OUTER_BOUND('',#5766,.T.);
#4068=FACE_OUTER_BOUND('',#5767,.T.);
#4069=FACE_OUTER_BOUND('',#5768,.T.);
#4070=FACE_OUTER_BOUND('',#5769,.T.);
#4071=FACE_OUTER_BOUND('',#5770,.T.);
#4072=FACE_OUTER_BOUND('',#5771,.T.);
#4073=FACE_OUTER_BOUND('',#5772,.T.);
#4074=FACE_OUTER_BOUND('',#5773,.T.);
#4075=FACE_OUTER_BOUND('',#5774,.T.);
#4076=FACE_OUTER_BOUND('',#5775,.T.);
#4077=FACE_OUTER_BOUND('',#5776,.T.);
#4078=FACE_OUTER_BOUND('',#5777,.T.);
#4079=FACE_OUTER_BOUND('',#5778,.T.);
#4080=FACE_OUTER_BOUND('',#5779,.T.);
#4081=FACE_OUTER_BOUND('',#5780,.T.);
#4082=FACE_OUTER_BOUND('',#5781,.T.);
#4083=FACE_OUTER_BOUND('',#5782,.T.);
#4084=FACE_OUTER_BOUND('',#5783,.T.);
#4085=FACE_OUTER_BOUND('',#5784,.T.);
#4086=FACE_OUTER_BOUND('',#5785,.T.);
#4087=FACE_OUTER_BOUND('',#5786,.T.);
#4088=FACE_OUTER_BOUND('',#5787,.T.);
#4089=FACE_OUTER_BOUND('',#5788,.T.);
#4090=FACE_OUTER_BOUND('',#5789,.T.);
#4091=FACE_OUTER_BOUND('',#5790,.T.);
#4092=FACE_OUTER_BOUND('',#5792,.T.);
#4093=FACE_OUTER_BOUND('',#5793,.T.);
#4094=FACE_OUTER_BOUND('',#5794,.T.);
#4095=FACE_OUTER_BOUND('',#5795,.T.);
#4096=FACE_OUTER_BOUND('',#5796,.T.);
#4097=FACE_OUTER_BOUND('',#5797,.T.);
#4098=FACE_OUTER_BOUND('',#5798,.T.);
#4099=FACE_OUTER_BOUND('',#5799,.T.);
#4100=FACE_OUTER_BOUND('',#5800,.T.);
#4101=FACE_OUTER_BOUND('',#5801,.T.);
#4102=FACE_OUTER_BOUND('',#5802,.T.);
#4103=FACE_OUTER_BOUND('',#5804,.T.);
#4104=FACE_OUTER_BOUND('',#5805,.T.);
#4105=FACE_OUTER_BOUND('',#5807,.T.);
#4106=FACE_OUTER_BOUND('',#5808,.T.);
#4107=FACE_OUTER_BOUND('',#5810,.T.);
#4108=FACE_OUTER_BOUND('',#5811,.T.);
#4109=FACE_OUTER_BOUND('',#5812,.T.);
#4110=FACE_OUTER_BOUND('',#5813,.T.);
#4111=FACE_OUTER_BOUND('',#5815,.T.);
#4112=FACE_OUTER_BOUND('',#5817,.T.);
#4113=FACE_OUTER_BOUND('',#5818,.T.);
#4114=FACE_OUTER_BOUND('',#5819,.T.);
#4115=FACE_OUTER_BOUND('',#5820,.T.);
#4116=FACE_OUTER_BOUND('',#5822,.T.);
#4117=FACE_OUTER_BOUND('',#5824,.T.);
#4118=FACE_OUTER_BOUND('',#5826,.T.);
#4119=FACE_OUTER_BOUND('',#5828,.T.);
#4120=FACE_OUTER_BOUND('',#5829,.T.);
#4121=FACE_OUTER_BOUND('',#5830,.T.);
#4122=FACE_OUTER_BOUND('',#5831,.T.);
#4123=FACE_OUTER_BOUND('',#5832,.T.);
#4124=FACE_OUTER_BOUND('',#5833,.T.);
#4125=FACE_OUTER_BOUND('',#5834,.T.);
#4126=FACE_OUTER_BOUND('',#5835,.T.);
#4127=FACE_OUTER_BOUND('',#5838,.T.);
#4128=FACE_OUTER_BOUND('',#5841,.T.);
#4129=FACE_OUTER_BOUND('',#5842,.T.);
#4130=FACE_OUTER_BOUND('',#5844,.T.);
#4131=FACE_OUTER_BOUND('',#5846,.T.);
#4132=FACE_OUTER_BOUND('',#5847,.T.);
#4133=FACE_OUTER_BOUND('',#5848,.T.);
#4134=FACE_OUTER_BOUND('',#5849,.T.);
#4135=FACE_OUTER_BOUND('',#5851,.T.);
#4136=FACE_OUTER_BOUND('',#5853,.T.);
#4137=FACE_OUTER_BOUND('',#5854,.T.);
#4138=FACE_OUTER_BOUND('',#5855,.T.);
#4139=FACE_OUTER_BOUND('',#5857,.T.);
#4140=FACE_OUTER_BOUND('',#5859,.T.);
#4141=FACE_OUTER_BOUND('',#5860,.T.);
#4142=FACE_OUTER_BOUND('',#5861,.T.);
#4143=FACE_OUTER_BOUND('',#5862,.T.);
#4144=FACE_OUTER_BOUND('',#5863,.T.);
#4145=FACE_OUTER_BOUND('',#5864,.T.);
#4146=FACE_OUTER_BOUND('',#5865,.T.);
#4147=FACE_OUTER_BOUND('',#5866,.T.);
#4148=FACE_OUTER_BOUND('',#5867,.T.);
#4149=FACE_OUTER_BOUND('',#5868,.T.);
#4150=FACE_OUTER_BOUND('',#5869,.T.);
#4151=FACE_OUTER_BOUND('',#5870,.T.);
#4152=FACE_OUTER_BOUND('',#5871,.T.);
#4153=FACE_OUTER_BOUND('',#5872,.T.);
#4154=FACE_OUTER_BOUND('',#5873,.T.);
#4155=FACE_OUTER_BOUND('',#5874,.T.);
#4156=FACE_OUTER_BOUND('',#5875,.T.);
#4157=FACE_OUTER_BOUND('',#5876,.T.);
#4158=FACE_OUTER_BOUND('',#5878,.T.);
#4159=FACE_OUTER_BOUND('',#5879,.T.);
#4160=FACE_OUTER_BOUND('',#5880,.T.);
#4161=FACE_OUTER_BOUND('',#5881,.T.);
#4162=FACE_OUTER_BOUND('',#5882,.T.);
#4163=FACE_OUTER_BOUND('',#5883,.T.);
#4164=FACE_OUTER_BOUND('',#5884,.T.);
#4165=FACE_OUTER_BOUND('',#5886,.T.);
#4166=FACE_OUTER_BOUND('',#5888,.T.);
#4167=FACE_OUTER_BOUND('',#5889,.T.);
#4168=FACE_OUTER_BOUND('',#5890,.T.);
#4169=FACE_OUTER_BOUND('',#5891,.T.);
#4170=FACE_OUTER_BOUND('',#5892,.T.);
#4171=FACE_OUTER_BOUND('',#5894,.T.);
#4172=FACE_OUTER_BOUND('',#5895,.T.);
#4173=FACE_OUTER_BOUND('',#5896,.T.);
#4174=FACE_OUTER_BOUND('',#5897,.T.);
#4175=FACE_OUTER_BOUND('',#5898,.T.);
#4176=FACE_OUTER_BOUND('',#5899,.T.);
#4177=FACE_OUTER_BOUND('',#5900,.T.);
#4178=FACE_OUTER_BOUND('',#5901,.T.);
#4179=FACE_OUTER_BOUND('',#5902,.T.);
#4180=FACE_OUTER_BOUND('',#5903,.T.);
#4181=FACE_OUTER_BOUND('',#5904,.T.);
#4182=FACE_OUTER_BOUND('',#5905,.T.);
#4183=EDGE_LOOP('',(#14904,#14905,#14906,#14907));
#4184=EDGE_LOOP('',(#14908,#14909,#14910,#14911));
#4185=EDGE_LOOP('',(#14912,#14913,#14914,#14915));
#4186=EDGE_LOOP('',(#14916,#14917,#14918,#14919));
#4187=EDGE_LOOP('',(#14920,#14921,#14922,#14923));
#4188=EDGE_LOOP('',(#14924,#14925,#14926,#14927));
#4189=EDGE_LOOP('',(#14928,#14929,#14930,#14931));
#4190=EDGE_LOOP('',(#14932,#14933,#14934,#14935));
#4191=EDGE_LOOP('',(#14936,#14937,#14938,#14939));
#4192=EDGE_LOOP('',(#14940,#14941,#14942,#14943));
#4193=EDGE_LOOP('',(#14944,#14945,#14946,#14947));
#4194=EDGE_LOOP('',(#14948,#14949,#14950,#14951));
#4195=EDGE_LOOP('',(#14952,#14953,#14954,#14955));
#4196=EDGE_LOOP('',(#14956,#14957,#14958,#14959));
#4197=EDGE_LOOP('',(#14960,#14961,#14962,#14963));
#4198=EDGE_LOOP('',(#14964));
#4199=EDGE_LOOP('',(#14965));
#4200=EDGE_LOOP('',(#14966));
#4201=EDGE_LOOP('',(#14967));
#4202=EDGE_LOOP('',(#14968));
#4203=EDGE_LOOP('',(#14969));
#4204=EDGE_LOOP('',(#14970));
#4205=EDGE_LOOP('',(#14971));
#4206=EDGE_LOOP('',(#14972));
#4207=EDGE_LOOP('',(#14973));
#4208=EDGE_LOOP('',(#14974,#14975,#14976,#14977));
#4209=EDGE_LOOP('',(#14978));
#4210=EDGE_LOOP('',(#14979));
#4211=EDGE_LOOP('',(#14980));
#4212=EDGE_LOOP('',(#14981));
#4213=EDGE_LOOP('',(#14982));
#4214=EDGE_LOOP('',(#14983));
#4215=EDGE_LOOP('',(#14984));
#4216=EDGE_LOOP('',(#14985));
#4217=EDGE_LOOP('',(#14986));
#4218=EDGE_LOOP('',(#14987));
#4219=EDGE_LOOP('',(#14988,#14989,#14990,#14991));
#4220=EDGE_LOOP('',(#14992,#14993,#14994,#14995));
#4221=EDGE_LOOP('',(#14996,#14997,#14998,#14999));
#4222=EDGE_LOOP('',(#15000,#15001,#15002,#15003));
#4223=EDGE_LOOP('',(#15004,#15005,#15006,#15007));
#4224=EDGE_LOOP('',(#15008,#15009,#15010,#15011));
#4225=EDGE_LOOP('',(#15012,#15013,#15014,#15015));
#4226=EDGE_LOOP('',(#15016,#15017,#15018,#15019));
#4227=EDGE_LOOP('',(#15020,#15021,#15022,#15023));
#4228=EDGE_LOOP('',(#15024,#15025,#15026,#15027));
#4229=EDGE_LOOP('',(#15028,#15029,#15030,#15031));
#4230=EDGE_LOOP('',(#15032,#15033,#15034,#15035));
#4231=EDGE_LOOP('',(#15036,#15037,#15038,#15039));
#4232=EDGE_LOOP('',(#15040,#15041,#15042,#15043));
#4233=EDGE_LOOP('',(#15044,#15045,#15046,#15047));
#4234=EDGE_LOOP('',(#15048,#15049,#15050,#15051));
#4235=EDGE_LOOP('',(#15052,#15053,#15054,#15055));
#4236=EDGE_LOOP('',(#15056,#15057,#15058,#15059));
#4237=EDGE_LOOP('',(#15060,#15061,#15062,#15063));
#4238=EDGE_LOOP('',(#15064));
#4239=EDGE_LOOP('',(#15065));
#4240=EDGE_LOOP('',(#15066,#15067,#15068,#15069));
#4241=EDGE_LOOP('',(#15070,#15071));
#4242=EDGE_LOOP('',(#15072));
#4243=EDGE_LOOP('',(#15073,#15074,#15075,#15076));
#4244=EDGE_LOOP('',(#15077));
#4245=EDGE_LOOP('',(#15078));
#4246=EDGE_LOOP('',(#15079,#15080,#15081,#15082));
#4247=EDGE_LOOP('',(#15083,#15084));
#4248=EDGE_LOOP('',(#15085));
#4249=EDGE_LOOP('',(#15086,#15087,#15088,#15089,#15090,#15091,#15092,#15093,
#15094,#15095));
#4250=EDGE_LOOP('',(#15096));
#4251=EDGE_LOOP('',(#15097));
#4252=EDGE_LOOP('',(#15098));
#4253=EDGE_LOOP('',(#15099));
#4254=EDGE_LOOP('',(#15100));
#4255=EDGE_LOOP('',(#15101));
#4256=EDGE_LOOP('',(#15102,#15103,#15104,#15105));
#4257=EDGE_LOOP('',(#15106,#15107,#15108,#15109));
#4258=EDGE_LOOP('',(#15110,#15111,#15112,#15113));
#4259=EDGE_LOOP('',(#15114,#15115,#15116,#15117));
#4260=EDGE_LOOP('',(#15118,#15119,#15120,#15121,#15122,#15123,#15124,#15125,
#15126,#15127));
#4261=EDGE_LOOP('',(#15128,#15129,#15130,#15131));
#4262=EDGE_LOOP('',(#15132,#15133,#15134,#15135));
#4263=EDGE_LOOP('',(#15136,#15137,#15138,#15139));
#4264=EDGE_LOOP('',(#15140,#15141,#15142,#15143));
#4265=EDGE_LOOP('',(#15144));
#4266=EDGE_LOOP('',(#15145));
#4267=EDGE_LOOP('',(#15146));
#4268=EDGE_LOOP('',(#15147));
#4269=EDGE_LOOP('',(#15148));
#4270=EDGE_LOOP('',(#15149));
#4271=EDGE_LOOP('',(#15150));
#4272=EDGE_LOOP('',(#15151));
#4273=EDGE_LOOP('',(#15152,#15153,#15154,#15155));
#4274=EDGE_LOOP('',(#15156,#15157,#15158,#15159));
#4275=EDGE_LOOP('',(#15160,#15161,#15162,#15163));
#4276=EDGE_LOOP('',(#15164,#15165,#15166,#15167));
#4277=EDGE_LOOP('',(#15168));
#4278=EDGE_LOOP('',(#15169));
#4279=EDGE_LOOP('',(#15170,#15171,#15172,#15173));
#4280=EDGE_LOOP('',(#15174,#15175,#15176,#15177));
#4281=EDGE_LOOP('',(#15178));
#4282=EDGE_LOOP('',(#15179,#15180,#15181,#15182));
#4283=EDGE_LOOP('',(#15183));
#4284=EDGE_LOOP('',(#15184,#15185,#15186,#15187));
#4285=EDGE_LOOP('',(#15188,#15189,#15190,#15191));
#4286=EDGE_LOOP('',(#15192));
#4287=EDGE_LOOP('',(#15193));
#4288=EDGE_LOOP('',(#15194));
#4289=EDGE_LOOP('',(#15195));
#4290=EDGE_LOOP('',(#15196,#15197,#15198,#15199));
#4291=EDGE_LOOP('',(#15200,#15201,#15202,#15203));
#4292=EDGE_LOOP('',(#15204));
#4293=EDGE_LOOP('',(#15205));
#4294=EDGE_LOOP('',(#15206));
#4295=EDGE_LOOP('',(#15207));
#4296=EDGE_LOOP('',(#15208,#15209,#15210,#15211));
#4297=EDGE_LOOP('',(#15212,#15213,#15214,#15215));
#4298=EDGE_LOOP('',(#15216));
#4299=EDGE_LOOP('',(#15217));
#4300=EDGE_LOOP('',(#15218,#15219,#15220,#15221));
#4301=EDGE_LOOP('',(#15222,#15223,#15224,#15225));
#4302=EDGE_LOOP('',(#15226,#15227,#15228,#15229));
#4303=EDGE_LOOP('',(#15230,#15231,#15232,#15233));
#4304=EDGE_LOOP('',(#15234));
#4305=EDGE_LOOP('',(#15235));
#4306=EDGE_LOOP('',(#15236,#15237,#15238,#15239));
#4307=EDGE_LOOP('',(#15240,#15241,#15242,#15243));
#4308=EDGE_LOOP('',(#15244));
#4309=EDGE_LOOP('',(#15245));
#4310=EDGE_LOOP('',(#15246));
#4311=EDGE_LOOP('',(#15247));
#4312=EDGE_LOOP('',(#15248));
#4313=EDGE_LOOP('',(#15249));
#4314=EDGE_LOOP('',(#15250));
#4315=EDGE_LOOP('',(#15251));
#4316=EDGE_LOOP('',(#15252));
#4317=EDGE_LOOP('',(#15253));
#4318=EDGE_LOOP('',(#15254,#15255,#15256,#15257));
#4319=EDGE_LOOP('',(#15258,#15259,#15260,#15261));
#4320=EDGE_LOOP('',(#15262,#15263,#15264,#15265));
#4321=EDGE_LOOP('',(#15266,#15267,#15268,#15269));
#4322=EDGE_LOOP('',(#15270));
#4323=EDGE_LOOP('',(#15271));
#4324=EDGE_LOOP('',(#15272,#15273,#15274,#15275));
#4325=EDGE_LOOP('',(#15276,#15277,#15278,#15279));
#4326=EDGE_LOOP('',(#15280));
#4327=EDGE_LOOP('',(#15281,#15282,#15283,#15284));
#4328=EDGE_LOOP('',(#15285));
#4329=EDGE_LOOP('',(#15286,#15287,#15288,#15289));
#4330=EDGE_LOOP('',(#15290,#15291,#15292,#15293));
#4331=EDGE_LOOP('',(#15294));
#4332=EDGE_LOOP('',(#15295));
#4333=EDGE_LOOP('',(#15296));
#4334=EDGE_LOOP('',(#15297));
#4335=EDGE_LOOP('',(#15298,#15299,#15300,#15301));
#4336=EDGE_LOOP('',(#15302,#15303,#15304,#15305));
#4337=EDGE_LOOP('',(#15306));
#4338=EDGE_LOOP('',(#15307));
#4339=EDGE_LOOP('',(#15308));
#4340=EDGE_LOOP('',(#15309));
#4341=EDGE_LOOP('',(#15310,#15311,#15312,#15313));
#4342=EDGE_LOOP('',(#15314,#15315,#15316,#15317));
#4343=EDGE_LOOP('',(#15318));
#4344=EDGE_LOOP('',(#15319));
#4345=EDGE_LOOP('',(#15320,#15321,#15322,#15323));
#4346=EDGE_LOOP('',(#15324,#15325,#15326,#15327));
#4347=EDGE_LOOP('',(#15328,#15329,#15330,#15331));
#4348=EDGE_LOOP('',(#15332,#15333,#15334,#15335));
#4349=EDGE_LOOP('',(#15336,#15337));
#4350=EDGE_LOOP('',(#15338));
#4351=EDGE_LOOP('',(#15339));
#4352=EDGE_LOOP('',(#15340));
#4353=EDGE_LOOP('',(#15341));
#4354=EDGE_LOOP('',(#15342,#15343,#15344,#15345));
#4355=EDGE_LOOP('',(#15346,#15347,#15348,#15349));
#4356=EDGE_LOOP('',(#15350));
#4357=EDGE_LOOP('',(#15351));
#4358=EDGE_LOOP('',(#15352,#15353,#15354,#15355));
#4359=EDGE_LOOP('',(#15356,#15357));
#4360=EDGE_LOOP('',(#15358));
#4361=EDGE_LOOP('',(#15359));
#4362=EDGE_LOOP('',(#15360));
#4363=EDGE_LOOP('',(#15361));
#4364=EDGE_LOOP('',(#15362,#15363,#15364,#15365));
#4365=EDGE_LOOP('',(#15366));
#4366=EDGE_LOOP('',(#15367));
#4367=EDGE_LOOP('',(#15368,#15369,#15370,#15371));
#4368=EDGE_LOOP('',(#15372,#15373,#15374,#15375));
#4369=EDGE_LOOP('',(#15376,#15377,#15378,#15379));
#4370=EDGE_LOOP('',(#15380,#15381,#15382,#15383));
#4371=EDGE_LOOP('',(#15384,#15385,#15386,#15387));
#4372=EDGE_LOOP('',(#15388,#15389,#15390,#15391));
#4373=EDGE_LOOP('',(#15392));
#4374=EDGE_LOOP('',(#15393,#15394,#15395,#15396));
#4375=EDGE_LOOP('',(#15397));
#4376=EDGE_LOOP('',(#15398,#15399,#15400,#15401));
#4377=EDGE_LOOP('',(#15402));
#4378=EDGE_LOOP('',(#15403));
#4379=EDGE_LOOP('',(#15404,#15405,#15406,#15407));
#4380=EDGE_LOOP('',(#15408,#15409,#15410,#15411));
#4381=EDGE_LOOP('',(#15412,#15413,#15414,#15415));
#4382=EDGE_LOOP('',(#15416,#15417,#15418,#15419));
#4383=EDGE_LOOP('',(#15420,#15421,#15422,#15423));
#4384=EDGE_LOOP('',(#15424,#15425,#15426,#15427));
#4385=EDGE_LOOP('',(#15428));
#4386=EDGE_LOOP('',(#15429,#15430,#15431,#15432));
#4387=EDGE_LOOP('',(#15433));
#4388=EDGE_LOOP('',(#15434,#15435,#15436,#15437));
#4389=EDGE_LOOP('',(#15438));
#4390=EDGE_LOOP('',(#15439));
#4391=EDGE_LOOP('',(#15440,#15441,#15442,#15443));
#4392=EDGE_LOOP('',(#15444));
#4393=EDGE_LOOP('',(#15445));
#4394=EDGE_LOOP('',(#15446,#15447,#15448,#15449));
#4395=EDGE_LOOP('',(#15450));
#4396=EDGE_LOOP('',(#15451));
#4397=EDGE_LOOP('',(#15452,#15453,#15454,#15455));
#4398=EDGE_LOOP('',(#15456));
#4399=EDGE_LOOP('',(#15457));
#4400=EDGE_LOOP('',(#15458,#15459,#15460,#15461));
#4401=EDGE_LOOP('',(#15462,#15463,#15464,#15465));
#4402=EDGE_LOOP('',(#15466,#15467,#15468,#15469));
#4403=EDGE_LOOP('',(#15470,#15471,#15472,#15473));
#4404=EDGE_LOOP('',(#15474,#15475,#15476,#15477));
#4405=EDGE_LOOP('',(#15478,#15479,#15480,#15481));
#4406=EDGE_LOOP('',(#15482,#15483,#15484,#15485));
#4407=EDGE_LOOP('',(#15486,#15487,#15488,#15489));
#4408=EDGE_LOOP('',(#15490,#15491,#15492,#15493));
#4409=EDGE_LOOP('',(#15494));
#4410=EDGE_LOOP('',(#15495));
#4411=EDGE_LOOP('',(#15496));
#4412=EDGE_LOOP('',(#15497));
#4413=EDGE_LOOP('',(#15498,#15499,#15500,#15501));
#4414=EDGE_LOOP('',(#15502,#15503,#15504,#15505));
#4415=EDGE_LOOP('',(#15506,#15507,#15508,#15509));
#4416=EDGE_LOOP('',(#15510,#15511,#15512,#15513));
#4417=EDGE_LOOP('',(#15514,#15515,#15516,#15517));
#4418=EDGE_LOOP('',(#15518,#15519,#15520,#15521));
#4419=EDGE_LOOP('',(#15522));
#4420=EDGE_LOOP('',(#15523));
#4421=EDGE_LOOP('',(#15524));
#4422=EDGE_LOOP('',(#15525));
#4423=EDGE_LOOP('',(#15526,#15527,#15528,#15529));
#4424=EDGE_LOOP('',(#15530,#15531,#15532,#15533,#15534,#15535,#15536,#15537,
#15538,#15539,#15540,#15541));
#4425=EDGE_LOOP('',(#15542,#15543,#15544,#15545,#15546,#15547,#15548,#15549,
#15550,#15551,#15552,#15553));
#4426=EDGE_LOOP('',(#15554,#15555,#15556,#15557,#15558,#15559));
#4427=EDGE_LOOP('',(#15560,#15561,#15562,#15563,#15564));
#4428=EDGE_LOOP('',(#15565,#15566,#15567,#15568));
#4429=EDGE_LOOP('',(#15569,#15570,#15571,#15572));
#4430=EDGE_LOOP('',(#15573));
#4431=EDGE_LOOP('',(#15574));
#4432=EDGE_LOOP('',(#15575,#15576,#15577,#15578,#15579));
#4433=EDGE_LOOP('',(#15580));
#4434=EDGE_LOOP('',(#15581));
#4435=EDGE_LOOP('',(#15582,#15583,#15584,#15585));
#4436=EDGE_LOOP('',(#15586,#15587,#15588,#15589,#15590,#15591));
#4437=EDGE_LOOP('',(#15592,#15593,#15594,#15595,#15596));
#4438=EDGE_LOOP('',(#15597));
#4439=EDGE_LOOP('',(#15598));
#4440=EDGE_LOOP('',(#15599,#15600,#15601,#15602));
#4441=EDGE_LOOP('',(#15603,#15604,#15605,#15606));
#4442=EDGE_LOOP('',(#15607,#15608,#15609,#15610));
#4443=EDGE_LOOP('',(#15611));
#4444=EDGE_LOOP('',(#15612));
#4445=EDGE_LOOP('',(#15613,#15614,#15615,#15616,#15617));
#4446=EDGE_LOOP('',(#15618,#15619));
#4447=EDGE_LOOP('',(#15620,#15621));
#4448=EDGE_LOOP('',(#15622,#15623));
#4449=EDGE_LOOP('',(#15624,#15625));
#4450=EDGE_LOOP('',(#15626,#15627));
#4451=EDGE_LOOP('',(#15628,#15629));
#4452=EDGE_LOOP('',(#15630,#15631));
#4453=EDGE_LOOP('',(#15632,#15633,#15634,#15635));
#4454=EDGE_LOOP('',(#15636,#15637,#15638,#15639,#15640,#15641,#15642,#15643,
#15644,#15645,#15646,#15647,#15648,#15649,#15650,#15651,#15652,#15653));
#4455=EDGE_LOOP('',(#15654,#15655,#15656,#15657));
#4456=EDGE_LOOP('',(#15658,#15659,#15660,#15661));
#4457=EDGE_LOOP('',(#15662,#15663,#15664,#15665));
#4458=EDGE_LOOP('',(#15666,#15667,#15668,#15669));
#4459=EDGE_LOOP('',(#15670,#15671,#15672,#15673,#15674,#15675));
#4460=EDGE_LOOP('',(#15676,#15677,#15678,#15679));
#4461=EDGE_LOOP('',(#15680,#15681,#15682,#15683));
#4462=EDGE_LOOP('',(#15684,#15685,#15686,#15687));
#4463=EDGE_LOOP('',(#15688,#15689,#15690,#15691));
#4464=EDGE_LOOP('',(#15692,#15693,#15694,#15695));
#4465=EDGE_LOOP('',(#15696,#15697,#15698,#15699,#15700,#15701,#15702,#15703,
#15704,#15705,#15706,#15707,#15708,#15709,#15710,#15711,#15712,#15713));
#4466=EDGE_LOOP('',(#15714,#15715,#15716,#15717));
#4467=EDGE_LOOP('',(#15718,#15719,#15720,#15721));
#4468=EDGE_LOOP('',(#15722));
#4469=EDGE_LOOP('',(#15723));
#4470=EDGE_LOOP('',(#15724,#15725,#15726,#15727));
#4471=EDGE_LOOP('',(#15728));
#4472=EDGE_LOOP('',(#15729));
#4473=EDGE_LOOP('',(#15730,#15731,#15732,#15733));
#4474=EDGE_LOOP('',(#15734));
#4475=EDGE_LOOP('',(#15735));
#4476=EDGE_LOOP('',(#15736,#15737,#15738,#15739));
#4477=EDGE_LOOP('',(#15740));
#4478=EDGE_LOOP('',(#15741));
#4479=EDGE_LOOP('',(#15742,#15743,#15744,#15745));
#4480=EDGE_LOOP('',(#15746));
#4481=EDGE_LOOP('',(#15747));
#4482=EDGE_LOOP('',(#15748,#15749,#15750,#15751));
#4483=EDGE_LOOP('',(#15752,#15753,#15754,#15755,#15756,#15757));
#4484=EDGE_LOOP('',(#15758,#15759,#15760,#15761,#15762));
#4485=EDGE_LOOP('',(#15763,#15764,#15765,#15766));
#4486=EDGE_LOOP('',(#15767,#15768,#15769,#15770));
#4487=EDGE_LOOP('',(#15771));
#4488=EDGE_LOOP('',(#15772));
#4489=EDGE_LOOP('',(#15773,#15774,#15775,#15776,#15777));
#4490=EDGE_LOOP('',(#15778));
#4491=EDGE_LOOP('',(#15779));
#4492=EDGE_LOOP('',(#15780,#15781,#15782,#15783));
#4493=EDGE_LOOP('',(#15784,#15785,#15786,#15787,#15788,#15789));
#4494=EDGE_LOOP('',(#15790,#15791,#15792,#15793,#15794));
#4495=EDGE_LOOP('',(#15795));
#4496=EDGE_LOOP('',(#15796));
#4497=EDGE_LOOP('',(#15797,#15798,#15799,#15800));
#4498=EDGE_LOOP('',(#15801,#15802,#15803,#15804));
#4499=EDGE_LOOP('',(#15805,#15806,#15807,#15808));
#4500=EDGE_LOOP('',(#15809));
#4501=EDGE_LOOP('',(#15810));
#4502=EDGE_LOOP('',(#15811,#15812,#15813,#15814,#15815));
#4503=EDGE_LOOP('',(#15816,#15817));
#4504=EDGE_LOOP('',(#15818,#15819));
#4505=EDGE_LOOP('',(#15820,#15821));
#4506=EDGE_LOOP('',(#15822,#15823));
#4507=EDGE_LOOP('',(#15824,#15825));
#4508=EDGE_LOOP('',(#15826,#15827));
#4509=EDGE_LOOP('',(#15828,#15829));
#4510=EDGE_LOOP('',(#15830,#15831));
#4511=EDGE_LOOP('',(#15832,#15833,#15834,#15835));
#4512=EDGE_LOOP('',(#15836,#15837,#15838,#15839,#15840,#15841,#15842,#15843,
#15844,#15845,#15846,#15847,#15848,#15849,#15850,#15851,#15852,#15853,#15854,
#15855));
#4513=EDGE_LOOP('',(#15856,#15857,#15858,#15859));
#4514=EDGE_LOOP('',(#15860,#15861,#15862,#15863));
#4515=EDGE_LOOP('',(#15864,#15865,#15866,#15867));
#4516=EDGE_LOOP('',(#15868,#15869,#15870,#15871));
#4517=EDGE_LOOP('',(#15872,#15873,#15874,#15875));
#4518=EDGE_LOOP('',(#15876,#15877,#15878,#15879,#15880,#15881));
#4519=EDGE_LOOP('',(#15882,#15883,#15884,#15885));
#4520=EDGE_LOOP('',(#15886,#15887,#15888,#15889));
#4521=EDGE_LOOP('',(#15890,#15891,#15892,#15893));
#4522=EDGE_LOOP('',(#15894,#15895,#15896,#15897));
#4523=EDGE_LOOP('',(#15898,#15899,#15900,#15901));
#4524=EDGE_LOOP('',(#15902,#15903,#15904,#15905));
#4525=EDGE_LOOP('',(#15906,#15907,#15908,#15909,#15910,#15911,#15912,#15913,
#15914,#15915,#15916,#15917,#15918,#15919,#15920,#15921,#15922,#15923,#15924,
#15925));
#4526=EDGE_LOOP('',(#15926,#15927,#15928,#15929));
#4527=EDGE_LOOP('',(#15930,#15931,#15932,#15933));
#4528=EDGE_LOOP('',(#15934));
#4529=EDGE_LOOP('',(#15935));
#4530=EDGE_LOOP('',(#15936,#15937,#15938,#15939));
#4531=EDGE_LOOP('',(#15940));
#4532=EDGE_LOOP('',(#15941));
#4533=EDGE_LOOP('',(#15942,#15943,#15944,#15945));
#4534=EDGE_LOOP('',(#15946));
#4535=EDGE_LOOP('',(#15947));
#4536=EDGE_LOOP('',(#15948,#15949,#15950,#15951));
#4537=EDGE_LOOP('',(#15952));
#4538=EDGE_LOOP('',(#15953));
#4539=EDGE_LOOP('',(#15954,#15955,#15956,#15957));
#4540=EDGE_LOOP('',(#15958));
#4541=EDGE_LOOP('',(#15959));
#4542=EDGE_LOOP('',(#15960,#15961,#15962,#15963));
#4543=EDGE_LOOP('',(#15964,#15965,#15966,#15967));
#4544=EDGE_LOOP('',(#15968,#15969,#15970,#15971));
#4545=EDGE_LOOP('',(#15972,#15973,#15974,#15975));
#4546=EDGE_LOOP('',(#15976,#15977,#15978,#15979));
#4547=EDGE_LOOP('',(#15980,#15981,#15982,#15983));
#4548=EDGE_LOOP('',(#15984,#15985,#15986,#15987));
#4549=EDGE_LOOP('',(#15988,#15989,#15990,#15991));
#4550=EDGE_LOOP('',(#15992,#15993,#15994,#15995));
#4551=EDGE_LOOP('',(#15996,#15997,#15998,#15999));
#4552=EDGE_LOOP('',(#16000));
#4553=EDGE_LOOP('',(#16001));
#4554=EDGE_LOOP('',(#16002));
#4555=EDGE_LOOP('',(#16003));
#4556=EDGE_LOOP('',(#16004,#16005,#16006,#16007));
#4557=EDGE_LOOP('',(#16008));
#4558=EDGE_LOOP('',(#16009));
#4559=EDGE_LOOP('',(#16010));
#4560=EDGE_LOOP('',(#16011));
#4561=EDGE_LOOP('',(#16012,#16013,#16014,#16015));
#4562=EDGE_LOOP('',(#16016,#16017,#16018,#16019));
#4563=EDGE_LOOP('',(#16020,#16021,#16022,#16023));
#4564=EDGE_LOOP('',(#16024,#16025,#16026,#16027));
#4565=EDGE_LOOP('',(#16028,#16029,#16030,#16031));
#4566=EDGE_LOOP('',(#16032,#16033,#16034,#16035));
#4567=EDGE_LOOP('',(#16036,#16037,#16038,#16039));
#4568=EDGE_LOOP('',(#16040,#16041,#16042,#16043));
#4569=EDGE_LOOP('',(#16044,#16045,#16046,#16047));
#4570=EDGE_LOOP('',(#16048,#16049,#16050,#16051));
#4571=EDGE_LOOP('',(#16052,#16053,#16054,#16055));
#4572=EDGE_LOOP('',(#16056,#16057,#16058,#16059));
#4573=EDGE_LOOP('',(#16060,#16061,#16062,#16063));
#4574=EDGE_LOOP('',(#16064,#16065,#16066,#16067));
#4575=EDGE_LOOP('',(#16068,#16069,#16070,#16071));
#4576=EDGE_LOOP('',(#16072,#16073,#16074,#16075));
#4577=EDGE_LOOP('',(#16076,#16077,#16078,#16079));
#4578=EDGE_LOOP('',(#16080));
#4579=EDGE_LOOP('',(#16081));
#4580=EDGE_LOOP('',(#16082));
#4581=EDGE_LOOP('',(#16083));
#4582=EDGE_LOOP('',(#16084));
#4583=EDGE_LOOP('',(#16085));
#4584=EDGE_LOOP('',(#16086));
#4585=EDGE_LOOP('',(#16087));
#4586=EDGE_LOOP('',(#16088));
#4587=EDGE_LOOP('',(#16089));
#4588=EDGE_LOOP('',(#16090));
#4589=EDGE_LOOP('',(#16091));
#4590=EDGE_LOOP('',(#16092,#16093,#16094,#16095));
#4591=EDGE_LOOP('',(#16096));
#4592=EDGE_LOOP('',(#16097));
#4593=EDGE_LOOP('',(#16098));
#4594=EDGE_LOOP('',(#16099));
#4595=EDGE_LOOP('',(#16100));
#4596=EDGE_LOOP('',(#16101));
#4597=EDGE_LOOP('',(#16102));
#4598=EDGE_LOOP('',(#16103));
#4599=EDGE_LOOP('',(#16104));
#4600=EDGE_LOOP('',(#16105));
#4601=EDGE_LOOP('',(#16106));
#4602=EDGE_LOOP('',(#16107));
#4603=EDGE_LOOP('',(#16108,#16109,#16110,#16111));
#4604=EDGE_LOOP('',(#16112));
#4605=EDGE_LOOP('',(#16113,#16114,#16115,#16116));
#4606=EDGE_LOOP('',(#16117));
#4607=EDGE_LOOP('',(#16118,#16119,#16120,#16121));
#4608=EDGE_LOOP('',(#16122));
#4609=EDGE_LOOP('',(#16123,#16124,#16125,#16126));
#4610=EDGE_LOOP('',(#16127));
#4611=EDGE_LOOP('',(#16128,#16129,#16130,#16131));
#4612=EDGE_LOOP('',(#16132));
#4613=EDGE_LOOP('',(#16133,#16134,#16135,#16136));
#4614=EDGE_LOOP('',(#16137));
#4615=EDGE_LOOP('',(#16138,#16139,#16140,#16141));
#4616=EDGE_LOOP('',(#16142));
#4617=EDGE_LOOP('',(#16143,#16144,#16145,#16146));
#4618=EDGE_LOOP('',(#16147,#16148,#16149,#16150));
#4619=EDGE_LOOP('',(#16151,#16152,#16153,#16154));
#4620=EDGE_LOOP('',(#16155));
#4621=EDGE_LOOP('',(#16156));
#4622=EDGE_LOOP('',(#16157));
#4623=EDGE_LOOP('',(#16158));
#4624=EDGE_LOOP('',(#16159,#16160,#16161,#16162));
#4625=EDGE_LOOP('',(#16163,#16164,#16165,#16166));
#4626=EDGE_LOOP('',(#16167));
#4627=EDGE_LOOP('',(#16168,#16169,#16170,#16171));
#4628=EDGE_LOOP('',(#16172));
#4629=EDGE_LOOP('',(#16173));
#4630=EDGE_LOOP('',(#16174));
#4631=EDGE_LOOP('',(#16175));
#4632=EDGE_LOOP('',(#16176,#16177,#16178,#16179));
#4633=EDGE_LOOP('',(#16180,#16181));
#4634=EDGE_LOOP('',(#16182,#16183,#16184,#16185,#16186,#16187,#16188,#16189));
#4635=EDGE_LOOP('',(#16190,#16191));
#4636=EDGE_LOOP('',(#16192,#16193,#16194,#16195,#16196,#16197,#16198,#16199));
#4637=EDGE_LOOP('',(#16200,#16201));
#4638=EDGE_LOOP('',(#16202,#16203,#16204,#16205,#16206,#16207,#16208,#16209));
#4639=EDGE_LOOP('',(#16210,#16211));
#4640=EDGE_LOOP('',(#16212,#16213,#16214,#16215,#16216,#16217,#16218,#16219));
#4641=EDGE_LOOP('',(#16220,#16221,#16222,#16223,#16224,#16225,#16226,#16227,
#16228,#16229,#16230,#16231));
#4642=EDGE_LOOP('',(#16232,#16233,#16234,#16235,#16236,#16237,#16238,#16239,
#16240,#16241,#16242,#16243));
#4643=EDGE_LOOP('',(#16244,#16245,#16246,#16247,#16248,#16249,#16250,#16251,
#16252,#16253,#16254,#16255));
#4644=EDGE_LOOP('',(#16256,#16257,#16258,#16259,#16260,#16261,#16262,#16263,
#16264,#16265));
#4645=EDGE_LOOP('',(#16266,#16267,#16268,#16269));
#4646=EDGE_LOOP('',(#16270,#16271,#16272,#16273));
#4647=EDGE_LOOP('',(#16274));
#4648=EDGE_LOOP('',(#16275));
#4649=EDGE_LOOP('',(#16276));
#4650=EDGE_LOOP('',(#16277));
#4651=EDGE_LOOP('',(#16278,#16279,#16280,#16281));
#4652=EDGE_LOOP('',(#16282,#16283,#16284,#16285,#16286,#16287,#16288,#16289,
#16290,#16291));
#4653=EDGE_LOOP('',(#16292,#16293,#16294,#16295));
#4654=EDGE_LOOP('',(#16296,#16297,#16298,#16299));
#4655=EDGE_LOOP('',(#16300,#16301,#16302,#16303));
#4656=EDGE_LOOP('',(#16304,#16305,#16306,#16307));
#4657=EDGE_LOOP('',(#16308,#16309,#16310,#16311));
#4658=EDGE_LOOP('',(#16312,#16313,#16314,#16315,#16316,#16317,#16318,#16319,
#16320,#16321,#16322,#16323));
#4659=EDGE_LOOP('',(#16324,#16325,#16326,#16327));
#4660=EDGE_LOOP('',(#16328,#16329,#16330,#16331));
#4661=EDGE_LOOP('',(#16332,#16333,#16334,#16335));
#4662=EDGE_LOOP('',(#16336,#16337,#16338,#16339));
#4663=EDGE_LOOP('',(#16340,#16341,#16342,#16343));
#4664=EDGE_LOOP('',(#16344,#16345,#16346,#16347));
#4665=EDGE_LOOP('',(#16348,#16349,#16350,#16351));
#4666=EDGE_LOOP('',(#16352,#16353,#16354,#16355));
#4667=EDGE_LOOP('',(#16356,#16357,#16358,#16359,#16360,#16361,#16362,#16363));
#4668=EDGE_LOOP('',(#16364,#16365,#16366,#16367,#16368,#16369,#16370,#16371));
#4669=EDGE_LOOP('',(#16372,#16373,#16374,#16375));
#4670=EDGE_LOOP('',(#16376,#16377,#16378,#16379));
#4671=EDGE_LOOP('',(#16380,#16381,#16382,#16383));
#4672=EDGE_LOOP('',(#16384,#16385,#16386,#16387));
#4673=EDGE_LOOP('',(#16388,#16389,#16390,#16391));
#4674=EDGE_LOOP('',(#16392,#16393,#16394,#16395));
#4675=EDGE_LOOP('',(#16396,#16397,#16398,#16399));
#4676=EDGE_LOOP('',(#16400,#16401,#16402,#16403));
#4677=EDGE_LOOP('',(#16404,#16405,#16406,#16407,#16408,#16409,#16410,#16411));
#4678=EDGE_LOOP('',(#16412,#16413,#16414,#16415,#16416,#16417,#16418,#16419));
#4679=EDGE_LOOP('',(#16420,#16421,#16422,#16423));
#4680=EDGE_LOOP('',(#16424,#16425,#16426,#16427));
#4681=EDGE_LOOP('',(#16428));
#4682=EDGE_LOOP('',(#16429));
#4683=EDGE_LOOP('',(#16430,#16431,#16432,#16433));
#4684=EDGE_LOOP('',(#16434));
#4685=EDGE_LOOP('',(#16435));
#4686=EDGE_LOOP('',(#16436,#16437,#16438,#16439));
#4687=EDGE_LOOP('',(#16440,#16441,#16442,#16443));
#4688=EDGE_LOOP('',(#16444,#16445,#16446,#16447));
#4689=EDGE_LOOP('',(#16448,#16449,#16450,#16451));
#4690=EDGE_LOOP('',(#16452,#16453,#16454,#16455));
#4691=EDGE_LOOP('',(#16456,#16457,#16458,#16459));
#4692=EDGE_LOOP('',(#16460,#16461,#16462,#16463,#16464,#16465));
#4693=EDGE_LOOP('',(#16466,#16467,#16468,#16469,#16470,#16471));
#4694=EDGE_LOOP('',(#16472));
#4695=EDGE_LOOP('',(#16473));
#4696=EDGE_LOOP('',(#16474,#16475,#16476,#16477));
#4697=EDGE_LOOP('',(#16478));
#4698=EDGE_LOOP('',(#16479));
#4699=EDGE_LOOP('',(#16480,#16481,#16482,#16483));
#4700=EDGE_LOOP('',(#16484,#16485,#16486,#16487));
#4701=EDGE_LOOP('',(#16488,#16489,#16490,#16491));
#4702=EDGE_LOOP('',(#16492));
#4703=EDGE_LOOP('',(#16493));
#4704=EDGE_LOOP('',(#16494,#16495,#16496,#16497));
#4705=EDGE_LOOP('',(#16498,#16499,#16500,#16501));
#4706=EDGE_LOOP('',(#16502,#16503,#16504,#16505));
#4707=EDGE_LOOP('',(#16506,#16507,#16508,#16509));
#4708=EDGE_LOOP('',(#16510,#16511,#16512,#16513));
#4709=EDGE_LOOP('',(#16514,#16515,#16516,#16517));
#4710=EDGE_LOOP('',(#16518,#16519,#16520,#16521));
#4711=EDGE_LOOP('',(#16522,#16523,#16524,#16525));
#4712=EDGE_LOOP('',(#16526,#16527,#16528,#16529));
#4713=EDGE_LOOP('',(#16530,#16531,#16532,#16533));
#4714=EDGE_LOOP('',(#16534,#16535,#16536));
#4715=EDGE_LOOP('',(#16537,#16538,#16539,#16540));
#4716=EDGE_LOOP('',(#16541,#16542,#16543,#16544));
#4717=EDGE_LOOP('',(#16545,#16546,#16547,#16548));
#4718=EDGE_LOOP('',(#16549,#16550,#16551,#16552));
#4719=EDGE_LOOP('',(#16553,#16554,#16555,#16556));
#4720=EDGE_LOOP('',(#16557,#16558,#16559,#16560));
#4721=EDGE_LOOP('',(#16561,#16562,#16563,#16564));
#4722=EDGE_LOOP('',(#16565,#16566,#16567,#16568));
#4723=EDGE_LOOP('',(#16569,#16570,#16571,#16572));
#4724=EDGE_LOOP('',(#16573,#16574,#16575,#16576));
#4725=EDGE_LOOP('',(#16577,#16578,#16579,#16580,#16581,#16582,#16583,#16584,
#16585,#16586,#16587,#16588,#16589,#16590,#16591,#16592,#16593,#16594,#16595,
#16596,#16597,#16598));
#4726=EDGE_LOOP('',(#16599,#16600,#16601,#16602,#16603,#16604,#16605,#16606,
#16607,#16608,#16609,#16610,#16611,#16612,#16613,#16614,#16615,#16616,#16617,
#16618,#16619));
#4727=EDGE_LOOP('',(#16620,#16621));
#4728=EDGE_LOOP('',(#16622,#16623,#16624,#16625,#16626));
#4729=EDGE_LOOP('',(#16627));
#4730=EDGE_LOOP('',(#16628));
#4731=EDGE_LOOP('',(#16629));
#4732=EDGE_LOOP('',(#16630,#16631,#16632,#16633));
#4733=EDGE_LOOP('',(#16634,#16635,#16636,#16637));
#4734=EDGE_LOOP('',(#16638,#16639,#16640,#16641));
#4735=EDGE_LOOP('',(#16642,#16643,#16644,#16645));
#4736=EDGE_LOOP('',(#16646,#16647));
#4737=EDGE_LOOP('',(#16648));
#4738=EDGE_LOOP('',(#16649));
#4739=EDGE_LOOP('',(#16650));
#4740=EDGE_LOOP('',(#16651));
#4741=EDGE_LOOP('',(#16652,#16653,#16654,#16655));
#4742=EDGE_LOOP('',(#16656,#16657,#16658,#16659,#16660));
#4743=EDGE_LOOP('',(#16661,#16662,#16663,#16664));
#4744=EDGE_LOOP('',(#16665));
#4745=EDGE_LOOP('',(#16666,#16667,#16668,#16669));
#4746=EDGE_LOOP('',(#16670));
#4747=EDGE_LOOP('',(#16671,#16672,#16673,#16674));
#4748=EDGE_LOOP('',(#16675,#16676,#16677,#16678));
#4749=EDGE_LOOP('',(#16679,#16680,#16681,#16682));
#4750=EDGE_LOOP('',(#16683));
#4751=EDGE_LOOP('',(#16684));
#4752=EDGE_LOOP('',(#16685,#16686,#16687,#16688));
#4753=EDGE_LOOP('',(#16689,#16690,#16691,#16692));
#4754=EDGE_LOOP('',(#16693,#16694,#16695,#16696));
#4755=EDGE_LOOP('',(#16697));
#4756=EDGE_LOOP('',(#16698,#16699,#16700,#16701));
#4757=EDGE_LOOP('',(#16702,#16703,#16704,#16705));
#4758=EDGE_LOOP('',(#16706,#16707,#16708,#16709));
#4759=EDGE_LOOP('',(#16710,#16711,#16712,#16713));
#4760=EDGE_LOOP('',(#16714,#16715,#16716,#16717));
#4761=EDGE_LOOP('',(#16718,#16719,#16720,#16721));
#4762=EDGE_LOOP('',(#16722,#16723,#16724,#16725,#16726,#16727));
#4763=EDGE_LOOP('',(#16728,#16729,#16730,#16731,#16732,#16733));
#4764=EDGE_LOOP('',(#16734));
#4765=EDGE_LOOP('',(#16735,#16736,#16737,#16738));
#4766=EDGE_LOOP('',(#16739,#16740,#16741,#16742));
#4767=EDGE_LOOP('',(#16743,#16744,#16745,#16746));
#4768=EDGE_LOOP('',(#16747));
#4769=EDGE_LOOP('',(#16748));
#4770=EDGE_LOOP('',(#16749,#16750,#16751,#16752));
#4771=EDGE_LOOP('',(#16753,#16754,#16755,#16756));
#4772=EDGE_LOOP('',(#16757,#16758,#16759,#16760));
#4773=EDGE_LOOP('',(#16761));
#4774=EDGE_LOOP('',(#16762,#16763,#16764,#16765));
#4775=EDGE_LOOP('',(#16766,#16767,#16768,#16769));
#4776=EDGE_LOOP('',(#16770,#16771,#16772,#16773));
#4777=EDGE_LOOP('',(#16774,#16775,#16776,#16777));
#4778=EDGE_LOOP('',(#16778,#16779,#16780,#16781));
#4779=EDGE_LOOP('',(#16782,#16783,#16784,#16785));
#4780=EDGE_LOOP('',(#16786,#16787,#16788,#16789,#16790,#16791));
#4781=EDGE_LOOP('',(#16792,#16793,#16794,#16795,#16796,#16797));
#4782=EDGE_LOOP('',(#16798,#16799,#16800,#16801));
#4783=EDGE_LOOP('',(#16802,#16803,#16804,#16805));
#4784=EDGE_LOOP('',(#16806,#16807,#16808,#16809));
#4785=EDGE_LOOP('',(#16810,#16811,#16812,#16813));
#4786=EDGE_LOOP('',(#16814,#16815,#16816,#16817));
#4787=EDGE_LOOP('',(#16818,#16819,#16820,#16821));
#4788=EDGE_LOOP('',(#16822,#16823,#16824,#16825));
#4789=EDGE_LOOP('',(#16826,#16827,#16828,#16829));
#4790=EDGE_LOOP('',(#16830,#16831,#16832,#16833));
#4791=EDGE_LOOP('',(#16834,#16835,#16836,#16837));
#4792=EDGE_LOOP('',(#16838,#16839,#16840,#16841));
#4793=EDGE_LOOP('',(#16842,#16843,#16844,#16845));
#4794=EDGE_LOOP('',(#16846,#16847,#16848,#16849));
#4795=EDGE_LOOP('',(#16850,#16851,#16852,#16853));
#4796=EDGE_LOOP('',(#16854,#16855,#16856,#16857));
#4797=EDGE_LOOP('',(#16858,#16859,#16860,#16861));
#4798=EDGE_LOOP('',(#16862,#16863,#16864,#16865));
#4799=EDGE_LOOP('',(#16866,#16867,#16868,#16869));
#4800=EDGE_LOOP('',(#16870,#16871,#16872,#16873));
#4801=EDGE_LOOP('',(#16874,#16875,#16876,#16877));
#4802=EDGE_LOOP('',(#16878,#16879,#16880,#16881));
#4803=EDGE_LOOP('',(#16882,#16883,#16884,#16885));
#4804=EDGE_LOOP('',(#16886,#16887,#16888,#16889));
#4805=EDGE_LOOP('',(#16890,#16891,#16892,#16893));
#4806=EDGE_LOOP('',(#16894,#16895,#16896,#16897));
#4807=EDGE_LOOP('',(#16898,#16899,#16900,#16901));
#4808=EDGE_LOOP('',(#16902,#16903,#16904,#16905));
#4809=EDGE_LOOP('',(#16906,#16907,#16908,#16909));
#4810=EDGE_LOOP('',(#16910,#16911,#16912,#16913));
#4811=EDGE_LOOP('',(#16914,#16915,#16916,#16917));
#4812=EDGE_LOOP('',(#16918,#16919,#16920,#16921));
#4813=EDGE_LOOP('',(#16922,#16923,#16924,#16925));
#4814=EDGE_LOOP('',(#16926,#16927,#16928,#16929));
#4815=EDGE_LOOP('',(#16930,#16931,#16932,#16933));
#4816=EDGE_LOOP('',(#16934,#16935,#16936,#16937));
#4817=EDGE_LOOP('',(#16938,#16939,#16940,#16941));
#4818=EDGE_LOOP('',(#16942,#16943,#16944,#16945));
#4819=EDGE_LOOP('',(#16946,#16947,#16948,#16949));
#4820=EDGE_LOOP('',(#16950,#16951,#16952,#16953));
#4821=EDGE_LOOP('',(#16954,#16955,#16956,#16957));
#4822=EDGE_LOOP('',(#16958,#16959,#16960,#16961));
#4823=EDGE_LOOP('',(#16962,#16963,#16964,#16965));
#4824=EDGE_LOOP('',(#16966,#16967,#16968,#16969));
#4825=EDGE_LOOP('',(#16970,#16971,#16972,#16973));
#4826=EDGE_LOOP('',(#16974,#16975,#16976,#16977));
#4827=EDGE_LOOP('',(#16978,#16979,#16980,#16981));
#4828=EDGE_LOOP('',(#16982,#16983,#16984,#16985));
#4829=EDGE_LOOP('',(#16986,#16987,#16988,#16989));
#4830=EDGE_LOOP('',(#16990,#16991,#16992,#16993));
#4831=EDGE_LOOP('',(#16994,#16995,#16996,#16997));
#4832=EDGE_LOOP('',(#16998,#16999,#17000,#17001));
#4833=EDGE_LOOP('',(#17002,#17003,#17004,#17005));
#4834=EDGE_LOOP('',(#17006,#17007,#17008,#17009));
#4835=EDGE_LOOP('',(#17010,#17011,#17012,#17013));
#4836=EDGE_LOOP('',(#17014,#17015,#17016,#17017));
#4837=EDGE_LOOP('',(#17018,#17019,#17020,#17021));
#4838=EDGE_LOOP('',(#17022,#17023,#17024,#17025));
#4839=EDGE_LOOP('',(#17026,#17027,#17028,#17029));
#4840=EDGE_LOOP('',(#17030,#17031,#17032,#17033));
#4841=EDGE_LOOP('',(#17034,#17035,#17036,#17037));
#4842=EDGE_LOOP('',(#17038,#17039,#17040,#17041));
#4843=EDGE_LOOP('',(#17042,#17043,#17044,#17045));
#4844=EDGE_LOOP('',(#17046,#17047,#17048,#17049));
#4845=EDGE_LOOP('',(#17050,#17051,#17052));
#4846=EDGE_LOOP('',(#17053,#17054,#17055,#17056,#17057));
#4847=EDGE_LOOP('',(#17058,#17059,#17060,#17061));
#4848=EDGE_LOOP('',(#17062,#17063,#17064,#17065));
#4849=EDGE_LOOP('',(#17066,#17067,#17068,#17069));
#4850=EDGE_LOOP('',(#17070,#17071,#17072,#17073));
#4851=EDGE_LOOP('',(#17074,#17075,#17076,#17077));
#4852=EDGE_LOOP('',(#17078,#17079,#17080,#17081));
#4853=EDGE_LOOP('',(#17082,#17083,#17084,#17085));
#4854=EDGE_LOOP('',(#17086,#17087,#17088,#17089));
#4855=EDGE_LOOP('',(#17090,#17091,#17092,#17093));
#4856=EDGE_LOOP('',(#17094,#17095,#17096,#17097));
#4857=EDGE_LOOP('',(#17098,#17099,#17100,#17101));
#4858=EDGE_LOOP('',(#17102,#17103,#17104,#17105));
#4859=EDGE_LOOP('',(#17106,#17107,#17108,#17109));
#4860=EDGE_LOOP('',(#17110,#17111,#17112,#17113));
#4861=EDGE_LOOP('',(#17114,#17115,#17116,#17117));
#4862=EDGE_LOOP('',(#17118,#17119,#17120,#17121));
#4863=EDGE_LOOP('',(#17122,#17123,#17124,#17125));
#4864=EDGE_LOOP('',(#17126,#17127,#17128,#17129));
#4865=EDGE_LOOP('',(#17130,#17131,#17132,#17133));
#4866=EDGE_LOOP('',(#17134,#17135,#17136,#17137));
#4867=EDGE_LOOP('',(#17138,#17139,#17140,#17141));
#4868=EDGE_LOOP('',(#17142,#17143,#17144,#17145));
#4869=EDGE_LOOP('',(#17146,#17147,#17148,#17149));
#4870=EDGE_LOOP('',(#17150,#17151,#17152,#17153));
#4871=EDGE_LOOP('',(#17154,#17155,#17156,#17157));
#4872=EDGE_LOOP('',(#17158,#17159,#17160,#17161));
#4873=EDGE_LOOP('',(#17162,#17163,#17164,#17165));
#4874=EDGE_LOOP('',(#17166,#17167,#17168,#17169));
#4875=EDGE_LOOP('',(#17170,#17171,#17172,#17173));
#4876=EDGE_LOOP('',(#17174,#17175,#17176,#17177));
#4877=EDGE_LOOP('',(#17178,#17179,#17180,#17181));
#4878=EDGE_LOOP('',(#17182,#17183,#17184,#17185));
#4879=EDGE_LOOP('',(#17186,#17187,#17188,#17189));
#4880=EDGE_LOOP('',(#17190,#17191,#17192,#17193));
#4881=EDGE_LOOP('',(#17194,#17195,#17196,#17197));
#4882=EDGE_LOOP('',(#17198,#17199,#17200,#17201));
#4883=EDGE_LOOP('',(#17202,#17203,#17204,#17205));
#4884=EDGE_LOOP('',(#17206,#17207,#17208,#17209));
#4885=EDGE_LOOP('',(#17210,#17211,#17212,#17213));
#4886=EDGE_LOOP('',(#17214,#17215,#17216,#17217));
#4887=EDGE_LOOP('',(#17218,#17219,#17220,#17221));
#4888=EDGE_LOOP('',(#17222,#17223,#17224,#17225));
#4889=EDGE_LOOP('',(#17226,#17227,#17228,#17229));
#4890=EDGE_LOOP('',(#17230,#17231,#17232,#17233));
#4891=EDGE_LOOP('',(#17234,#17235,#17236,#17237));
#4892=EDGE_LOOP('',(#17238,#17239,#17240,#17241));
#4893=EDGE_LOOP('',(#17242,#17243,#17244,#17245));
#4894=EDGE_LOOP('',(#17246,#17247,#17248,#17249));
#4895=EDGE_LOOP('',(#17250,#17251,#17252,#17253));
#4896=EDGE_LOOP('',(#17254,#17255,#17256,#17257));
#4897=EDGE_LOOP('',(#17258,#17259,#17260,#17261));
#4898=EDGE_LOOP('',(#17262,#17263,#17264,#17265));
#4899=EDGE_LOOP('',(#17266,#17267,#17268,#17269));
#4900=EDGE_LOOP('',(#17270,#17271,#17272,#17273));
#4901=EDGE_LOOP('',(#17274,#17275,#17276,#17277));
#4902=EDGE_LOOP('',(#17278,#17279,#17280,#17281));
#4903=EDGE_LOOP('',(#17282,#17283,#17284,#17285));
#4904=EDGE_LOOP('',(#17286,#17287,#17288,#17289));
#4905=EDGE_LOOP('',(#17290,#17291,#17292,#17293));
#4906=EDGE_LOOP('',(#17294,#17295,#17296,#17297));
#4907=EDGE_LOOP('',(#17298,#17299,#17300,#17301));
#4908=EDGE_LOOP('',(#17302));
#4909=EDGE_LOOP('',(#17303,#17304,#17305,#17306));
#4910=EDGE_LOOP('',(#17307,#17308,#17309,#17310));
#4911=EDGE_LOOP('',(#17311));
#4912=EDGE_LOOP('',(#17312,#17313,#17314,#17315,#17316,#17317,#17318,#17319,
#17320,#17321,#17322,#17323,#17324,#17325,#17326,#17327,#17328,#17329,#17330,
#17331,#17332,#17333,#17334,#17335,#17336,#17337,#17338,#17339,#17340,#17341,
#17342,#17343,#17344,#17345,#17346,#17347,#17348,#17349,#17350,#17351,#17352,
#17353,#17354,#17355,#17356,#17357,#17358,#17359,#17360,#17361,#17362,#17363,
#17364,#17365,#17366,#17367,#17368,#17369,#17370,#17371,#17372,#17373,#17374,
#17375,#17376,#17377,#17378,#17379,#17380,#17381,#17382,#17383,#17384,#17385,
#17386,#17387,#17388,#17389,#17390,#17391,#17392,#17393,#17394,#17395,#17396,
#17397,#17398,#17399,#17400,#17401,#17402,#17403,#17404,#17405,#17406,#17407,
#17408,#17409,#17410,#17411,#17412,#17413,#17414,#17415,#17416,#17417,#17418,
#17419,#17420,#17421,#17422,#17423,#17424,#17425,#17426,#17427,#17428,#17429,
#17430,#17431,#17432,#17433,#17434,#17435,#17436,#17437,#17438,#17439,#17440));
#4913=EDGE_LOOP('',(#17441,#17442,#17443,#17444));
#4914=EDGE_LOOP('',(#17445,#17446,#17447,#17448,#17449,#17450,#17451,#17452,
#17453,#17454,#17455,#17456,#17457,#17458,#17459,#17460,#17461,#17462,#17463,
#17464,#17465,#17466,#17467,#17468,#17469,#17470,#17471,#17472,#17473,#17474,
#17475,#17476,#17477,#17478,#17479,#17480,#17481,#17482,#17483,#17484,#17485,
#17486,#17487,#17488,#17489,#17490,#17491,#17492,#17493,#17494,#17495,#17496,
#17497,#17498,#17499,#17500,#17501,#17502,#17503,#17504,#17505,#17506,#17507,
#17508,#17509,#17510,#17511,#17512,#17513,#17514,#17515,#17516,#17517,#17518,
#17519,#17520,#17521,#17522,#17523,#17524,#17525,#17526,#17527,#17528,#17529,
#17530,#17531,#17532,#17533,#17534,#17535,#17536,#17537,#17538,#17539,#17540,
#17541,#17542,#17543,#17544,#17545,#17546,#17547,#17548,#17549,#17550,#17551,
#17552,#17553,#17554,#17555,#17556,#17557,#17558,#17559,#17560,#17561,#17562,
#17563,#17564,#17565,#17566,#17567,#17568,#17569,#17570,#17571,#17572,#17573,
#17574));
#4915=EDGE_LOOP('',(#17575,#17576,#17577,#17578));
#4916=EDGE_LOOP('',(#17579,#17580,#17581,#17582));
#4917=EDGE_LOOP('',(#17583,#17584,#17585,#17586));
#4918=EDGE_LOOP('',(#17587,#17588,#17589,#17590));
#4919=EDGE_LOOP('',(#17591,#17592,#17593,#17594));
#4920=EDGE_LOOP('',(#17595,#17596,#17597,#17598));
#4921=EDGE_LOOP('',(#17599,#17600,#17601,#17602));
#4922=EDGE_LOOP('',(#17603));
#4923=EDGE_LOOP('',(#17604));
#4924=EDGE_LOOP('',(#17605,#17606,#17607,#17608,#17609));
#4925=EDGE_LOOP('',(#17610,#17611,#17612,#17613));
#4926=EDGE_LOOP('',(#17614));
#4927=EDGE_LOOP('',(#17615));
#4928=EDGE_LOOP('',(#17616,#17617,#17618,#17619));
#4929=EDGE_LOOP('',(#17620,#17621,#17622,#17623));
#4930=EDGE_LOOP('',(#17624,#17625,#17626,#17627));
#4931=EDGE_LOOP('',(#17628));
#4932=EDGE_LOOP('',(#17629));
#4933=EDGE_LOOP('',(#17630));
#4934=EDGE_LOOP('',(#17631));
#4935=EDGE_LOOP('',(#17632,#17633));
#4936=EDGE_LOOP('',(#17634,#17635,#17636,#17637,#17638,#17639,#17640,#17641,
#17642));
#4937=EDGE_LOOP('',(#17643,#17644));
#4938=EDGE_LOOP('',(#17645,#17646,#17647,#17648));
#4939=EDGE_LOOP('',(#17649,#17650,#17651,#17652,#17653));
#4940=EDGE_LOOP('',(#17654,#17655,#17656,#17657));
#4941=EDGE_LOOP('',(#17658,#17659));
#4942=EDGE_LOOP('',(#17660));
#4943=EDGE_LOOP('',(#17661));
#4944=EDGE_LOOP('',(#17662));
#4945=EDGE_LOOP('',(#17663));
#4946=EDGE_LOOP('',(#17664,#17665,#17666,#17667));
#4947=EDGE_LOOP('',(#17668,#17669));
#4948=EDGE_LOOP('',(#17670,#17671,#17672,#17673,#17674,#17675,#17676,#17677,
#17678));
#4949=EDGE_LOOP('',(#17679,#17680));
#4950=EDGE_LOOP('',(#17681,#17682,#17683,#17684,#17685,#17686));
#4951=EDGE_LOOP('',(#17687,#17688,#17689,#17690));
#4952=EDGE_LOOP('',(#17691,#17692,#17693,#17694,#17695,#17696));
#4953=EDGE_LOOP('',(#17697));
#4954=EDGE_LOOP('',(#17698));
#4955=EDGE_LOOP('',(#17699,#17700,#17701,#17702));
#4956=EDGE_LOOP('',(#17703));
#4957=EDGE_LOOP('',(#17704));
#4958=EDGE_LOOP('',(#17705,#17706,#17707,#17708));
#4959=EDGE_LOOP('',(#17709,#17710,#17711,#17712));
#4960=EDGE_LOOP('',(#17713,#17714,#17715,#17716));
#4961=EDGE_LOOP('',(#17717,#17718,#17719,#17720,#17721));
#4962=EDGE_LOOP('',(#17722,#17723,#17724,#17725));
#4963=EDGE_LOOP('',(#17726,#17727));
#4964=EDGE_LOOP('',(#17728,#17729,#17730,#17731));
#4965=EDGE_LOOP('',(#17732,#17733,#17734,#17735));
#4966=EDGE_LOOP('',(#17736,#17737,#17738,#17739));
#4967=EDGE_LOOP('',(#17740));
#4968=EDGE_LOOP('',(#17741));
#4969=EDGE_LOOP('',(#17742));
#4970=EDGE_LOOP('',(#17743));
#4971=EDGE_LOOP('',(#17744,#17745,#17746,#17747));
#4972=EDGE_LOOP('',(#17748,#17749,#17750,#17751));
#4973=EDGE_LOOP('',(#17752));
#4974=EDGE_LOOP('',(#17753));
#4975=EDGE_LOOP('',(#17754));
#4976=EDGE_LOOP('',(#17755));
#4977=EDGE_LOOP('',(#17756,#17757,#17758,#17759,#17760,#17761,#17762,#17763));
#4978=EDGE_LOOP('',(#17764,#17765,#17766,#17767));
#4979=EDGE_LOOP('',(#17768,#17769,#17770,#17771));
#4980=EDGE_LOOP('',(#17772,#17773,#17774,#17775));
#4981=EDGE_LOOP('',(#17776,#17777,#17778,#17779));
#4982=EDGE_LOOP('',(#17780,#17781,#17782,#17783,#17784,#17785,#17786,#17787));
#4983=EDGE_LOOP('',(#17788,#17789,#17790,#17791));
#4984=EDGE_LOOP('',(#17792,#17793,#17794,#17795));
#4985=EDGE_LOOP('',(#17796,#17797,#17798,#17799));
#4986=EDGE_LOOP('',(#17800,#17801,#17802,#17803));
#4987=EDGE_LOOP('',(#17804,#17805,#17806,#17807));
#4988=EDGE_LOOP('',(#17808,#17809,#17810,#17811));
#4989=EDGE_LOOP('',(#17812,#17813,#17814,#17815));
#4990=EDGE_LOOP('',(#17816,#17817,#17818,#17819));
#4991=EDGE_LOOP('',(#17820,#17821,#17822,#17823));
#4992=EDGE_LOOP('',(#17824,#17825,#17826,#17827));
#4993=EDGE_LOOP('',(#17828,#17829,#17830,#17831,#17832,#17833));
#4994=EDGE_LOOP('',(#17834));
#4995=EDGE_LOOP('',(#17835,#17836,#17837,#17838,#17839,#17840));
#4996=EDGE_LOOP('',(#17841,#17842,#17843,#17844));
#4997=EDGE_LOOP('',(#17845,#17846,#17847,#17848));
#4998=EDGE_LOOP('',(#17849,#17850,#17851,#17852));
#4999=EDGE_LOOP('',(#17853));
#5000=EDGE_LOOP('',(#17854,#17855,#17856,#17857));
#5001=EDGE_LOOP('',(#17858,#17859,#17860,#17861));
#5002=EDGE_LOOP('',(#17862));
#5003=EDGE_LOOP('',(#17863));
#5004=EDGE_LOOP('',(#17864));
#5005=EDGE_LOOP('',(#17865));
#5006=EDGE_LOOP('',(#17866));
#5007=EDGE_LOOP('',(#17867,#17868,#17869,#17870));
#5008=EDGE_LOOP('',(#17871,#17872,#17873,#17874));
#5009=EDGE_LOOP('',(#17875,#17876,#17877,#17878));
#5010=EDGE_LOOP('',(#17879));
#5011=EDGE_LOOP('',(#17880));
#5012=EDGE_LOOP('',(#17881,#17882,#17883,#17884));
#5013=EDGE_LOOP('',(#17885,#17886,#17887,#17888));
#5014=EDGE_LOOP('',(#17889,#17890,#17891,#17892));
#5015=EDGE_LOOP('',(#17893));
#5016=EDGE_LOOP('',(#17894,#17895,#17896,#17897));
#5017=EDGE_LOOP('',(#17898,#17899,#17900,#17901));
#5018=EDGE_LOOP('',(#17902,#17903,#17904,#17905));
#5019=EDGE_LOOP('',(#17906,#17907,#17908,#17909));
#5020=EDGE_LOOP('',(#17910,#17911,#17912,#17913));
#5021=EDGE_LOOP('',(#17914,#17915,#17916,#17917));
#5022=EDGE_LOOP('',(#17918,#17919,#17920,#17921,#17922,#17923));
#5023=EDGE_LOOP('',(#17924,#17925,#17926,#17927,#17928,#17929));
#5024=EDGE_LOOP('',(#17930,#17931,#17932,#17933));
#5025=EDGE_LOOP('',(#17934));
#5026=EDGE_LOOP('',(#17935,#17936,#17937,#17938));
#5027=EDGE_LOOP('',(#17939));
#5028=EDGE_LOOP('',(#17940,#17941,#17942,#17943));
#5029=EDGE_LOOP('',(#17944));
#5030=EDGE_LOOP('',(#17945,#17946,#17947,#17948));
#5031=EDGE_LOOP('',(#17949));
#5032=EDGE_LOOP('',(#17950,#17951,#17952,#17953));
#5033=EDGE_LOOP('',(#17954));
#5034=EDGE_LOOP('',(#17955,#17956,#17957,#17958));
#5035=EDGE_LOOP('',(#17959));
#5036=EDGE_LOOP('',(#17960,#17961,#17962,#17963));
#5037=EDGE_LOOP('',(#17964));
#5038=EDGE_LOOP('',(#17965,#17966,#17967,#17968));
#5039=EDGE_LOOP('',(#17969));
#5040=EDGE_LOOP('',(#17970,#17971,#17972,#17973));
#5041=EDGE_LOOP('',(#17974));
#5042=EDGE_LOOP('',(#17975));
#5043=EDGE_LOOP('',(#17976,#17977,#17978,#17979));
#5044=EDGE_LOOP('',(#17980));
#5045=EDGE_LOOP('',(#17981));
#5046=EDGE_LOOP('',(#17982,#17983,#17984,#17985));
#5047=EDGE_LOOP('',(#17986));
#5048=EDGE_LOOP('',(#17987));
#5049=EDGE_LOOP('',(#17988,#17989,#17990,#17991));
#5050=EDGE_LOOP('',(#17992));
#5051=EDGE_LOOP('',(#17993));
#5052=EDGE_LOOP('',(#17994,#17995,#17996,#17997));
#5053=EDGE_LOOP('',(#17998,#17999,#18000,#18001));
#5054=EDGE_LOOP('',(#18002,#18003,#18004,#18005));
#5055=EDGE_LOOP('',(#18006,#18007,#18008,#18009));
#5056=EDGE_LOOP('',(#18010,#18011,#18012,#18013));
#5057=EDGE_LOOP('',(#18014,#18015,#18016,#18017));
#5058=EDGE_LOOP('',(#18018,#18019,#18020,#18021));
#5059=EDGE_LOOP('',(#18022,#18023,#18024,#18025));
#5060=EDGE_LOOP('',(#18026,#18027,#18028,#18029));
#5061=EDGE_LOOP('',(#18030,#18031,#18032,#18033));
#5062=EDGE_LOOP('',(#18034,#18035,#18036,#18037));
#5063=EDGE_LOOP('',(#18038,#18039,#18040,#18041));
#5064=EDGE_LOOP('',(#18042,#18043,#18044,#18045));
#5065=EDGE_LOOP('',(#18046,#18047,#18048,#18049));
#5066=EDGE_LOOP('',(#18050,#18051,#18052,#18053));
#5067=EDGE_LOOP('',(#18054,#18055,#18056,#18057));
#5068=EDGE_LOOP('',(#18058,#18059,#18060,#18061));
#5069=EDGE_LOOP('',(#18062,#18063,#18064,#18065));
#5070=EDGE_LOOP('',(#18066,#18067,#18068,#18069));
#5071=EDGE_LOOP('',(#18070));
#5072=EDGE_LOOP('',(#18071));
#5073=EDGE_LOOP('',(#18072));
#5074=EDGE_LOOP('',(#18073));
#5075=EDGE_LOOP('',(#18074));
#5076=EDGE_LOOP('',(#18075));
#5077=EDGE_LOOP('',(#18076));
#5078=EDGE_LOOP('',(#18077));
#5079=EDGE_LOOP('',(#18078));
#5080=EDGE_LOOP('',(#18079));
#5081=EDGE_LOOP('',(#18080));
#5082=EDGE_LOOP('',(#18081));
#5083=EDGE_LOOP('',(#18082));
#5084=EDGE_LOOP('',(#18083));
#5085=EDGE_LOOP('',(#18084,#18085,#18086,#18087));
#5086=EDGE_LOOP('',(#18088));
#5087=EDGE_LOOP('',(#18089));
#5088=EDGE_LOOP('',(#18090));
#5089=EDGE_LOOP('',(#18091));
#5090=EDGE_LOOP('',(#18092));
#5091=EDGE_LOOP('',(#18093));
#5092=EDGE_LOOP('',(#18094));
#5093=EDGE_LOOP('',(#18095));
#5094=EDGE_LOOP('',(#18096));
#5095=EDGE_LOOP('',(#18097));
#5096=EDGE_LOOP('',(#18098));
#5097=EDGE_LOOP('',(#18099));
#5098=EDGE_LOOP('',(#18100));
#5099=EDGE_LOOP('',(#18101));
#5100=EDGE_LOOP('',(#18102));
#5101=EDGE_LOOP('',(#18103));
#5102=EDGE_LOOP('',(#18104));
#5103=EDGE_LOOP('',(#18105));
#5104=EDGE_LOOP('',(#18106));
#5105=EDGE_LOOP('',(#18107));
#5106=EDGE_LOOP('',(#18108));
#5107=EDGE_LOOP('',(#18109));
#5108=EDGE_LOOP('',(#18110,#18111,#18112,#18113));
#5109=EDGE_LOOP('',(#18114,#18115,#18116,#18117));
#5110=EDGE_LOOP('',(#18118,#18119,#18120,#18121));
#5111=EDGE_LOOP('',(#18122,#18123,#18124,#18125));
#5112=EDGE_LOOP('',(#18126,#18127,#18128,#18129));
#5113=EDGE_LOOP('',(#18130,#18131,#18132,#18133));
#5114=EDGE_LOOP('',(#18134,#18135,#18136,#18137));
#5115=EDGE_LOOP('',(#18138));
#5116=EDGE_LOOP('',(#18139));
#5117=EDGE_LOOP('',(#18140,#18141,#18142,#18143));
#5118=EDGE_LOOP('',(#18144,#18145));
#5119=EDGE_LOOP('',(#18146));
#5120=EDGE_LOOP('',(#18147,#18148,#18149,#18150));
#5121=EDGE_LOOP('',(#18151));
#5122=EDGE_LOOP('',(#18152));
#5123=EDGE_LOOP('',(#18153,#18154,#18155,#18156));
#5124=EDGE_LOOP('',(#18157,#18158));
#5125=EDGE_LOOP('',(#18159));
#5126=EDGE_LOOP('',(#18160,#18161,#18162,#18163,#18164,#18165,#18166,#18167,
#18168,#18169));
#5127=EDGE_LOOP('',(#18170));
#5128=EDGE_LOOP('',(#18171));
#5129=EDGE_LOOP('',(#18172));
#5130=EDGE_LOOP('',(#18173));
#5131=EDGE_LOOP('',(#18174));
#5132=EDGE_LOOP('',(#18175));
#5133=EDGE_LOOP('',(#18176,#18177,#18178,#18179));
#5134=EDGE_LOOP('',(#18180,#18181,#18182,#18183));
#5135=EDGE_LOOP('',(#18184,#18185,#18186,#18187));
#5136=EDGE_LOOP('',(#18188,#18189,#18190,#18191));
#5137=EDGE_LOOP('',(#18192,#18193,#18194,#18195,#18196,#18197,#18198,#18199,
#18200,#18201));
#5138=EDGE_LOOP('',(#18202,#18203,#18204,#18205));
#5139=EDGE_LOOP('',(#18206,#18207,#18208,#18209));
#5140=EDGE_LOOP('',(#18210,#18211,#18212,#18213));
#5141=EDGE_LOOP('',(#18214,#18215,#18216,#18217));
#5142=EDGE_LOOP('',(#18218));
#5143=EDGE_LOOP('',(#18219));
#5144=EDGE_LOOP('',(#18220));
#5145=EDGE_LOOP('',(#18221));
#5146=EDGE_LOOP('',(#18222));
#5147=EDGE_LOOP('',(#18223));
#5148=EDGE_LOOP('',(#18224));
#5149=EDGE_LOOP('',(#18225));
#5150=EDGE_LOOP('',(#18226,#18227,#18228,#18229));
#5151=EDGE_LOOP('',(#18230,#18231,#18232,#18233));
#5152=EDGE_LOOP('',(#18234,#18235,#18236,#18237));
#5153=EDGE_LOOP('',(#18238,#18239,#18240,#18241));
#5154=EDGE_LOOP('',(#18242));
#5155=EDGE_LOOP('',(#18243));
#5156=EDGE_LOOP('',(#18244,#18245,#18246,#18247));
#5157=EDGE_LOOP('',(#18248,#18249,#18250,#18251));
#5158=EDGE_LOOP('',(#18252));
#5159=EDGE_LOOP('',(#18253,#18254,#18255,#18256));
#5160=EDGE_LOOP('',(#18257));
#5161=EDGE_LOOP('',(#18258,#18259,#18260,#18261));
#5162=EDGE_LOOP('',(#18262,#18263,#18264,#18265));
#5163=EDGE_LOOP('',(#18266));
#5164=EDGE_LOOP('',(#18267));
#5165=EDGE_LOOP('',(#18268));
#5166=EDGE_LOOP('',(#18269));
#5167=EDGE_LOOP('',(#18270,#18271,#18272,#18273));
#5168=EDGE_LOOP('',(#18274,#18275,#18276,#18277));
#5169=EDGE_LOOP('',(#18278));
#5170=EDGE_LOOP('',(#18279));
#5171=EDGE_LOOP('',(#18280));
#5172=EDGE_LOOP('',(#18281));
#5173=EDGE_LOOP('',(#18282,#18283,#18284,#18285));
#5174=EDGE_LOOP('',(#18286,#18287,#18288,#18289));
#5175=EDGE_LOOP('',(#18290));
#5176=EDGE_LOOP('',(#18291));
#5177=EDGE_LOOP('',(#18292,#18293,#18294,#18295));
#5178=EDGE_LOOP('',(#18296,#18297,#18298,#18299));
#5179=EDGE_LOOP('',(#18300,#18301,#18302,#18303));
#5180=EDGE_LOOP('',(#18304,#18305,#18306,#18307));
#5181=EDGE_LOOP('',(#18308));
#5182=EDGE_LOOP('',(#18309));
#5183=EDGE_LOOP('',(#18310,#18311,#18312,#18313));
#5184=EDGE_LOOP('',(#18314,#18315,#18316,#18317));
#5185=EDGE_LOOP('',(#18318));
#5186=EDGE_LOOP('',(#18319));
#5187=EDGE_LOOP('',(#18320));
#5188=EDGE_LOOP('',(#18321));
#5189=EDGE_LOOP('',(#18322));
#5190=EDGE_LOOP('',(#18323));
#5191=EDGE_LOOP('',(#18324));
#5192=EDGE_LOOP('',(#18325));
#5193=EDGE_LOOP('',(#18326));
#5194=EDGE_LOOP('',(#18327));
#5195=EDGE_LOOP('',(#18328,#18329,#18330,#18331));
#5196=EDGE_LOOP('',(#18332,#18333,#18334,#18335));
#5197=EDGE_LOOP('',(#18336,#18337,#18338,#18339));
#5198=EDGE_LOOP('',(#18340,#18341,#18342,#18343));
#5199=EDGE_LOOP('',(#18344));
#5200=EDGE_LOOP('',(#18345));
#5201=EDGE_LOOP('',(#18346,#18347,#18348,#18349));
#5202=EDGE_LOOP('',(#18350,#18351,#18352,#18353));
#5203=EDGE_LOOP('',(#18354));
#5204=EDGE_LOOP('',(#18355,#18356,#18357,#18358));
#5205=EDGE_LOOP('',(#18359));
#5206=EDGE_LOOP('',(#18360,#18361,#18362,#18363));
#5207=EDGE_LOOP('',(#18364,#18365,#18366,#18367));
#5208=EDGE_LOOP('',(#18368));
#5209=EDGE_LOOP('',(#18369));
#5210=EDGE_LOOP('',(#18370));
#5211=EDGE_LOOP('',(#18371));
#5212=EDGE_LOOP('',(#18372,#18373,#18374,#18375));
#5213=EDGE_LOOP('',(#18376,#18377,#18378,#18379));
#5214=EDGE_LOOP('',(#18380));
#5215=EDGE_LOOP('',(#18381));
#5216=EDGE_LOOP('',(#18382));
#5217=EDGE_LOOP('',(#18383));
#5218=EDGE_LOOP('',(#18384,#18385,#18386,#18387));
#5219=EDGE_LOOP('',(#18388,#18389,#18390,#18391));
#5220=EDGE_LOOP('',(#18392));
#5221=EDGE_LOOP('',(#18393));
#5222=EDGE_LOOP('',(#18394,#18395,#18396,#18397));
#5223=EDGE_LOOP('',(#18398,#18399,#18400,#18401));
#5224=EDGE_LOOP('',(#18402,#18403,#18404,#18405));
#5225=EDGE_LOOP('',(#18406,#18407,#18408,#18409));
#5226=EDGE_LOOP('',(#18410,#18411));
#5227=EDGE_LOOP('',(#18412));
#5228=EDGE_LOOP('',(#18413));
#5229=EDGE_LOOP('',(#18414));
#5230=EDGE_LOOP('',(#18415));
#5231=EDGE_LOOP('',(#18416,#18417,#18418,#18419));
#5232=EDGE_LOOP('',(#18420,#18421,#18422,#18423));
#5233=EDGE_LOOP('',(#18424));
#5234=EDGE_LOOP('',(#18425));
#5235=EDGE_LOOP('',(#18426,#18427,#18428,#18429));
#5236=EDGE_LOOP('',(#18430,#18431));
#5237=EDGE_LOOP('',(#18432));
#5238=EDGE_LOOP('',(#18433));
#5239=EDGE_LOOP('',(#18434));
#5240=EDGE_LOOP('',(#18435));
#5241=EDGE_LOOP('',(#18436,#18437,#18438,#18439));
#5242=EDGE_LOOP('',(#18440));
#5243=EDGE_LOOP('',(#18441));
#5244=EDGE_LOOP('',(#18442,#18443,#18444,#18445));
#5245=EDGE_LOOP('',(#18446,#18447,#18448,#18449));
#5246=EDGE_LOOP('',(#18450,#18451,#18452,#18453));
#5247=EDGE_LOOP('',(#18454,#18455,#18456,#18457));
#5248=EDGE_LOOP('',(#18458,#18459,#18460,#18461));
#5249=EDGE_LOOP('',(#18462,#18463,#18464,#18465));
#5250=EDGE_LOOP('',(#18466));
#5251=EDGE_LOOP('',(#18467,#18468,#18469,#18470));
#5252=EDGE_LOOP('',(#18471));
#5253=EDGE_LOOP('',(#18472,#18473,#18474,#18475));
#5254=EDGE_LOOP('',(#18476));
#5255=EDGE_LOOP('',(#18477));
#5256=EDGE_LOOP('',(#18478,#18479,#18480,#18481));
#5257=EDGE_LOOP('',(#18482,#18483,#18484,#18485));
#5258=EDGE_LOOP('',(#18486,#18487,#18488,#18489));
#5259=EDGE_LOOP('',(#18490,#18491,#18492,#18493));
#5260=EDGE_LOOP('',(#18494,#18495,#18496,#18497));
#5261=EDGE_LOOP('',(#18498,#18499,#18500,#18501));
#5262=EDGE_LOOP('',(#18502));
#5263=EDGE_LOOP('',(#18503,#18504,#18505,#18506));
#5264=EDGE_LOOP('',(#18507));
#5265=EDGE_LOOP('',(#18508,#18509,#18510,#18511));
#5266=EDGE_LOOP('',(#18512));
#5267=EDGE_LOOP('',(#18513));
#5268=EDGE_LOOP('',(#18514,#18515,#18516,#18517));
#5269=EDGE_LOOP('',(#18518));
#5270=EDGE_LOOP('',(#18519));
#5271=EDGE_LOOP('',(#18520,#18521,#18522,#18523));
#5272=EDGE_LOOP('',(#18524));
#5273=EDGE_LOOP('',(#18525));
#5274=EDGE_LOOP('',(#18526,#18527,#18528,#18529));
#5275=EDGE_LOOP('',(#18530));
#5276=EDGE_LOOP('',(#18531));
#5277=EDGE_LOOP('',(#18532,#18533,#18534,#18535));
#5278=EDGE_LOOP('',(#18536,#18537,#18538,#18539));
#5279=EDGE_LOOP('',(#18540,#18541,#18542,#18543));
#5280=EDGE_LOOP('',(#18544,#18545,#18546,#18547));
#5281=EDGE_LOOP('',(#18548,#18549,#18550,#18551));
#5282=EDGE_LOOP('',(#18552,#18553,#18554,#18555));
#5283=EDGE_LOOP('',(#18556,#18557,#18558,#18559));
#5284=EDGE_LOOP('',(#18560,#18561,#18562,#18563));
#5285=EDGE_LOOP('',(#18564,#18565,#18566,#18567));
#5286=EDGE_LOOP('',(#18568));
#5287=EDGE_LOOP('',(#18569));
#5288=EDGE_LOOP('',(#18570));
#5289=EDGE_LOOP('',(#18571));
#5290=EDGE_LOOP('',(#18572,#18573,#18574,#18575));
#5291=EDGE_LOOP('',(#18576,#18577,#18578,#18579));
#5292=EDGE_LOOP('',(#18580,#18581,#18582,#18583));
#5293=EDGE_LOOP('',(#18584,#18585,#18586,#18587));
#5294=EDGE_LOOP('',(#18588,#18589,#18590,#18591));
#5295=EDGE_LOOP('',(#18592,#18593,#18594,#18595));
#5296=EDGE_LOOP('',(#18596));
#5297=EDGE_LOOP('',(#18597));
#5298=EDGE_LOOP('',(#18598));
#5299=EDGE_LOOP('',(#18599));
#5300=EDGE_LOOP('',(#18600,#18601,#18602,#18603));
#5301=EDGE_LOOP('',(#18604,#18605,#18606,#18607,#18608,#18609,#18610,#18611,
#18612,#18613,#18614,#18615));
#5302=EDGE_LOOP('',(#18616,#18617,#18618,#18619,#18620,#18621,#18622,#18623,
#18624,#18625,#18626,#18627));
#5303=EDGE_LOOP('',(#18628,#18629,#18630,#18631,#18632,#18633));
#5304=EDGE_LOOP('',(#18634,#18635,#18636,#18637,#18638));
#5305=EDGE_LOOP('',(#18639,#18640,#18641,#18642));
#5306=EDGE_LOOP('',(#18643,#18644,#18645,#18646));
#5307=EDGE_LOOP('',(#18647));
#5308=EDGE_LOOP('',(#18648));
#5309=EDGE_LOOP('',(#18649,#18650,#18651,#18652,#18653));
#5310=EDGE_LOOP('',(#18654));
#5311=EDGE_LOOP('',(#18655));
#5312=EDGE_LOOP('',(#18656,#18657,#18658,#18659));
#5313=EDGE_LOOP('',(#18660,#18661,#18662,#18663,#18664,#18665));
#5314=EDGE_LOOP('',(#18666,#18667,#18668,#18669,#18670));
#5315=EDGE_LOOP('',(#18671));
#5316=EDGE_LOOP('',(#18672));
#5317=EDGE_LOOP('',(#18673,#18674,#18675,#18676));
#5318=EDGE_LOOP('',(#18677,#18678,#18679,#18680));
#5319=EDGE_LOOP('',(#18681,#18682,#18683,#18684));
#5320=EDGE_LOOP('',(#18685));
#5321=EDGE_LOOP('',(#18686));
#5322=EDGE_LOOP('',(#18687,#18688,#18689,#18690,#18691));
#5323=EDGE_LOOP('',(#18692,#18693));
#5324=EDGE_LOOP('',(#18694,#18695));
#5325=EDGE_LOOP('',(#18696,#18697));
#5326=EDGE_LOOP('',(#18698,#18699));
#5327=EDGE_LOOP('',(#18700,#18701));
#5328=EDGE_LOOP('',(#18702,#18703));
#5329=EDGE_LOOP('',(#18704,#18705));
#5330=EDGE_LOOP('',(#18706,#18707,#18708,#18709));
#5331=EDGE_LOOP('',(#18710,#18711,#18712,#18713,#18714,#18715,#18716,#18717,
#18718,#18719,#18720,#18721,#18722,#18723,#18724,#18725,#18726,#18727));
#5332=EDGE_LOOP('',(#18728,#18729,#18730,#18731));
#5333=EDGE_LOOP('',(#18732,#18733,#18734,#18735));
#5334=EDGE_LOOP('',(#18736,#18737,#18738,#18739));
#5335=EDGE_LOOP('',(#18740,#18741,#18742,#18743));
#5336=EDGE_LOOP('',(#18744,#18745,#18746,#18747,#18748,#18749));
#5337=EDGE_LOOP('',(#18750,#18751,#18752,#18753));
#5338=EDGE_LOOP('',(#18754,#18755,#18756,#18757));
#5339=EDGE_LOOP('',(#18758,#18759,#18760,#18761));
#5340=EDGE_LOOP('',(#18762,#18763,#18764,#18765));
#5341=EDGE_LOOP('',(#18766,#18767,#18768,#18769));
#5342=EDGE_LOOP('',(#18770,#18771,#18772,#18773,#18774,#18775,#18776,#18777,
#18778,#18779,#18780,#18781,#18782,#18783,#18784,#18785,#18786,#18787));
#5343=EDGE_LOOP('',(#18788,#18789,#18790,#18791));
#5344=EDGE_LOOP('',(#18792,#18793,#18794,#18795));
#5345=EDGE_LOOP('',(#18796));
#5346=EDGE_LOOP('',(#18797));
#5347=EDGE_LOOP('',(#18798,#18799,#18800,#18801));
#5348=EDGE_LOOP('',(#18802));
#5349=EDGE_LOOP('',(#18803));
#5350=EDGE_LOOP('',(#18804,#18805,#18806,#18807));
#5351=EDGE_LOOP('',(#18808));
#5352=EDGE_LOOP('',(#18809));
#5353=EDGE_LOOP('',(#18810,#18811,#18812,#18813));
#5354=EDGE_LOOP('',(#18814));
#5355=EDGE_LOOP('',(#18815));
#5356=EDGE_LOOP('',(#18816,#18817,#18818,#18819));
#5357=EDGE_LOOP('',(#18820));
#5358=EDGE_LOOP('',(#18821));
#5359=EDGE_LOOP('',(#18822,#18823,#18824,#18825));
#5360=EDGE_LOOP('',(#18826,#18827,#18828,#18829,#18830,#18831));
#5361=EDGE_LOOP('',(#18832,#18833,#18834,#18835,#18836));
#5362=EDGE_LOOP('',(#18837,#18838,#18839,#18840));
#5363=EDGE_LOOP('',(#18841,#18842,#18843,#18844));
#5364=EDGE_LOOP('',(#18845));
#5365=EDGE_LOOP('',(#18846));
#5366=EDGE_LOOP('',(#18847,#18848,#18849,#18850,#18851));
#5367=EDGE_LOOP('',(#18852));
#5368=EDGE_LOOP('',(#18853));
#5369=EDGE_LOOP('',(#18854,#18855,#18856,#18857));
#5370=EDGE_LOOP('',(#18858,#18859,#18860,#18861,#18862,#18863));
#5371=EDGE_LOOP('',(#18864,#18865,#18866,#18867,#18868));
#5372=EDGE_LOOP('',(#18869));
#5373=EDGE_LOOP('',(#18870));
#5374=EDGE_LOOP('',(#18871,#18872,#18873,#18874));
#5375=EDGE_LOOP('',(#18875,#18876,#18877,#18878));
#5376=EDGE_LOOP('',(#18879,#18880,#18881,#18882));
#5377=EDGE_LOOP('',(#18883));
#5378=EDGE_LOOP('',(#18884));
#5379=EDGE_LOOP('',(#18885,#18886,#18887,#18888,#18889));
#5380=EDGE_LOOP('',(#18890,#18891));
#5381=EDGE_LOOP('',(#18892,#18893));
#5382=EDGE_LOOP('',(#18894,#18895));
#5383=EDGE_LOOP('',(#18896,#18897));
#5384=EDGE_LOOP('',(#18898,#18899));
#5385=EDGE_LOOP('',(#18900,#18901));
#5386=EDGE_LOOP('',(#18902,#18903));
#5387=EDGE_LOOP('',(#18904,#18905));
#5388=EDGE_LOOP('',(#18906,#18907,#18908,#18909));
#5389=EDGE_LOOP('',(#18910,#18911,#18912,#18913,#18914,#18915,#18916,#18917,
#18918,#18919,#18920,#18921,#18922,#18923,#18924,#18925,#18926,#18927,#18928,
#18929));
#5390=EDGE_LOOP('',(#18930,#18931,#18932,#18933));
#5391=EDGE_LOOP('',(#18934,#18935,#18936,#18937));
#5392=EDGE_LOOP('',(#18938,#18939,#18940,#18941));
#5393=EDGE_LOOP('',(#18942,#18943,#18944,#18945));
#5394=EDGE_LOOP('',(#18946,#18947,#18948,#18949));
#5395=EDGE_LOOP('',(#18950,#18951,#18952,#18953,#18954,#18955));
#5396=EDGE_LOOP('',(#18956,#18957,#18958,#18959));
#5397=EDGE_LOOP('',(#18960,#18961,#18962,#18963));
#5398=EDGE_LOOP('',(#18964,#18965,#18966,#18967));
#5399=EDGE_LOOP('',(#18968,#18969,#18970,#18971));
#5400=EDGE_LOOP('',(#18972,#18973,#18974,#18975));
#5401=EDGE_LOOP('',(#18976,#18977,#18978,#18979));
#5402=EDGE_LOOP('',(#18980,#18981,#18982,#18983,#18984,#18985,#18986,#18987,
#18988,#18989,#18990,#18991,#18992,#18993,#18994,#18995,#18996,#18997,#18998,
#18999));
#5403=EDGE_LOOP('',(#19000,#19001,#19002,#19003));
#5404=EDGE_LOOP('',(#19004,#19005,#19006,#19007));
#5405=EDGE_LOOP('',(#19008));
#5406=EDGE_LOOP('',(#19009));
#5407=EDGE_LOOP('',(#19010,#19011,#19012,#19013));
#5408=EDGE_LOOP('',(#19014));
#5409=EDGE_LOOP('',(#19015));
#5410=EDGE_LOOP('',(#19016,#19017,#19018,#19019));
#5411=EDGE_LOOP('',(#19020));
#5412=EDGE_LOOP('',(#19021));
#5413=EDGE_LOOP('',(#19022,#19023,#19024,#19025));
#5414=EDGE_LOOP('',(#19026));
#5415=EDGE_LOOP('',(#19027));
#5416=EDGE_LOOP('',(#19028,#19029,#19030,#19031));
#5417=EDGE_LOOP('',(#19032));
#5418=EDGE_LOOP('',(#19033));
#5419=EDGE_LOOP('',(#19034,#19035,#19036,#19037));
#5420=EDGE_LOOP('',(#19038,#19039,#19040,#19041));
#5421=EDGE_LOOP('',(#19042,#19043,#19044,#19045));
#5422=EDGE_LOOP('',(#19046,#19047,#19048,#19049));
#5423=EDGE_LOOP('',(#19050,#19051,#19052,#19053));
#5424=EDGE_LOOP('',(#19054,#19055,#19056,#19057));
#5425=EDGE_LOOP('',(#19058,#19059,#19060,#19061));
#5426=EDGE_LOOP('',(#19062,#19063,#19064,#19065,#19066,#19067));
#5427=EDGE_LOOP('',(#19068,#19069,#19070,#19071,#19072,#19073));
#5428=EDGE_LOOP('',(#19074));
#5429=EDGE_LOOP('',(#19075));
#5430=EDGE_LOOP('',(#19076,#19077,#19078,#19079));
#5431=EDGE_LOOP('',(#19080,#19081,#19082,#19083));
#5432=EDGE_LOOP('',(#19084,#19085,#19086,#19087));
#5433=EDGE_LOOP('',(#19088));
#5434=EDGE_LOOP('',(#19089));
#5435=EDGE_LOOP('',(#19090,#19091,#19092,#19093));
#5436=EDGE_LOOP('',(#19094,#19095,#19096,#19097));
#5437=EDGE_LOOP('',(#19098,#19099,#19100,#19101));
#5438=EDGE_LOOP('',(#19102,#19103,#19104,#19105));
#5439=EDGE_LOOP('',(#19106,#19107,#19108,#19109));
#5440=EDGE_LOOP('',(#19110,#19111,#19112,#19113));
#5441=EDGE_LOOP('',(#19114,#19115,#19116,#19117));
#5442=EDGE_LOOP('',(#19118,#19119,#19120,#19121));
#5443=EDGE_LOOP('',(#19122,#19123,#19124,#19125));
#5444=EDGE_LOOP('',(#19126,#19127,#19128,#19129));
#5445=EDGE_LOOP('',(#19130,#19131,#19132,#19133));
#5446=EDGE_LOOP('',(#19134));
#5447=EDGE_LOOP('',(#19135));
#5448=EDGE_LOOP('',(#19136));
#5449=EDGE_LOOP('',(#19137));
#5450=EDGE_LOOP('',(#19138,#19139,#19140,#19141));
#5451=EDGE_LOOP('',(#19142));
#5452=EDGE_LOOP('',(#19143));
#5453=EDGE_LOOP('',(#19144));
#5454=EDGE_LOOP('',(#19145));
#5455=EDGE_LOOP('',(#19146,#19147,#19148,#19149));
#5456=EDGE_LOOP('',(#19150,#19151,#19152,#19153));
#5457=EDGE_LOOP('',(#19154,#19155,#19156,#19157));
#5458=EDGE_LOOP('',(#19158,#19159,#19160,#19161));
#5459=EDGE_LOOP('',(#19162,#19163,#19164,#19165));
#5460=EDGE_LOOP('',(#19166,#19167,#19168,#19169));
#5461=EDGE_LOOP('',(#19170,#19171,#19172,#19173));
#5462=EDGE_LOOP('',(#19174,#19175,#19176,#19177));
#5463=EDGE_LOOP('',(#19178,#19179,#19180,#19181));
#5464=EDGE_LOOP('',(#19182,#19183,#19184,#19185));
#5465=EDGE_LOOP('',(#19186,#19187,#19188,#19189));
#5466=EDGE_LOOP('',(#19190,#19191,#19192,#19193));
#5467=EDGE_LOOP('',(#19194,#19195,#19196,#19197));
#5468=EDGE_LOOP('',(#19198));
#5469=EDGE_LOOP('',(#19199));
#5470=EDGE_LOOP('',(#19200));
#5471=EDGE_LOOP('',(#19201));
#5472=EDGE_LOOP('',(#19202));
#5473=EDGE_LOOP('',(#19203));
#5474=EDGE_LOOP('',(#19204));
#5475=EDGE_LOOP('',(#19205));
#5476=EDGE_LOOP('',(#19206,#19207,#19208,#19209));
#5477=EDGE_LOOP('',(#19210));
#5478=EDGE_LOOP('',(#19211));
#5479=EDGE_LOOP('',(#19212));
#5480=EDGE_LOOP('',(#19213));
#5481=EDGE_LOOP('',(#19214));
#5482=EDGE_LOOP('',(#19215));
#5483=EDGE_LOOP('',(#19216));
#5484=EDGE_LOOP('',(#19217));
#5485=EDGE_LOOP('',(#19218,#19219,#19220,#19221));
#5486=EDGE_LOOP('',(#19222));
#5487=EDGE_LOOP('',(#19223,#19224,#19225,#19226));
#5488=EDGE_LOOP('',(#19227));
#5489=EDGE_LOOP('',(#19228,#19229,#19230,#19231));
#5490=EDGE_LOOP('',(#19232));
#5491=EDGE_LOOP('',(#19233,#19234,#19235,#19236));
#5492=EDGE_LOOP('',(#19237));
#5493=EDGE_LOOP('',(#19238,#19239,#19240,#19241));
#5494=EDGE_LOOP('',(#19242));
#5495=EDGE_LOOP('',(#19243,#19244,#19245,#19246));
#5496=EDGE_LOOP('',(#19247));
#5497=EDGE_LOOP('',(#19248,#19249,#19250,#19251));
#5498=EDGE_LOOP('',(#19252));
#5499=EDGE_LOOP('',(#19253,#19254,#19255,#19256));
#5500=EDGE_LOOP('',(#19257,#19258,#19259,#19260));
#5501=EDGE_LOOP('',(#19261,#19262,#19263,#19264));
#5502=EDGE_LOOP('',(#19265));
#5503=EDGE_LOOP('',(#19266));
#5504=EDGE_LOOP('',(#19267));
#5505=EDGE_LOOP('',(#19268));
#5506=EDGE_LOOP('',(#19269,#19270,#19271,#19272));
#5507=EDGE_LOOP('',(#19273,#19274,#19275,#19276));
#5508=EDGE_LOOP('',(#19277));
#5509=EDGE_LOOP('',(#19278,#19279,#19280,#19281));
#5510=EDGE_LOOP('',(#19282));
#5511=EDGE_LOOP('',(#19283));
#5512=EDGE_LOOP('',(#19284));
#5513=EDGE_LOOP('',(#19285));
#5514=EDGE_LOOP('',(#19286,#19287,#19288,#19289));
#5515=EDGE_LOOP('',(#19290,#19291));
#5516=EDGE_LOOP('',(#19292,#19293,#19294,#19295,#19296,#19297,#19298,#19299));
#5517=EDGE_LOOP('',(#19300,#19301));
#5518=EDGE_LOOP('',(#19302,#19303,#19304,#19305,#19306,#19307,#19308,#19309));
#5519=EDGE_LOOP('',(#19310,#19311));
#5520=EDGE_LOOP('',(#19312,#19313,#19314,#19315,#19316,#19317,#19318,#19319));
#5521=EDGE_LOOP('',(#19320,#19321));
#5522=EDGE_LOOP('',(#19322,#19323,#19324,#19325,#19326,#19327,#19328,#19329));
#5523=EDGE_LOOP('',(#19330,#19331,#19332,#19333,#19334,#19335,#19336,#19337,
#19338,#19339,#19340,#19341));
#5524=EDGE_LOOP('',(#19342,#19343,#19344,#19345,#19346,#19347,#19348,#19349,
#19350,#19351,#19352,#19353));
#5525=EDGE_LOOP('',(#19354,#19355,#19356,#19357,#19358,#19359,#19360,#19361,
#19362,#19363,#19364,#19365));
#5526=EDGE_LOOP('',(#19366,#19367,#19368,#19369,#19370,#19371,#19372,#19373,
#19374,#19375));
#5527=EDGE_LOOP('',(#19376,#19377,#19378,#19379));
#5528=EDGE_LOOP('',(#19380,#19381,#19382,#19383));
#5529=EDGE_LOOP('',(#19384));
#5530=EDGE_LOOP('',(#19385));
#5531=EDGE_LOOP('',(#19386));
#5532=EDGE_LOOP('',(#19387));
#5533=EDGE_LOOP('',(#19388,#19389,#19390,#19391));
#5534=EDGE_LOOP('',(#19392,#19393,#19394,#19395,#19396,#19397,#19398,#19399,
#19400,#19401));
#5535=EDGE_LOOP('',(#19402,#19403,#19404,#19405));
#5536=EDGE_LOOP('',(#19406,#19407,#19408,#19409));
#5537=EDGE_LOOP('',(#19410,#19411,#19412,#19413));
#5538=EDGE_LOOP('',(#19414,#19415,#19416,#19417));
#5539=EDGE_LOOP('',(#19418,#19419,#19420,#19421));
#5540=EDGE_LOOP('',(#19422,#19423,#19424,#19425,#19426,#19427,#19428,#19429,
#19430,#19431,#19432,#19433));
#5541=EDGE_LOOP('',(#19434,#19435,#19436,#19437));
#5542=EDGE_LOOP('',(#19438,#19439,#19440,#19441));
#5543=EDGE_LOOP('',(#19442,#19443,#19444,#19445));
#5544=EDGE_LOOP('',(#19446,#19447,#19448,#19449));
#5545=EDGE_LOOP('',(#19450,#19451,#19452,#19453));
#5546=EDGE_LOOP('',(#19454,#19455,#19456,#19457));
#5547=EDGE_LOOP('',(#19458,#19459,#19460,#19461));
#5548=EDGE_LOOP('',(#19462,#19463,#19464,#19465));
#5549=EDGE_LOOP('',(#19466,#19467,#19468,#19469,#19470,#19471,#19472,#19473));
#5550=EDGE_LOOP('',(#19474,#19475,#19476,#19477,#19478,#19479,#19480,#19481));
#5551=EDGE_LOOP('',(#19482,#19483,#19484,#19485));
#5552=EDGE_LOOP('',(#19486,#19487,#19488,#19489));
#5553=EDGE_LOOP('',(#19490,#19491,#19492,#19493));
#5554=EDGE_LOOP('',(#19494,#19495,#19496,#19497));
#5555=EDGE_LOOP('',(#19498,#19499,#19500,#19501));
#5556=EDGE_LOOP('',(#19502,#19503,#19504,#19505));
#5557=EDGE_LOOP('',(#19506,#19507,#19508,#19509));
#5558=EDGE_LOOP('',(#19510,#19511,#19512,#19513));
#5559=EDGE_LOOP('',(#19514,#19515,#19516,#19517,#19518,#19519,#19520,#19521));
#5560=EDGE_LOOP('',(#19522,#19523,#19524,#19525,#19526,#19527,#19528,#19529));
#5561=EDGE_LOOP('',(#19530,#19531,#19532,#19533));
#5562=EDGE_LOOP('',(#19534,#19535,#19536,#19537));
#5563=EDGE_LOOP('',(#19538));
#5564=EDGE_LOOP('',(#19539));
#5565=EDGE_LOOP('',(#19540,#19541,#19542,#19543));
#5566=EDGE_LOOP('',(#19544));
#5567=EDGE_LOOP('',(#19545));
#5568=EDGE_LOOP('',(#19546,#19547,#19548,#19549));
#5569=EDGE_LOOP('',(#19550,#19551,#19552,#19553));
#5570=EDGE_LOOP('',(#19554,#19555,#19556,#19557));
#5571=EDGE_LOOP('',(#19558,#19559,#19560,#19561));
#5572=EDGE_LOOP('',(#19562,#19563,#19564,#19565));
#5573=EDGE_LOOP('',(#19566,#19567,#19568,#19569));
#5574=EDGE_LOOP('',(#19570,#19571,#19572,#19573,#19574,#19575));
#5575=EDGE_LOOP('',(#19576,#19577,#19578,#19579,#19580,#19581));
#5576=EDGE_LOOP('',(#19582));
#5577=EDGE_LOOP('',(#19583));
#5578=EDGE_LOOP('',(#19584,#19585,#19586,#19587));
#5579=EDGE_LOOP('',(#19588));
#5580=EDGE_LOOP('',(#19589));
#5581=EDGE_LOOP('',(#19590,#19591,#19592,#19593));
#5582=EDGE_LOOP('',(#19594,#19595,#19596,#19597));
#5583=EDGE_LOOP('',(#19598,#19599,#19600,#19601));
#5584=EDGE_LOOP('',(#19602));
#5585=EDGE_LOOP('',(#19603));
#5586=EDGE_LOOP('',(#19604,#19605,#19606,#19607));
#5587=EDGE_LOOP('',(#19608,#19609,#19610,#19611));
#5588=EDGE_LOOP('',(#19612,#19613,#19614,#19615));
#5589=EDGE_LOOP('',(#19616,#19617,#19618,#19619));
#5590=EDGE_LOOP('',(#19620,#19621,#19622,#19623));
#5591=EDGE_LOOP('',(#19624,#19625,#19626,#19627));
#5592=EDGE_LOOP('',(#19628,#19629,#19630,#19631));
#5593=EDGE_LOOP('',(#19632,#19633,#19634,#19635));
#5594=EDGE_LOOP('',(#19636,#19637,#19638,#19639));
#5595=EDGE_LOOP('',(#19640,#19641,#19642,#19643));
#5596=EDGE_LOOP('',(#19644,#19645,#19646));
#5597=EDGE_LOOP('',(#19647,#19648,#19649,#19650));
#5598=EDGE_LOOP('',(#19651,#19652,#19653,#19654));
#5599=EDGE_LOOP('',(#19655,#19656,#19657,#19658));
#5600=EDGE_LOOP('',(#19659,#19660,#19661,#19662));
#5601=EDGE_LOOP('',(#19663,#19664,#19665,#19666));
#5602=EDGE_LOOP('',(#19667,#19668,#19669,#19670));
#5603=EDGE_LOOP('',(#19671,#19672,#19673,#19674));
#5604=EDGE_LOOP('',(#19675,#19676,#19677,#19678));
#5605=EDGE_LOOP('',(#19679,#19680,#19681,#19682));
#5606=EDGE_LOOP('',(#19683,#19684,#19685,#19686));
#5607=EDGE_LOOP('',(#19687,#19688,#19689,#19690,#19691,#19692,#19693,#19694,
#19695,#19696,#19697,#19698,#19699,#19700,#19701,#19702,#19703,#19704,#19705,
#19706,#19707,#19708));
#5608=EDGE_LOOP('',(#19709,#19710,#19711,#19712,#19713,#19714,#19715,#19716,
#19717,#19718,#19719,#19720,#19721,#19722,#19723,#19724,#19725,#19726,#19727,
#19728,#19729));
#5609=EDGE_LOOP('',(#19730,#19731));
#5610=EDGE_LOOP('',(#19732,#19733,#19734,#19735,#19736));
#5611=EDGE_LOOP('',(#19737));
#5612=EDGE_LOOP('',(#19738));
#5613=EDGE_LOOP('',(#19739));
#5614=EDGE_LOOP('',(#19740,#19741,#19742,#19743));
#5615=EDGE_LOOP('',(#19744,#19745,#19746,#19747));
#5616=EDGE_LOOP('',(#19748,#19749,#19750,#19751));
#5617=EDGE_LOOP('',(#19752,#19753,#19754,#19755));
#5618=EDGE_LOOP('',(#19756,#19757));
#5619=EDGE_LOOP('',(#19758));
#5620=EDGE_LOOP('',(#19759));
#5621=EDGE_LOOP('',(#19760));
#5622=EDGE_LOOP('',(#19761));
#5623=EDGE_LOOP('',(#19762,#19763,#19764,#19765));
#5624=EDGE_LOOP('',(#19766,#19767,#19768,#19769,#19770));
#5625=EDGE_LOOP('',(#19771,#19772,#19773,#19774));
#5626=EDGE_LOOP('',(#19775));
#5627=EDGE_LOOP('',(#19776,#19777,#19778,#19779));
#5628=EDGE_LOOP('',(#19780));
#5629=EDGE_LOOP('',(#19781,#19782,#19783,#19784));
#5630=EDGE_LOOP('',(#19785,#19786,#19787,#19788));
#5631=EDGE_LOOP('',(#19789,#19790,#19791,#19792));
#5632=EDGE_LOOP('',(#19793));
#5633=EDGE_LOOP('',(#19794));
#5634=EDGE_LOOP('',(#19795,#19796,#19797,#19798));
#5635=EDGE_LOOP('',(#19799,#19800,#19801,#19802));
#5636=EDGE_LOOP('',(#19803,#19804,#19805,#19806));
#5637=EDGE_LOOP('',(#19807));
#5638=EDGE_LOOP('',(#19808,#19809,#19810,#19811));
#5639=EDGE_LOOP('',(#19812,#19813,#19814,#19815));
#5640=EDGE_LOOP('',(#19816,#19817,#19818,#19819));
#5641=EDGE_LOOP('',(#19820,#19821,#19822,#19823));
#5642=EDGE_LOOP('',(#19824,#19825,#19826,#19827));
#5643=EDGE_LOOP('',(#19828,#19829,#19830,#19831));
#5644=EDGE_LOOP('',(#19832,#19833,#19834,#19835,#19836,#19837));
#5645=EDGE_LOOP('',(#19838,#19839,#19840,#19841,#19842,#19843));
#5646=EDGE_LOOP('',(#19844));
#5647=EDGE_LOOP('',(#19845,#19846,#19847,#19848));
#5648=EDGE_LOOP('',(#19849,#19850,#19851,#19852));
#5649=EDGE_LOOP('',(#19853,#19854,#19855,#19856));
#5650=EDGE_LOOP('',(#19857));
#5651=EDGE_LOOP('',(#19858));
#5652=EDGE_LOOP('',(#19859,#19860,#19861,#19862));
#5653=EDGE_LOOP('',(#19863,#19864,#19865,#19866));
#5654=EDGE_LOOP('',(#19867,#19868,#19869,#19870));
#5655=EDGE_LOOP('',(#19871));
#5656=EDGE_LOOP('',(#19872,#19873,#19874,#19875));
#5657=EDGE_LOOP('',(#19876,#19877,#19878,#19879));
#5658=EDGE_LOOP('',(#19880,#19881,#19882,#19883));
#5659=EDGE_LOOP('',(#19884,#19885,#19886,#19887));
#5660=EDGE_LOOP('',(#19888,#19889,#19890,#19891));
#5661=EDGE_LOOP('',(#19892,#19893,#19894,#19895));
#5662=EDGE_LOOP('',(#19896,#19897,#19898,#19899,#19900,#19901));
#5663=EDGE_LOOP('',(#19902,#19903,#19904,#19905,#19906,#19907));
#5664=EDGE_LOOP('',(#19908,#19909,#19910,#19911));
#5665=EDGE_LOOP('',(#19912,#19913,#19914,#19915));
#5666=EDGE_LOOP('',(#19916,#19917,#19918,#19919));
#5667=EDGE_LOOP('',(#19920,#19921,#19922,#19923));
#5668=EDGE_LOOP('',(#19924,#19925,#19926,#19927));
#5669=EDGE_LOOP('',(#19928,#19929,#19930,#19931));
#5670=EDGE_LOOP('',(#19932,#19933,#19934,#19935));
#5671=EDGE_LOOP('',(#19936,#19937,#19938,#19939));
#5672=EDGE_LOOP('',(#19940,#19941,#19942,#19943));
#5673=EDGE_LOOP('',(#19944,#19945,#19946,#19947));
#5674=EDGE_LOOP('',(#19948,#19949,#19950,#19951));
#5675=EDGE_LOOP('',(#19952,#19953,#19954,#19955));
#5676=EDGE_LOOP('',(#19956,#19957,#19958,#19959));
#5677=EDGE_LOOP('',(#19960,#19961,#19962,#19963));
#5678=EDGE_LOOP('',(#19964,#19965,#19966,#19967));
#5679=EDGE_LOOP('',(#19968,#19969,#19970,#19971));
#5680=EDGE_LOOP('',(#19972,#19973,#19974,#19975));
#5681=EDGE_LOOP('',(#19976,#19977,#19978,#19979));
#5682=EDGE_LOOP('',(#19980,#19981,#19982,#19983));
#5683=EDGE_LOOP('',(#19984,#19985,#19986,#19987));
#5684=EDGE_LOOP('',(#19988,#19989,#19990,#19991));
#5685=EDGE_LOOP('',(#19992,#19993,#19994,#19995));
#5686=EDGE_LOOP('',(#19996,#19997,#19998,#19999));
#5687=EDGE_LOOP('',(#20000,#20001,#20002,#20003));
#5688=EDGE_LOOP('',(#20004,#20005,#20006,#20007));
#5689=EDGE_LOOP('',(#20008,#20009,#20010,#20011));
#5690=EDGE_LOOP('',(#20012,#20013,#20014,#20015));
#5691=EDGE_LOOP('',(#20016,#20017,#20018,#20019));
#5692=EDGE_LOOP('',(#20020,#20021,#20022,#20023));
#5693=EDGE_LOOP('',(#20024,#20025,#20026,#20027));
#5694=EDGE_LOOP('',(#20028,#20029,#20030,#20031));
#5695=EDGE_LOOP('',(#20032,#20033,#20034,#20035));
#5696=EDGE_LOOP('',(#20036,#20037,#20038,#20039));
#5697=EDGE_LOOP('',(#20040,#20041,#20042,#20043));
#5698=EDGE_LOOP('',(#20044,#20045,#20046,#20047));
#5699=EDGE_LOOP('',(#20048,#20049,#20050,#20051));
#5700=EDGE_LOOP('',(#20052,#20053,#20054,#20055));
#5701=EDGE_LOOP('',(#20056,#20057,#20058,#20059));
#5702=EDGE_LOOP('',(#20060,#20061,#20062,#20063));
#5703=EDGE_LOOP('',(#20064,#20065,#20066,#20067));
#5704=EDGE_LOOP('',(#20068,#20069,#20070,#20071));
#5705=EDGE_LOOP('',(#20072,#20073,#20074,#20075));
#5706=EDGE_LOOP('',(#20076,#20077,#20078,#20079));
#5707=EDGE_LOOP('',(#20080,#20081,#20082,#20083));
#5708=EDGE_LOOP('',(#20084,#20085,#20086,#20087));
#5709=EDGE_LOOP('',(#20088,#20089,#20090,#20091));
#5710=EDGE_LOOP('',(#20092,#20093,#20094,#20095));
#5711=EDGE_LOOP('',(#20096,#20097,#20098,#20099));
#5712=EDGE_LOOP('',(#20100,#20101,#20102,#20103));
#5713=EDGE_LOOP('',(#20104,#20105,#20106,#20107));
#5714=EDGE_LOOP('',(#20108,#20109,#20110,#20111));
#5715=EDGE_LOOP('',(#20112,#20113,#20114,#20115));
#5716=EDGE_LOOP('',(#20116,#20117,#20118,#20119));
#5717=EDGE_LOOP('',(#20120,#20121,#20122,#20123));
#5718=EDGE_LOOP('',(#20124,#20125,#20126,#20127));
#5719=EDGE_LOOP('',(#20128,#20129,#20130,#20131));
#5720=EDGE_LOOP('',(#20132,#20133,#20134,#20135));
#5721=EDGE_LOOP('',(#20136,#20137,#20138,#20139));
#5722=EDGE_LOOP('',(#20140,#20141,#20142,#20143));
#5723=EDGE_LOOP('',(#20144,#20145,#20146,#20147));
#5724=EDGE_LOOP('',(#20148,#20149,#20150,#20151));
#5725=EDGE_LOOP('',(#20152,#20153,#20154,#20155));
#5726=EDGE_LOOP('',(#20156,#20157,#20158,#20159));
#5727=EDGE_LOOP('',(#20160,#20161,#20162));
#5728=EDGE_LOOP('',(#20163,#20164,#20165,#20166,#20167));
#5729=EDGE_LOOP('',(#20168,#20169,#20170,#20171));
#5730=EDGE_LOOP('',(#20172,#20173,#20174,#20175));
#5731=EDGE_LOOP('',(#20176,#20177,#20178,#20179));
#5732=EDGE_LOOP('',(#20180,#20181,#20182,#20183));
#5733=EDGE_LOOP('',(#20184,#20185,#20186,#20187));
#5734=EDGE_LOOP('',(#20188,#20189,#20190,#20191));
#5735=EDGE_LOOP('',(#20192,#20193,#20194,#20195));
#5736=EDGE_LOOP('',(#20196,#20197,#20198,#20199));
#5737=EDGE_LOOP('',(#20200,#20201,#20202,#20203));
#5738=EDGE_LOOP('',(#20204,#20205,#20206,#20207));
#5739=EDGE_LOOP('',(#20208,#20209,#20210,#20211));
#5740=EDGE_LOOP('',(#20212,#20213,#20214,#20215));
#5741=EDGE_LOOP('',(#20216,#20217,#20218,#20219));
#5742=EDGE_LOOP('',(#20220,#20221,#20222,#20223));
#5743=EDGE_LOOP('',(#20224,#20225,#20226,#20227));
#5744=EDGE_LOOP('',(#20228,#20229,#20230,#20231));
#5745=EDGE_LOOP('',(#20232,#20233,#20234,#20235));
#5746=EDGE_LOOP('',(#20236,#20237,#20238,#20239));
#5747=EDGE_LOOP('',(#20240,#20241,#20242,#20243));
#5748=EDGE_LOOP('',(#20244,#20245,#20246,#20247));
#5749=EDGE_LOOP('',(#20248,#20249,#20250,#20251));
#5750=EDGE_LOOP('',(#20252,#20253,#20254,#20255));
#5751=EDGE_LOOP('',(#20256,#20257,#20258,#20259));
#5752=EDGE_LOOP('',(#20260,#20261,#20262,#20263));
#5753=EDGE_LOOP('',(#20264,#20265,#20266,#20267));
#5754=EDGE_LOOP('',(#20268,#20269,#20270,#20271));
#5755=EDGE_LOOP('',(#20272,#20273,#20274,#20275));
#5756=EDGE_LOOP('',(#20276,#20277,#20278,#20279));
#5757=EDGE_LOOP('',(#20280,#20281,#20282,#20283));
#5758=EDGE_LOOP('',(#20284,#20285,#20286,#20287));
#5759=EDGE_LOOP('',(#20288,#20289,#20290,#20291));
#5760=EDGE_LOOP('',(#20292,#20293,#20294,#20295));
#5761=EDGE_LOOP('',(#20296,#20297,#20298,#20299));
#5762=EDGE_LOOP('',(#20300,#20301,#20302,#20303));
#5763=EDGE_LOOP('',(#20304,#20305,#20306,#20307));
#5764=EDGE_LOOP('',(#20308,#20309,#20310,#20311));
#5765=EDGE_LOOP('',(#20312,#20313,#20314,#20315));
#5766=EDGE_LOOP('',(#20316,#20317,#20318,#20319));
#5767=EDGE_LOOP('',(#20320,#20321,#20322,#20323));
#5768=EDGE_LOOP('',(#20324,#20325,#20326,#20327));
#5769=EDGE_LOOP('',(#20328,#20329,#20330,#20331));
#5770=EDGE_LOOP('',(#20332,#20333,#20334,#20335));
#5771=EDGE_LOOP('',(#20336,#20337,#20338,#20339));
#5772=EDGE_LOOP('',(#20340,#20341,#20342,#20343));
#5773=EDGE_LOOP('',(#20344,#20345,#20346,#20347));
#5774=EDGE_LOOP('',(#20348,#20349,#20350,#20351));
#5775=EDGE_LOOP('',(#20352,#20353,#20354,#20355));
#5776=EDGE_LOOP('',(#20356,#20357,#20358,#20359));
#5777=EDGE_LOOP('',(#20360,#20361,#20362,#20363));
#5778=EDGE_LOOP('',(#20364,#20365,#20366,#20367));
#5779=EDGE_LOOP('',(#20368,#20369,#20370,#20371));
#5780=EDGE_LOOP('',(#20372,#20373,#20374,#20375));
#5781=EDGE_LOOP('',(#20376,#20377,#20378,#20379));
#5782=EDGE_LOOP('',(#20380,#20381,#20382,#20383));
#5783=EDGE_LOOP('',(#20384,#20385,#20386,#20387));
#5784=EDGE_LOOP('',(#20388,#20389,#20390,#20391));
#5785=EDGE_LOOP('',(#20392,#20393,#20394,#20395));
#5786=EDGE_LOOP('',(#20396,#20397,#20398,#20399));
#5787=EDGE_LOOP('',(#20400,#20401,#20402,#20403));
#5788=EDGE_LOOP('',(#20404,#20405,#20406,#20407));
#5789=EDGE_LOOP('',(#20408,#20409,#20410,#20411));
#5790=EDGE_LOOP('',(#20412));
#5791=EDGE_LOOP('',(#20413,#20414,#20415,#20416));
#5792=EDGE_LOOP('',(#20417,#20418,#20419,#20420));
#5793=EDGE_LOOP('',(#20421));
#5794=EDGE_LOOP('',(#20422,#20423,#20424,#20425,#20426,#20427,#20428,#20429,
#20430,#20431,#20432,#20433,#20434,#20435,#20436,#20437,#20438,#20439,#20440,
#20441,#20442,#20443,#20444,#20445,#20446,#20447,#20448,#20449,#20450,#20451,
#20452,#20453,#20454,#20455,#20456,#20457,#20458,#20459,#20460,#20461,#20462,
#20463,#20464,#20465,#20466,#20467,#20468,#20469,#20470,#20471,#20472,#20473,
#20474,#20475,#20476,#20477,#20478,#20479,#20480,#20481,#20482,#20483,#20484,
#20485,#20486,#20487,#20488,#20489,#20490,#20491,#20492,#20493,#20494,#20495,
#20496,#20497,#20498,#20499,#20500,#20501,#20502,#20503,#20504,#20505,#20506,
#20507,#20508,#20509,#20510,#20511,#20512,#20513,#20514,#20515,#20516,#20517,
#20518,#20519,#20520,#20521,#20522,#20523,#20524,#20525,#20526,#20527,#20528,
#20529,#20530,#20531,#20532,#20533,#20534,#20535,#20536,#20537,#20538,#20539,
#20540,#20541,#20542,#20543,#20544,#20545,#20546,#20547,#20548,#20549,#20550));
#5795=EDGE_LOOP('',(#20551,#20552,#20553,#20554));
#5796=EDGE_LOOP('',(#20555,#20556,#20557,#20558,#20559,#20560,#20561,#20562,
#20563,#20564,#20565,#20566,#20567,#20568,#20569,#20570,#20571,#20572,#20573,
#20574,#20575,#20576,#20577,#20578,#20579,#20580,#20581,#20582,#20583,#20584,
#20585,#20586,#20587,#20588,#20589,#20590,#20591,#20592,#20593,#20594,#20595,
#20596,#20597,#20598,#20599,#20600,#20601,#20602,#20603,#20604,#20605,#20606,
#20607,#20608,#20609,#20610,#20611,#20612,#20613,#20614,#20615,#20616,#20617,
#20618,#20619,#20620,#20621,#20622,#20623,#20624,#20625,#20626,#20627,#20628,
#20629,#20630,#20631,#20632,#20633,#20634,#20635,#20636,#20637,#20638,#20639,
#20640,#20641,#20642,#20643,#20644,#20645,#20646,#20647,#20648,#20649,#20650,
#20651,#20652,#20653,#20654,#20655,#20656,#20657,#20658,#20659,#20660,#20661,
#20662,#20663,#20664,#20665,#20666,#20667,#20668,#20669,#20670,#20671,#20672,
#20673,#20674,#20675,#20676,#20677,#20678,#20679,#20680,#20681,#20682,#20683,
#20684));
#5797=EDGE_LOOP('',(#20685,#20686,#20687,#20688));
#5798=EDGE_LOOP('',(#20689,#20690,#20691,#20692));
#5799=EDGE_LOOP('',(#20693,#20694,#20695,#20696));
#5800=EDGE_LOOP('',(#20697,#20698,#20699,#20700));
#5801=EDGE_LOOP('',(#20701,#20702,#20703,#20704));
#5802=EDGE_LOOP('',(#20705,#20706,#20707,#20708));
#5803=EDGE_LOOP('',(#20709,#20710,#20711,#20712));
#5804=EDGE_LOOP('',(#20713));
#5805=EDGE_LOOP('',(#20714));
#5806=EDGE_LOOP('',(#20715,#20716,#20717,#20718,#20719));
#5807=EDGE_LOOP('',(#20720,#20721,#20722,#20723));
#5808=EDGE_LOOP('',(#20724));
#5809=EDGE_LOOP('',(#20725));
#5810=EDGE_LOOP('',(#20726,#20727,#20728,#20729));
#5811=EDGE_LOOP('',(#20730,#20731,#20732,#20733));
#5812=EDGE_LOOP('',(#20734,#20735,#20736,#20737));
#5813=EDGE_LOOP('',(#20738));
#5814=EDGE_LOOP('',(#20739));
#5815=EDGE_LOOP('',(#20740));
#5816=EDGE_LOOP('',(#20741));
#5817=EDGE_LOOP('',(#20742,#20743));
#5818=EDGE_LOOP('',(#20744,#20745,#20746,#20747,#20748,#20749,#20750,#20751,
#20752));
#5819=EDGE_LOOP('',(#20753,#20754));
#5820=EDGE_LOOP('',(#20755,#20756,#20757,#20758));
#5821=EDGE_LOOP('',(#20759,#20760,#20761,#20762,#20763));
#5822=EDGE_LOOP('',(#20764,#20765,#20766,#20767));
#5823=EDGE_LOOP('',(#20768,#20769));
#5824=EDGE_LOOP('',(#20770));
#5825=EDGE_LOOP('',(#20771));
#5826=EDGE_LOOP('',(#20772));
#5827=EDGE_LOOP('',(#20773));
#5828=EDGE_LOOP('',(#20774,#20775,#20776,#20777));
#5829=EDGE_LOOP('',(#20778,#20779));
#5830=EDGE_LOOP('',(#20780,#20781,#20782,#20783,#20784,#20785,#20786,#20787,
#20788));
#5831=EDGE_LOOP('',(#20789,#20790));
#5832=EDGE_LOOP('',(#20791,#20792,#20793,#20794,#20795,#20796));
#5833=EDGE_LOOP('',(#20797,#20798,#20799,#20800));
#5834=EDGE_LOOP('',(#20801,#20802,#20803,#20804,#20805,#20806));
#5835=EDGE_LOOP('',(#20807));
#5836=EDGE_LOOP('',(#20808));
#5837=EDGE_LOOP('',(#20809,#20810,#20811,#20812));
#5838=EDGE_LOOP('',(#20813));
#5839=EDGE_LOOP('',(#20814));
#5840=EDGE_LOOP('',(#20815,#20816,#20817,#20818));
#5841=EDGE_LOOP('',(#20819,#20820,#20821,#20822));
#5842=EDGE_LOOP('',(#20823,#20824,#20825,#20826));
#5843=EDGE_LOOP('',(#20827,#20828,#20829,#20830,#20831));
#5844=EDGE_LOOP('',(#20832,#20833,#20834,#20835));
#5845=EDGE_LOOP('',(#20836,#20837));
#5846=EDGE_LOOP('',(#20838,#20839,#20840,#20841));
#5847=EDGE_LOOP('',(#20842,#20843,#20844,#20845));
#5848=EDGE_LOOP('',(#20846,#20847,#20848,#20849));
#5849=EDGE_LOOP('',(#20850));
#5850=EDGE_LOOP('',(#20851));
#5851=EDGE_LOOP('',(#20852));
#5852=EDGE_LOOP('',(#20853));
#5853=EDGE_LOOP('',(#20854,#20855,#20856,#20857));
#5854=EDGE_LOOP('',(#20858,#20859,#20860,#20861));
#5855=EDGE_LOOP('',(#20862));
#5856=EDGE_LOOP('',(#20863));
#5857=EDGE_LOOP('',(#20864));
#5858=EDGE_LOOP('',(#20865));
#5859=EDGE_LOOP('',(#20866,#20867,#20868,#20869,#20870,#20871,#20872,#20873));
#5860=EDGE_LOOP('',(#20874,#20875,#20876,#20877));
#5861=EDGE_LOOP('',(#20878,#20879,#20880,#20881));
#5862=EDGE_LOOP('',(#20882,#20883,#20884,#20885));
#5863=EDGE_LOOP('',(#20886,#20887,#20888,#20889));
#5864=EDGE_LOOP('',(#20890,#20891,#20892,#20893,#20894,#20895,#20896,#20897));
#5865=EDGE_LOOP('',(#20898,#20899,#20900,#20901));
#5866=EDGE_LOOP('',(#20902,#20903,#20904,#20905));
#5867=EDGE_LOOP('',(#20906,#20907,#20908,#20909));
#5868=EDGE_LOOP('',(#20910,#20911,#20912,#20913));
#5869=EDGE_LOOP('',(#20914,#20915,#20916,#20917));
#5870=EDGE_LOOP('',(#20918,#20919,#20920,#20921));
#5871=EDGE_LOOP('',(#20922,#20923,#20924,#20925));
#5872=EDGE_LOOP('',(#20926,#20927,#20928,#20929));
#5873=EDGE_LOOP('',(#20930,#20931,#20932,#20933));
#5874=EDGE_LOOP('',(#20934,#20935,#20936,#20937));
#5875=EDGE_LOOP('',(#20938,#20939,#20940,#20941,#20942,#20943));
#5876=EDGE_LOOP('',(#20944));
#5877=EDGE_LOOP('',(#20945,#20946,#20947,#20948,#20949,#20950));
#5878=EDGE_LOOP('',(#20951,#20952,#20953,#20954));
#5879=EDGE_LOOP('',(#20955,#20956,#20957,#20958));
#5880=EDGE_LOOP('',(#20959,#20960,#20961,#20962));
#5881=EDGE_LOOP('',(#20963));
#5882=EDGE_LOOP('',(#20964,#20965,#20966,#20967));
#5883=EDGE_LOOP('',(#20968,#20969,#20970,#20971));
#5884=EDGE_LOOP('',(#20972));
#5885=EDGE_LOOP('',(#20973));
#5886=EDGE_LOOP('',(#20974));
#5887=EDGE_LOOP('',(#20975));
#5888=EDGE_LOOP('',(#20976));
#5889=EDGE_LOOP('',(#20977,#20978,#20979,#20980));
#5890=EDGE_LOOP('',(#20981,#20982,#20983,#20984));
#5891=EDGE_LOOP('',(#20985,#20986,#20987,#20988));
#5892=EDGE_LOOP('',(#20989));
#5893=EDGE_LOOP('',(#20990));
#5894=EDGE_LOOP('',(#20991,#20992,#20993,#20994));
#5895=EDGE_LOOP('',(#20995,#20996,#20997,#20998));
#5896=EDGE_LOOP('',(#20999,#21000,#21001,#21002));
#5897=EDGE_LOOP('',(#21003));
#5898=EDGE_LOOP('',(#21004,#21005,#21006,#21007));
#5899=EDGE_LOOP('',(#21008,#21009,#21010,#21011));
#5900=EDGE_LOOP('',(#21012,#21013,#21014,#21015));
#5901=EDGE_LOOP('',(#21016,#21017,#21018,#21019));
#5902=EDGE_LOOP('',(#21020,#21021,#21022,#21023));
#5903=EDGE_LOOP('',(#21024,#21025,#21026,#21027));
#5904=EDGE_LOOP('',(#21028,#21029,#21030,#21031,#21032,#21033));
#5905=EDGE_LOOP('',(#21034,#21035,#21036,#21037,#21038,#21039));
#5906=LINE('',#32878,#7393);
#5907=LINE('',#32884,#7394);
#5908=LINE('',#32890,#7395);
#5909=LINE('',#32896,#7396);
#5910=LINE('',#32902,#7397);
#5911=LINE('',#32908,#7398);
#5912=LINE('',#32914,#7399);
#5913=LINE('',#32920,#7400);
#5914=LINE('',#32926,#7401);
#5915=LINE('',#32932,#7402);
#5916=LINE('',#32937,#7403);
#5917=LINE('',#32939,#7404);
#5918=LINE('',#32941,#7405);
#5919=LINE('',#32942,#7406);
#5920=LINE('',#32945,#7407);
#5921=LINE('',#32947,#7408);
#5922=LINE('',#32948,#7409);
#5923=LINE('',#32951,#7410);
#5924=LINE('',#32953,#7411);
#5925=LINE('',#32954,#7412);
#5926=LINE('',#32956,#7413);
#5927=LINE('',#32957,#7414);
#5928=LINE('',#32964,#7415);
#5929=LINE('',#32966,#7416);
#5930=LINE('',#32968,#7417);
#5931=LINE('',#32969,#7418);
#5932=LINE('',#32972,#7419);
#5933=LINE('',#32974,#7420);
#5934=LINE('',#32975,#7421);
#5935=LINE('',#32978,#7422);
#5936=LINE('',#32980,#7423);
#5937=LINE('',#32981,#7424);
#5938=LINE('',#32983,#7425);
#5939=LINE('',#32984,#7426);
#5940=LINE('',#32991,#7427);
#5941=LINE('',#32993,#7428);
#5942=LINE('',#32995,#7429);
#5943=LINE('',#32996,#7430);
#5944=LINE('',#32999,#7431);
#5945=LINE('',#33001,#7432);
#5946=LINE('',#33002,#7433);
#5947=LINE('',#33005,#7434);
#5948=LINE('',#33007,#7435);
#5949=LINE('',#33008,#7436);
#5950=LINE('',#33010,#7437);
#5951=LINE('',#33011,#7438);
#5952=LINE('',#33018,#7439);
#5953=LINE('',#33022,#7440);
#5954=LINE('',#33027,#7441);
#5955=LINE('',#33031,#7442);
#5956=LINE('',#33037,#7443);
#5957=LINE('',#33043,#7444);
#5958=LINE('',#33049,#7445);
#5959=LINE('',#33055,#7446);
#5960=LINE('',#33061,#7447);
#5961=LINE('',#33068,#7448);
#5962=LINE('',#33077,#7449);
#5963=LINE('',#33084,#7450);
#5964=LINE('',#33092,#7451);
#5965=LINE('',#33094,#7452);
#5966=LINE('',#33096,#7453);
#5967=LINE('',#33097,#7454);
#5968=LINE('',#33098,#7455);
#5969=LINE('',#33099,#7456);
#5970=LINE('',#33103,#7457);
#5971=LINE('',#33107,#7458);
#5972=LINE('',#33111,#7459);
#5973=LINE('',#33115,#7460);
#5974=LINE('',#33119,#7461);
#5975=LINE('',#33120,#7462);
#5976=LINE('',#33121,#7463);
#5977=LINE('',#33124,#7464);
#5978=LINE('',#33125,#7465);
#5979=LINE('',#33128,#7466);
#5980=LINE('',#33129,#7467);
#5981=LINE('',#33131,#7468);
#5982=LINE('',#33138,#7469);
#5983=LINE('',#33144,#7470);
#5984=LINE('',#33150,#7471);
#5985=LINE('',#33156,#7472);
#5986=LINE('',#33163,#7473);
#5987=LINE('',#33169,#7474);
#5988=LINE('',#33176,#7475);
#5989=LINE('',#33182,#7476);
#5990=LINE('',#33184,#7477);
#5991=LINE('',#33186,#7478);
#5992=LINE('',#33187,#7479);
#5993=LINE('',#33190,#7480);
#5994=LINE('',#33192,#7481);
#5995=LINE('',#33193,#7482);
#5996=LINE('',#33196,#7483);
#5997=LINE('',#33198,#7484);
#5998=LINE('',#33199,#7485);
#5999=LINE('',#33201,#7486);
#6000=LINE('',#33202,#7487);
#6001=LINE('',#33210,#7488);
#6002=LINE('',#33216,#7489);
#6003=LINE('',#33222,#7490);
#6004=LINE('',#33228,#7491);
#6005=LINE('',#33235,#7492);
#6006=LINE('',#33241,#7493);
#6007=LINE('',#33250,#7494);
#6008=LINE('',#33256,#7495);
#6009=LINE('',#33262,#7496);
#6010=LINE('',#33268,#7497);
#6011=LINE('',#33276,#7498);
#6012=LINE('',#33281,#7499);
#6013=LINE('',#33288,#7500);
#6014=LINE('',#33294,#7501);
#6015=LINE('',#33296,#7502);
#6016=LINE('',#33298,#7503);
#6017=LINE('',#33299,#7504);
#6018=LINE('',#33302,#7505);
#6019=LINE('',#33304,#7506);
#6020=LINE('',#33305,#7507);
#6021=LINE('',#33308,#7508);
#6022=LINE('',#33310,#7509);
#6023=LINE('',#33311,#7510);
#6024=LINE('',#33313,#7511);
#6025=LINE('',#33314,#7512);
#6026=LINE('',#33322,#7513);
#6027=LINE('',#33328,#7514);
#6028=LINE('',#33334,#7515);
#6029=LINE('',#33339,#7516);
#6030=LINE('',#33341,#7517);
#6031=LINE('',#33343,#7518);
#6032=LINE('',#33344,#7519);
#6033=LINE('',#33353,#7520);
#6034=LINE('',#33361,#7521);
#6035=LINE('',#33368,#7522);
#6036=LINE('',#33376,#7523);
#6037=LINE('',#33380,#7524);
#6038=LINE('',#33382,#7525);
#6039=LINE('',#33384,#7526);
#6040=LINE('',#33385,#7527);
#6041=LINE('',#33388,#7528);
#6042=LINE('',#33390,#7529);
#6043=LINE('',#33391,#7530);
#6044=LINE('',#33394,#7531);
#6045=LINE('',#33396,#7532);
#6046=LINE('',#33397,#7533);
#6047=LINE('',#33399,#7534);
#6048=LINE('',#33400,#7535);
#6049=LINE('',#33408,#7536);
#6050=LINE('',#33416,#7537);
#6051=LINE('',#33420,#7538);
#6052=LINE('',#33422,#7539);
#6053=LINE('',#33424,#7540);
#6054=LINE('',#33425,#7541);
#6055=LINE('',#33428,#7542);
#6056=LINE('',#33430,#7543);
#6057=LINE('',#33431,#7544);
#6058=LINE('',#33434,#7545);
#6059=LINE('',#33436,#7546);
#6060=LINE('',#33437,#7547);
#6061=LINE('',#33439,#7548);
#6062=LINE('',#33440,#7549);
#6063=LINE('',#33448,#7550);
#6064=LINE('',#33457,#7551);
#6065=LINE('',#33466,#7552);
#6066=LINE('',#33475,#7553);
#6067=LINE('',#33483,#7554);
#6068=LINE('',#33487,#7555);
#6069=LINE('',#33491,#7556);
#6070=LINE('',#33495,#7557);
#6071=LINE('',#33499,#7558);
#6072=LINE('',#33501,#7559);
#6073=LINE('',#33503,#7560);
#6074=LINE('',#33504,#7561);
#6075=LINE('',#33507,#7562);
#6076=LINE('',#33509,#7563);
#6077=LINE('',#33510,#7564);
#6078=LINE('',#33513,#7565);
#6079=LINE('',#33515,#7566);
#6080=LINE('',#33516,#7567);
#6081=LINE('',#33519,#7568);
#6082=LINE('',#33521,#7569);
#6083=LINE('',#33522,#7570);
#6084=LINE('',#33525,#7571);
#6085=LINE('',#33527,#7572);
#6086=LINE('',#33528,#7573);
#6087=LINE('',#33531,#7574);
#6088=LINE('',#33533,#7575);
#6089=LINE('',#33534,#7576);
#6090=LINE('',#33537,#7577);
#6091=LINE('',#33539,#7578);
#6092=LINE('',#33540,#7579);
#6093=LINE('',#33543,#7580);
#6094=LINE('',#33545,#7581);
#6095=LINE('',#33546,#7582);
#6096=LINE('',#33549,#7583);
#6097=LINE('',#33551,#7584);
#6098=LINE('',#33552,#7585);
#6099=LINE('',#33555,#7586);
#6100=LINE('',#33557,#7587);
#6101=LINE('',#33558,#7588);
#6102=LINE('',#33561,#7589);
#6103=LINE('',#33563,#7590);
#6104=LINE('',#33564,#7591);
#6105=LINE('',#33566,#7592);
#6106=LINE('',#33567,#7593);
#6107=LINE('',#33584,#7594);
#6108=LINE('',#33590,#7595);
#6109=LINE('',#33594,#7596);
#6110=LINE('',#33600,#7597);
#6111=LINE('',#33605,#7598);
#6112=LINE('',#33620,#7599);
#6113=LINE('',#33629,#7600);
#6114=LINE('',#33633,#7601);
#6115=LINE('',#33637,#7602);
#6116=LINE('',#33640,#7603);
#6117=LINE('',#33776,#7604);
#6118=LINE('',#34029,#7605);
#6119=LINE('',#34071,#7606);
#6120=LINE('',#34076,#7607);
#6121=LINE('',#34085,#7608);
#6122=LINE('',#34090,#7609);
#6123=LINE('',#34110,#7610);
#6124=LINE('',#34116,#7611);
#6125=LINE('',#34120,#7612);
#6126=LINE('',#34126,#7613);
#6127=LINE('',#34131,#7614);
#6128=LINE('',#34146,#7615);
#6129=LINE('',#34155,#7616);
#6130=LINE('',#34159,#7617);
#6131=LINE('',#34163,#7618);
#6132=LINE('',#34166,#7619);
#6133=LINE('',#34319,#7620);
#6134=LINE('',#34615,#7621);
#6135=LINE('',#34657,#7622);
#6136=LINE('',#34662,#7623);
#6137=LINE('',#34671,#7624);
#6138=LINE('',#34676,#7625);
#6139=LINE('',#34688,#7626);
#6140=LINE('',#34694,#7627);
#6141=LINE('',#34700,#7628);
#6142=LINE('',#34706,#7629);
#6143=LINE('',#34711,#7630);
#6144=LINE('',#34713,#7631);
#6145=LINE('',#34715,#7632);
#6146=LINE('',#34716,#7633);
#6147=LINE('',#34719,#7634);
#6148=LINE('',#34721,#7635);
#6149=LINE('',#34722,#7636);
#6150=LINE('',#34725,#7637);
#6151=LINE('',#34727,#7638);
#6152=LINE('',#34728,#7639);
#6153=LINE('',#34730,#7640);
#6154=LINE('',#34731,#7641);
#6155=LINE('',#34739,#7642);
#6156=LINE('',#34745,#7643);
#6157=LINE('',#34751,#7644);
#6158=LINE('',#34757,#7645);
#6159=LINE('',#34763,#7646);
#6160=LINE('',#34769,#7647);
#6161=LINE('',#34775,#7648);
#6162=LINE('',#34781,#7649);
#6163=LINE('',#34787,#7650);
#6164=LINE('',#34793,#7651);
#6165=LINE('',#34799,#7652);
#6166=LINE('',#34805,#7653);
#6167=LINE('',#34810,#7654);
#6168=LINE('',#34812,#7655);
#6169=LINE('',#34814,#7656);
#6170=LINE('',#34815,#7657);
#6171=LINE('',#34818,#7658);
#6172=LINE('',#34820,#7659);
#6173=LINE('',#34821,#7660);
#6174=LINE('',#34824,#7661);
#6175=LINE('',#34826,#7662);
#6176=LINE('',#34827,#7663);
#6177=LINE('',#34829,#7664);
#6178=LINE('',#34830,#7665);
#6179=LINE('',#34838,#7666);
#6180=LINE('',#34845,#7667);
#6181=LINE('',#34852,#7668);
#6182=LINE('',#34859,#7669);
#6183=LINE('',#34866,#7670);
#6184=LINE('',#34873,#7671);
#6185=LINE('',#34880,#7672);
#6186=LINE('',#34887,#7673);
#6187=LINE('',#34892,#7674);
#6188=LINE('',#34894,#7675);
#6189=LINE('',#34896,#7676);
#6190=LINE('',#34897,#7677);
#6191=LINE('',#34900,#7678);
#6192=LINE('',#34902,#7679);
#6193=LINE('',#34903,#7680);
#6194=LINE('',#34906,#7681);
#6195=LINE('',#34908,#7682);
#6196=LINE('',#34909,#7683);
#6197=LINE('',#34911,#7684);
#6198=LINE('',#34912,#7685);
#6199=LINE('',#34920,#7686);
#6200=LINE('',#34924,#7687);
#6201=LINE('',#34928,#7688);
#6202=LINE('',#34932,#7689);
#6203=LINE('',#34936,#7690);
#6204=LINE('',#34940,#7691);
#6205=LINE('',#34944,#7692);
#6206=LINE('',#34948,#7693);
#6207=LINE('',#34952,#7694);
#6208=LINE('',#34956,#7695);
#6209=LINE('',#34960,#7696);
#6210=LINE('',#34964,#7697);
#6211=LINE('',#34968,#7698);
#6212=LINE('',#34972,#7699);
#6213=LINE('',#34976,#7700);
#6214=LINE('',#34980,#7701);
#6215=LINE('',#34982,#7702);
#6216=LINE('',#34984,#7703);
#6217=LINE('',#34986,#7704);
#6218=LINE('',#34988,#7705);
#6219=LINE('',#34990,#7706);
#6220=LINE('',#34991,#7707);
#6221=LINE('',#34993,#7708);
#6222=LINE('',#34995,#7709);
#6223=LINE('',#34997,#7710);
#6224=LINE('',#34999,#7711);
#6225=LINE('',#35001,#7712);
#6226=LINE('',#35002,#7713);
#6227=LINE('',#35005,#7714);
#6228=LINE('',#35007,#7715);
#6229=LINE('',#35009,#7716);
#6230=LINE('',#35011,#7717);
#6231=LINE('',#35012,#7718);
#6232=LINE('',#35014,#7719);
#6233=LINE('',#35016,#7720);
#6234=LINE('',#35018,#7721);
#6235=LINE('',#35020,#7722);
#6236=LINE('',#35021,#7723);
#6237=LINE('',#35024,#7724);
#6238=LINE('',#35025,#7725);
#6239=LINE('',#35028,#7726);
#6240=LINE('',#35029,#7727);
#6241=LINE('',#35032,#7728);
#6242=LINE('',#35033,#7729);
#6243=LINE('',#35036,#7730);
#6244=LINE('',#35037,#7731);
#6245=LINE('',#35039,#7732);
#6246=LINE('',#35042,#7733);
#6247=LINE('',#35043,#7734);
#6248=LINE('',#35046,#7735);
#6249=LINE('',#35047,#7736);
#6250=LINE('',#35050,#7737);
#6251=LINE('',#35051,#7738);
#6252=LINE('',#35054,#7739);
#6253=LINE('',#35055,#7740);
#6254=LINE('',#35057,#7741);
#6255=LINE('',#35063,#7742);
#6256=LINE('',#35065,#7743);
#6257=LINE('',#35067,#7744);
#6258=LINE('',#35068,#7745);
#6259=LINE('',#35071,#7746);
#6260=LINE('',#35073,#7747);
#6261=LINE('',#35074,#7748);
#6262=LINE('',#35077,#7749);
#6263=LINE('',#35079,#7750);
#6264=LINE('',#35080,#7751);
#6265=LINE('',#35083,#7752);
#6266=LINE('',#35085,#7753);
#6267=LINE('',#35086,#7754);
#6268=LINE('',#35089,#7755);
#6269=LINE('',#35091,#7756);
#6270=LINE('',#35092,#7757);
#6271=LINE('',#35095,#7758);
#6272=LINE('',#35097,#7759);
#6273=LINE('',#35098,#7760);
#6274=LINE('',#35101,#7761);
#6275=LINE('',#35103,#7762);
#6276=LINE('',#35104,#7763);
#6277=LINE('',#35106,#7764);
#6278=LINE('',#35107,#7765);
#6279=LINE('',#35114,#7766);
#6280=LINE('',#35116,#7767);
#6281=LINE('',#35118,#7768);
#6282=LINE('',#35119,#7769);
#6283=LINE('',#35122,#7770);
#6284=LINE('',#35124,#7771);
#6285=LINE('',#35125,#7772);
#6286=LINE('',#35128,#7773);
#6287=LINE('',#35130,#7774);
#6288=LINE('',#35131,#7775);
#6289=LINE('',#35134,#7776);
#6290=LINE('',#35136,#7777);
#6291=LINE('',#35137,#7778);
#6292=LINE('',#35140,#7779);
#6293=LINE('',#35142,#7780);
#6294=LINE('',#35143,#7781);
#6295=LINE('',#35146,#7782);
#6296=LINE('',#35148,#7783);
#6297=LINE('',#35149,#7784);
#6298=LINE('',#35152,#7785);
#6299=LINE('',#35154,#7786);
#6300=LINE('',#35155,#7787);
#6301=LINE('',#35157,#7788);
#6302=LINE('',#35158,#7789);
#6303=LINE('',#35169,#7790);
#6304=LINE('',#35173,#7791);
#6305=LINE('',#35180,#7792);
#6306=LINE('',#35187,#7793);
#6307=LINE('',#35189,#7794);
#6308=LINE('',#35191,#7795);
#6309=LINE('',#35192,#7796);
#6310=LINE('',#35195,#7797);
#6311=LINE('',#35197,#7798);
#6312=LINE('',#35198,#7799);
#6313=LINE('',#35201,#7800);
#6314=LINE('',#35203,#7801);
#6315=LINE('',#35204,#7802);
#6316=LINE('',#35207,#7803);
#6317=LINE('',#35209,#7804);
#6318=LINE('',#35210,#7805);
#6319=LINE('',#35213,#7806);
#6320=LINE('',#35215,#7807);
#6321=LINE('',#35216,#7808);
#6322=LINE('',#35218,#7809);
#6323=LINE('',#35219,#7810);
#6324=LINE('',#35229,#7811);
#6325=LINE('',#35238,#7812);
#6326=LINE('',#35242,#7813);
#6327=LINE('',#35246,#7814);
#6328=LINE('',#35253,#7815);
#6329=LINE('',#35255,#7816);
#6330=LINE('',#35260,#7817);
#6331=LINE('',#35332,#7818);
#6332=LINE('',#35419,#7819);
#6333=LINE('',#35509,#7820);
#6334=LINE('',#35596,#7821);
#6335=LINE('',#35686,#7822);
#6336=LINE('',#35773,#7823);
#6337=LINE('',#35860,#7824);
#6338=LINE('',#35950,#7825);
#6339=LINE('',#35966,#7826);
#6340=LINE('',#35992,#7827);
#6341=LINE('',#36029,#7828);
#6342=LINE('',#36066,#7829);
#6343=LINE('',#36104,#7830);
#6344=LINE('',#36141,#7831);
#6345=LINE('',#36178,#7832);
#6346=LINE('',#36216,#7833);
#6347=LINE('',#36254,#7834);
#6348=LINE('',#37419,#7835);
#6349=LINE('',#37431,#7836);
#6350=LINE('',#37435,#7837);
#6351=LINE('',#37439,#7838);
#6352=LINE('',#37443,#7839);
#6353=LINE('',#37444,#7840);
#6354=LINE('',#37445,#7841);
#6355=LINE('',#37454,#7842);
#6356=LINE('',#37464,#7843);
#6357=LINE('',#37468,#7844);
#6358=LINE('',#37472,#7845);
#6359=LINE('',#37479,#7846);
#6360=LINE('',#37483,#7847);
#6361=LINE('',#37487,#7848);
#6362=LINE('',#37492,#7849);
#6363=LINE('',#37494,#7850);
#6364=LINE('',#37496,#7851);
#6365=LINE('',#37497,#7852);
#6366=LINE('',#37500,#7853);
#6367=LINE('',#37502,#7854);
#6368=LINE('',#37503,#7855);
#6369=LINE('',#37506,#7856);
#6370=LINE('',#37508,#7857);
#6371=LINE('',#37509,#7858);
#6372=LINE('',#37512,#7859);
#6373=LINE('',#37514,#7860);
#6374=LINE('',#37515,#7861);
#6375=LINE('',#37518,#7862);
#6376=LINE('',#37520,#7863);
#6377=LINE('',#37521,#7864);
#6378=LINE('',#37523,#7865);
#6379=LINE('',#37524,#7866);
#6380=LINE('',#37534,#7867);
#6381=LINE('',#37538,#7868);
#6382=LINE('',#37542,#7869);
#6383=LINE('',#37549,#7870);
#6384=LINE('',#37553,#7871);
#6385=LINE('',#37557,#7872);
#6386=LINE('',#37562,#7873);
#6387=LINE('',#37564,#7874);
#6388=LINE('',#37566,#7875);
#6389=LINE('',#37567,#7876);
#6390=LINE('',#37570,#7877);
#6391=LINE('',#37572,#7878);
#6392=LINE('',#37573,#7879);
#6393=LINE('',#37576,#7880);
#6394=LINE('',#37578,#7881);
#6395=LINE('',#37579,#7882);
#6396=LINE('',#37582,#7883);
#6397=LINE('',#37584,#7884);
#6398=LINE('',#37585,#7885);
#6399=LINE('',#37588,#7886);
#6400=LINE('',#37590,#7887);
#6401=LINE('',#37591,#7888);
#6402=LINE('',#37593,#7889);
#6403=LINE('',#37594,#7890);
#6404=LINE('',#37622,#7891);
#6405=LINE('',#37652,#7892);
#6406=LINE('',#37739,#7893);
#6407=LINE('',#37829,#7894);
#6408=LINE('',#37916,#7895);
#6409=LINE('',#38003,#7896);
#6410=LINE('',#38090,#7897);
#6411=LINE('',#38177,#7898);
#6412=LINE('',#38264,#7899);
#6413=LINE('',#38336,#7900);
#6414=LINE('',#38387,#7901);
#6415=LINE('',#38435,#7902);
#6416=LINE('',#38483,#7903);
#6417=LINE('',#38534,#7904);
#6418=LINE('',#38585,#7905);
#6419=LINE('',#38633,#7906);
#6420=LINE('',#38684,#7907);
#6421=LINE('',#38735,#7908);
#6422=LINE('',#38783,#7909);
#6423=LINE('',#38831,#7910);
#6424=LINE('',#38882,#7911);
#6425=LINE('',#38933,#7912);
#6426=LINE('',#38981,#7913);
#6427=LINE('',#39032,#7914);
#6428=LINE('',#39083,#7915);
#6429=LINE('',#39131,#7916);
#6430=LINE('',#39179,#7917);
#6431=LINE('',#39230,#7918);
#6432=LINE('',#39281,#7919);
#6433=LINE('',#39329,#7920);
#6434=LINE('',#39380,#7921);
#6435=LINE('',#39431,#7922);
#6436=LINE('',#39479,#7923);
#6437=LINE('',#39527,#7924);
#6438=LINE('',#39578,#7925);
#6439=LINE('',#39629,#7926);
#6440=LINE('',#39677,#7927);
#6441=LINE('',#39728,#7928);
#6442=LINE('',#39779,#7929);
#6443=LINE('',#39827,#7930);
#6444=LINE('',#39875,#7931);
#6445=LINE('',#39926,#7932);
#6446=LINE('',#39977,#7933);
#6447=LINE('',#40025,#7934);
#6448=LINE('',#40076,#7935);
#6449=LINE('',#40127,#7936);
#6450=LINE('',#40175,#7937);
#6451=LINE('',#40223,#7938);
#6452=LINE('',#40274,#7939);
#6453=LINE('',#40325,#7940);
#6454=LINE('',#40373,#7941);
#6455=LINE('',#40424,#7942);
#6456=LINE('',#40475,#7943);
#6457=LINE('',#40523,#7944);
#6458=LINE('',#40571,#7945);
#6459=LINE('',#40622,#7946);
#6460=LINE('',#40688,#7947);
#6461=LINE('',#40778,#7948);
#6462=LINE('',#40865,#7949);
#6463=LINE('',#40952,#7950);
#6464=LINE('',#41039,#7951);
#6465=LINE('',#41126,#7952);
#6466=LINE('',#41213,#7953);
#6467=LINE('',#41303,#7954);
#6468=LINE('',#41313,#7955);
#6469=LINE('',#41349,#7956);
#6470=LINE('',#41387,#7957);
#6471=LINE('',#41423,#7958);
#6472=LINE('',#41461,#7959);
#6473=LINE('',#41497,#7960);
#6474=LINE('',#41535,#7961);
#6475=LINE('',#41572,#7962);
#6476=LINE('',#41607,#7963);
#6477=LINE('',#41634,#7964);
#6478=LINE('',#41658,#7965);
#6479=LINE('',#41682,#7966);
#6480=LINE('',#41706,#7967);
#6481=LINE('',#41732,#7968);
#6482=LINE('',#41756,#7969);
#6483=LINE('',#41780,#7970);
#6484=LINE('',#41806,#7971);
#6485=LINE('',#41830,#7972);
#6486=LINE('',#41854,#7973);
#6487=LINE('',#41878,#7974);
#6488=LINE('',#41904,#7975);
#6489=LINE('',#41928,#7976);
#6490=LINE('',#41952,#7977);
#6491=LINE('',#41978,#7978);
#6492=LINE('',#42002,#7979);
#6493=LINE('',#42026,#7980);
#6494=LINE('',#42050,#7981);
#6495=LINE('',#42076,#7982);
#6496=LINE('',#42100,#7983);
#6497=LINE('',#42124,#7984);
#6498=LINE('',#42150,#7985);
#6499=LINE('',#42174,#7986);
#6500=LINE('',#42198,#7987);
#6501=LINE('',#42222,#7988);
#6502=LINE('',#42248,#7989);
#6503=LINE('',#42272,#7990);
#6504=LINE('',#42296,#7991);
#6505=LINE('',#42322,#7992);
#6506=LINE('',#42346,#7993);
#6507=LINE('',#42370,#7994);
#6508=LINE('',#42394,#7995);
#6509=LINE('',#42420,#7996);
#6510=LINE('',#42444,#7997);
#6511=LINE('',#42468,#7998);
#6512=LINE('',#42494,#7999);
#6513=LINE('',#42518,#8000);
#6514=LINE('',#42542,#8001);
#6515=LINE('',#42566,#8002);
#6516=LINE('',#42592,#8003);
#6517=LINE('',#42616,#8004);
#6518=LINE('',#42640,#8005);
#6519=LINE('',#42666,#8006);
#6520=LINE('',#42690,#8007);
#6521=LINE('',#42714,#8008);
#6522=LINE('',#42739,#8009);
#6523=LINE('',#42766,#8010);
#6524=LINE('',#42803,#8011);
#6525=LINE('',#42839,#8012);
#6526=LINE('',#42877,#8013);
#6527=LINE('',#42913,#8014);
#6528=LINE('',#42951,#8015);
#6529=LINE('',#42988,#8016);
#6530=LINE('',#43104,#8017);
#6531=LINE('',#47238,#8018);
#6532=LINE('',#47240,#8019);
#6533=LINE('',#47242,#8020);
#6534=LINE('',#47243,#8021);
#6535=LINE('',#47248,#8022);
#6536=LINE('',#47249,#8023);
#6537=LINE('',#47252,#8024);
#6538=LINE('',#47253,#8025);
#6539=LINE('',#47256,#8026);
#6540=LINE('',#47257,#8027);
#6541=LINE('',#47264,#8028);
#6542=LINE('',#47274,#8029);
#6543=LINE('',#47282,#8030);
#6544=LINE('',#47288,#8031);
#6545=LINE('',#47296,#8032);
#6546=LINE('',#47334,#8033);
#6547=LINE('',#47373,#8034);
#6548=LINE('',#47378,#8035);
#6549=LINE('',#47384,#8036);
#6550=LINE('',#47393,#8037);
#6551=LINE('',#47398,#8038);
#6552=LINE('',#47428,#8039);
#6553=LINE('',#47467,#8040);
#6554=LINE('',#47471,#8041);
#6555=LINE('',#47473,#8042);
#6556=LINE('',#47475,#8043);
#6557=LINE('',#47477,#8044);
#6558=LINE('',#47479,#8045);
#6559=LINE('',#47480,#8046);
#6560=LINE('',#47483,#8047);
#6561=LINE('',#47485,#8048);
#6562=LINE('',#47486,#8049);
#6563=LINE('',#47489,#8050);
#6564=LINE('',#47491,#8051);
#6565=LINE('',#47493,#8052);
#6566=LINE('',#47495,#8053);
#6567=LINE('',#47496,#8054);
#6568=LINE('',#47506,#8055);
#6569=LINE('',#47517,#8056);
#6570=LINE('',#47523,#8057);
#6571=LINE('',#47532,#8058);
#6572=LINE('',#47538,#8059);
#6573=LINE('',#47546,#8060);
#6574=LINE('',#47548,#8061);
#6575=LINE('',#47550,#8062);
#6576=LINE('',#47552,#8063);
#6577=LINE('',#47554,#8064);
#6578=LINE('',#47556,#8065);
#6579=LINE('',#47558,#8066);
#6580=LINE('',#47559,#8067);
#6581=LINE('',#47562,#8068);
#6582=LINE('',#47564,#8069);
#6583=LINE('',#47565,#8070);
#6584=LINE('',#47568,#8071);
#6585=LINE('',#47569,#8072);
#6586=LINE('',#47572,#8073);
#6587=LINE('',#47573,#8074);
#6588=LINE('',#47576,#8075);
#6589=LINE('',#47577,#8076);
#6590=LINE('',#47581,#8077);
#6591=LINE('',#47582,#8078);
#6592=LINE('',#47584,#8079);
#6593=LINE('',#47585,#8080);
#6594=LINE('',#47587,#8081);
#6595=LINE('',#47589,#8082);
#6596=LINE('',#47591,#8083);
#6597=LINE('',#47597,#8084);
#6598=LINE('',#47599,#8085);
#6599=LINE('',#47601,#8086);
#6600=LINE('',#47602,#8087);
#6601=LINE('',#47605,#8088);
#6602=LINE('',#47607,#8089);
#6603=LINE('',#47608,#8090);
#6604=LINE('',#47611,#8091);
#6605=LINE('',#47613,#8092);
#6606=LINE('',#47614,#8093);
#6607=LINE('',#47617,#8094);
#6608=LINE('',#47619,#8095);
#6609=LINE('',#47620,#8096);
#6610=LINE('',#47623,#8097);
#6611=LINE('',#47625,#8098);
#6612=LINE('',#47626,#8099);
#6613=LINE('',#47628,#8100);
#6614=LINE('',#47629,#8101);
#6615=LINE('',#47637,#8102);
#6616=LINE('',#47641,#8103);
#6617=LINE('',#47645,#8104);
#6618=LINE('',#47652,#8105);
#6619=LINE('',#47658,#8106);
#6620=LINE('',#47669,#8107);
#6621=LINE('',#47673,#8108);
#6622=LINE('',#47677,#8109);
#6623=LINE('',#47684,#8110);
#6624=LINE('',#47688,#8111);
#6625=LINE('',#47692,#8112);
#6626=LINE('',#47697,#8113);
#6627=LINE('',#47699,#8114);
#6628=LINE('',#47701,#8115);
#6629=LINE('',#47702,#8116);
#6630=LINE('',#47705,#8117);
#6631=LINE('',#47707,#8118);
#6632=LINE('',#47708,#8119);
#6633=LINE('',#47711,#8120);
#6634=LINE('',#47713,#8121);
#6635=LINE('',#47714,#8122);
#6636=LINE('',#47717,#8123);
#6637=LINE('',#47719,#8124);
#6638=LINE('',#47720,#8125);
#6639=LINE('',#47723,#8126);
#6640=LINE('',#47725,#8127);
#6641=LINE('',#47726,#8128);
#6642=LINE('',#47728,#8129);
#6643=LINE('',#47729,#8130);
#6644=LINE('',#47786,#8131);
#6645=LINE('',#47793,#8132);
#6646=LINE('',#47800,#8133);
#6647=LINE('',#47807,#8134);
#6648=LINE('',#47814,#8135);
#6649=LINE('',#47821,#8136);
#6650=LINE('',#47828,#8137);
#6651=LINE('',#47835,#8138);
#6652=LINE('',#47842,#8139);
#6653=LINE('',#47851,#8140);
#6654=LINE('',#47860,#8141);
#6655=LINE('',#47869,#8142);
#6656=LINE('',#47877,#8143);
#6657=LINE('',#47881,#8144);
#6658=LINE('',#47885,#8145);
#6659=LINE('',#47889,#8146);
#6660=LINE('',#47894,#8147);
#6661=LINE('',#47900,#8148);
#6662=LINE('',#47906,#8149);
#6663=LINE('',#47912,#8150);
#6664=LINE('',#47918,#8151);
#6665=LINE('',#47924,#8152);
#6666=LINE('',#47930,#8153);
#6667=LINE('',#47936,#8154);
#6668=LINE('',#47942,#8155);
#6669=LINE('',#47948,#8156);
#6670=LINE('',#47953,#8157);
#6671=LINE('',#47955,#8158);
#6672=LINE('',#47957,#8159);
#6673=LINE('',#47958,#8160);
#6674=LINE('',#47961,#8161);
#6675=LINE('',#47963,#8162);
#6676=LINE('',#47964,#8163);
#6677=LINE('',#47967,#8164);
#6678=LINE('',#47969,#8165);
#6679=LINE('',#47970,#8166);
#6680=LINE('',#47972,#8167);
#6681=LINE('',#47973,#8168);
#6682=LINE('',#47980,#8169);
#6683=LINE('',#47984,#8170);
#6684=LINE('',#47989,#8171);
#6685=LINE('',#47993,#8172);
#6686=LINE('',#47999,#8173);
#6687=LINE('',#48005,#8174);
#6688=LINE('',#48011,#8175);
#6689=LINE('',#48017,#8176);
#6690=LINE('',#48023,#8177);
#6691=LINE('',#48030,#8178);
#6692=LINE('',#48039,#8179);
#6693=LINE('',#48046,#8180);
#6694=LINE('',#48054,#8181);
#6695=LINE('',#48056,#8182);
#6696=LINE('',#48058,#8183);
#6697=LINE('',#48059,#8184);
#6698=LINE('',#48060,#8185);
#6699=LINE('',#48061,#8186);
#6700=LINE('',#48065,#8187);
#6701=LINE('',#48069,#8188);
#6702=LINE('',#48073,#8189);
#6703=LINE('',#48077,#8190);
#6704=LINE('',#48081,#8191);
#6705=LINE('',#48082,#8192);
#6706=LINE('',#48083,#8193);
#6707=LINE('',#48086,#8194);
#6708=LINE('',#48087,#8195);
#6709=LINE('',#48090,#8196);
#6710=LINE('',#48091,#8197);
#6711=LINE('',#48093,#8198);
#6712=LINE('',#48100,#8199);
#6713=LINE('',#48106,#8200);
#6714=LINE('',#48112,#8201);
#6715=LINE('',#48118,#8202);
#6716=LINE('',#48125,#8203);
#6717=LINE('',#48131,#8204);
#6718=LINE('',#48138,#8205);
#6719=LINE('',#48144,#8206);
#6720=LINE('',#48146,#8207);
#6721=LINE('',#48148,#8208);
#6722=LINE('',#48149,#8209);
#6723=LINE('',#48152,#8210);
#6724=LINE('',#48154,#8211);
#6725=LINE('',#48155,#8212);
#6726=LINE('',#48158,#8213);
#6727=LINE('',#48160,#8214);
#6728=LINE('',#48161,#8215);
#6729=LINE('',#48163,#8216);
#6730=LINE('',#48164,#8217);
#6731=LINE('',#48172,#8218);
#6732=LINE('',#48178,#8219);
#6733=LINE('',#48184,#8220);
#6734=LINE('',#48190,#8221);
#6735=LINE('',#48197,#8222);
#6736=LINE('',#48203,#8223);
#6737=LINE('',#48212,#8224);
#6738=LINE('',#48218,#8225);
#6739=LINE('',#48224,#8226);
#6740=LINE('',#48230,#8227);
#6741=LINE('',#48238,#8228);
#6742=LINE('',#48243,#8229);
#6743=LINE('',#48250,#8230);
#6744=LINE('',#48256,#8231);
#6745=LINE('',#48258,#8232);
#6746=LINE('',#48260,#8233);
#6747=LINE('',#48261,#8234);
#6748=LINE('',#48264,#8235);
#6749=LINE('',#48266,#8236);
#6750=LINE('',#48267,#8237);
#6751=LINE('',#48270,#8238);
#6752=LINE('',#48272,#8239);
#6753=LINE('',#48273,#8240);
#6754=LINE('',#48275,#8241);
#6755=LINE('',#48276,#8242);
#6756=LINE('',#48284,#8243);
#6757=LINE('',#48290,#8244);
#6758=LINE('',#48296,#8245);
#6759=LINE('',#48301,#8246);
#6760=LINE('',#48303,#8247);
#6761=LINE('',#48305,#8248);
#6762=LINE('',#48306,#8249);
#6763=LINE('',#48315,#8250);
#6764=LINE('',#48323,#8251);
#6765=LINE('',#48330,#8252);
#6766=LINE('',#48338,#8253);
#6767=LINE('',#48342,#8254);
#6768=LINE('',#48344,#8255);
#6769=LINE('',#48346,#8256);
#6770=LINE('',#48347,#8257);
#6771=LINE('',#48350,#8258);
#6772=LINE('',#48352,#8259);
#6773=LINE('',#48353,#8260);
#6774=LINE('',#48356,#8261);
#6775=LINE('',#48358,#8262);
#6776=LINE('',#48359,#8263);
#6777=LINE('',#48361,#8264);
#6778=LINE('',#48362,#8265);
#6779=LINE('',#48370,#8266);
#6780=LINE('',#48378,#8267);
#6781=LINE('',#48382,#8268);
#6782=LINE('',#48384,#8269);
#6783=LINE('',#48386,#8270);
#6784=LINE('',#48387,#8271);
#6785=LINE('',#48390,#8272);
#6786=LINE('',#48392,#8273);
#6787=LINE('',#48393,#8274);
#6788=LINE('',#48396,#8275);
#6789=LINE('',#48398,#8276);
#6790=LINE('',#48399,#8277);
#6791=LINE('',#48401,#8278);
#6792=LINE('',#48402,#8279);
#6793=LINE('',#48410,#8280);
#6794=LINE('',#48419,#8281);
#6795=LINE('',#48428,#8282);
#6796=LINE('',#48437,#8283);
#6797=LINE('',#48445,#8284);
#6798=LINE('',#48449,#8285);
#6799=LINE('',#48453,#8286);
#6800=LINE('',#48457,#8287);
#6801=LINE('',#48461,#8288);
#6802=LINE('',#48463,#8289);
#6803=LINE('',#48465,#8290);
#6804=LINE('',#48466,#8291);
#6805=LINE('',#48469,#8292);
#6806=LINE('',#48471,#8293);
#6807=LINE('',#48472,#8294);
#6808=LINE('',#48475,#8295);
#6809=LINE('',#48477,#8296);
#6810=LINE('',#48478,#8297);
#6811=LINE('',#48481,#8298);
#6812=LINE('',#48483,#8299);
#6813=LINE('',#48484,#8300);
#6814=LINE('',#48487,#8301);
#6815=LINE('',#48489,#8302);
#6816=LINE('',#48490,#8303);
#6817=LINE('',#48493,#8304);
#6818=LINE('',#48495,#8305);
#6819=LINE('',#48496,#8306);
#6820=LINE('',#48499,#8307);
#6821=LINE('',#48501,#8308);
#6822=LINE('',#48502,#8309);
#6823=LINE('',#48505,#8310);
#6824=LINE('',#48507,#8311);
#6825=LINE('',#48508,#8312);
#6826=LINE('',#48511,#8313);
#6827=LINE('',#48513,#8314);
#6828=LINE('',#48514,#8315);
#6829=LINE('',#48517,#8316);
#6830=LINE('',#48519,#8317);
#6831=LINE('',#48520,#8318);
#6832=LINE('',#48523,#8319);
#6833=LINE('',#48525,#8320);
#6834=LINE('',#48526,#8321);
#6835=LINE('',#48528,#8322);
#6836=LINE('',#48529,#8323);
#6837=LINE('',#48546,#8324);
#6838=LINE('',#48552,#8325);
#6839=LINE('',#48556,#8326);
#6840=LINE('',#48562,#8327);
#6841=LINE('',#48567,#8328);
#6842=LINE('',#48582,#8329);
#6843=LINE('',#48591,#8330);
#6844=LINE('',#48595,#8331);
#6845=LINE('',#48599,#8332);
#6846=LINE('',#48602,#8333);
#6847=LINE('',#48738,#8334);
#6848=LINE('',#48991,#8335);
#6849=LINE('',#49033,#8336);
#6850=LINE('',#49038,#8337);
#6851=LINE('',#49047,#8338);
#6852=LINE('',#49052,#8339);
#6853=LINE('',#49072,#8340);
#6854=LINE('',#49078,#8341);
#6855=LINE('',#49082,#8342);
#6856=LINE('',#49088,#8343);
#6857=LINE('',#49093,#8344);
#6858=LINE('',#49108,#8345);
#6859=LINE('',#49117,#8346);
#6860=LINE('',#49121,#8347);
#6861=LINE('',#49125,#8348);
#6862=LINE('',#49128,#8349);
#6863=LINE('',#49281,#8350);
#6864=LINE('',#49577,#8351);
#6865=LINE('',#49619,#8352);
#6866=LINE('',#49624,#8353);
#6867=LINE('',#49633,#8354);
#6868=LINE('',#49638,#8355);
#6869=LINE('',#49648,#8356);
#6870=LINE('',#49650,#8357);
#6871=LINE('',#49652,#8358);
#6872=LINE('',#49653,#8359);
#6873=LINE('',#49656,#8360);
#6874=LINE('',#49658,#8361);
#6875=LINE('',#49659,#8362);
#6876=LINE('',#49662,#8363);
#6877=LINE('',#49664,#8364);
#6878=LINE('',#49665,#8365);
#6879=LINE('',#49668,#8366);
#6880=LINE('',#49670,#8367);
#6881=LINE('',#49671,#8368);
#6882=LINE('',#49674,#8369);
#6883=LINE('',#49676,#8370);
#6884=LINE('',#49677,#8371);
#6885=LINE('',#49679,#8372);
#6886=LINE('',#49680,#8373);
#6887=LINE('',#49692,#8374);
#6888=LINE('',#49696,#8375);
#6889=LINE('',#49700,#8376);
#6890=LINE('',#49707,#8377);
#6891=LINE('',#49709,#8378);
#6892=LINE('',#49716,#8379);
#6893=LINE('',#49722,#8380);
#6894=LINE('',#49728,#8381);
#6895=LINE('',#49734,#8382);
#6896=LINE('',#49739,#8383);
#6897=LINE('',#49741,#8384);
#6898=LINE('',#49743,#8385);
#6899=LINE('',#49744,#8386);
#6900=LINE('',#49747,#8387);
#6901=LINE('',#49749,#8388);
#6902=LINE('',#49750,#8389);
#6903=LINE('',#49753,#8390);
#6904=LINE('',#49755,#8391);
#6905=LINE('',#49756,#8392);
#6906=LINE('',#49758,#8393);
#6907=LINE('',#49759,#8394);
#6908=LINE('',#49767,#8395);
#6909=LINE('',#49773,#8396);
#6910=LINE('',#49779,#8397);
#6911=LINE('',#49785,#8398);
#6912=LINE('',#49791,#8399);
#6913=LINE('',#49797,#8400);
#6914=LINE('',#49803,#8401);
#6915=LINE('',#49809,#8402);
#6916=LINE('',#49814,#8403);
#6917=LINE('',#49816,#8404);
#6918=LINE('',#49818,#8405);
#6919=LINE('',#49819,#8406);
#6920=LINE('',#49822,#8407);
#6921=LINE('',#49824,#8408);
#6922=LINE('',#49825,#8409);
#6923=LINE('',#49828,#8410);
#6924=LINE('',#49830,#8411);
#6925=LINE('',#49831,#8412);
#6926=LINE('',#49833,#8413);
#6927=LINE('',#49834,#8414);
#6928=LINE('',#49842,#8415);
#6929=LINE('',#49849,#8416);
#6930=LINE('',#49856,#8417);
#6931=LINE('',#49863,#8418);
#6932=LINE('',#49870,#8419);
#6933=LINE('',#49877,#8420);
#6934=LINE('',#49884,#8421);
#6935=LINE('',#49891,#8422);
#6936=LINE('',#49896,#8423);
#6937=LINE('',#49898,#8424);
#6938=LINE('',#49900,#8425);
#6939=LINE('',#49901,#8426);
#6940=LINE('',#49904,#8427);
#6941=LINE('',#49906,#8428);
#6942=LINE('',#49907,#8429);
#6943=LINE('',#49910,#8430);
#6944=LINE('',#49912,#8431);
#6945=LINE('',#49913,#8432);
#6946=LINE('',#49915,#8433);
#6947=LINE('',#49916,#8434);
#6948=LINE('',#49924,#8435);
#6949=LINE('',#49928,#8436);
#6950=LINE('',#49932,#8437);
#6951=LINE('',#49936,#8438);
#6952=LINE('',#49940,#8439);
#6953=LINE('',#49944,#8440);
#6954=LINE('',#49948,#8441);
#6955=LINE('',#49952,#8442);
#6956=LINE('',#49956,#8443);
#6957=LINE('',#49960,#8444);
#6958=LINE('',#49964,#8445);
#6959=LINE('',#49968,#8446);
#6960=LINE('',#49972,#8447);
#6961=LINE('',#49976,#8448);
#6962=LINE('',#49980,#8449);
#6963=LINE('',#49984,#8450);
#6964=LINE('',#49986,#8451);
#6965=LINE('',#49988,#8452);
#6966=LINE('',#49990,#8453);
#6967=LINE('',#49992,#8454);
#6968=LINE('',#49994,#8455);
#6969=LINE('',#49995,#8456);
#6970=LINE('',#49997,#8457);
#6971=LINE('',#49999,#8458);
#6972=LINE('',#50001,#8459);
#6973=LINE('',#50003,#8460);
#6974=LINE('',#50005,#8461);
#6975=LINE('',#50006,#8462);
#6976=LINE('',#50009,#8463);
#6977=LINE('',#50011,#8464);
#6978=LINE('',#50013,#8465);
#6979=LINE('',#50015,#8466);
#6980=LINE('',#50016,#8467);
#6981=LINE('',#50018,#8468);
#6982=LINE('',#50020,#8469);
#6983=LINE('',#50022,#8470);
#6984=LINE('',#50024,#8471);
#6985=LINE('',#50025,#8472);
#6986=LINE('',#50028,#8473);
#6987=LINE('',#50029,#8474);
#6988=LINE('',#50032,#8475);
#6989=LINE('',#50033,#8476);
#6990=LINE('',#50036,#8477);
#6991=LINE('',#50037,#8478);
#6992=LINE('',#50040,#8479);
#6993=LINE('',#50041,#8480);
#6994=LINE('',#50043,#8481);
#6995=LINE('',#50046,#8482);
#6996=LINE('',#50047,#8483);
#6997=LINE('',#50050,#8484);
#6998=LINE('',#50051,#8485);
#6999=LINE('',#50054,#8486);
#7000=LINE('',#50055,#8487);
#7001=LINE('',#50058,#8488);
#7002=LINE('',#50059,#8489);
#7003=LINE('',#50061,#8490);
#7004=LINE('',#50067,#8491);
#7005=LINE('',#50069,#8492);
#7006=LINE('',#50071,#8493);
#7007=LINE('',#50072,#8494);
#7008=LINE('',#50075,#8495);
#7009=LINE('',#50077,#8496);
#7010=LINE('',#50078,#8497);
#7011=LINE('',#50081,#8498);
#7012=LINE('',#50083,#8499);
#7013=LINE('',#50084,#8500);
#7014=LINE('',#50087,#8501);
#7015=LINE('',#50089,#8502);
#7016=LINE('',#50090,#8503);
#7017=LINE('',#50093,#8504);
#7018=LINE('',#50095,#8505);
#7019=LINE('',#50096,#8506);
#7020=LINE('',#50099,#8507);
#7021=LINE('',#50101,#8508);
#7022=LINE('',#50102,#8509);
#7023=LINE('',#50105,#8510);
#7024=LINE('',#50107,#8511);
#7025=LINE('',#50108,#8512);
#7026=LINE('',#50110,#8513);
#7027=LINE('',#50111,#8514);
#7028=LINE('',#50118,#8515);
#7029=LINE('',#50120,#8516);
#7030=LINE('',#50122,#8517);
#7031=LINE('',#50123,#8518);
#7032=LINE('',#50126,#8519);
#7033=LINE('',#50128,#8520);
#7034=LINE('',#50129,#8521);
#7035=LINE('',#50132,#8522);
#7036=LINE('',#50134,#8523);
#7037=LINE('',#50135,#8524);
#7038=LINE('',#50138,#8525);
#7039=LINE('',#50140,#8526);
#7040=LINE('',#50141,#8527);
#7041=LINE('',#50144,#8528);
#7042=LINE('',#50146,#8529);
#7043=LINE('',#50147,#8530);
#7044=LINE('',#50150,#8531);
#7045=LINE('',#50152,#8532);
#7046=LINE('',#50153,#8533);
#7047=LINE('',#50156,#8534);
#7048=LINE('',#50158,#8535);
#7049=LINE('',#50159,#8536);
#7050=LINE('',#50161,#8537);
#7051=LINE('',#50162,#8538);
#7052=LINE('',#50173,#8539);
#7053=LINE('',#50177,#8540);
#7054=LINE('',#50184,#8541);
#7055=LINE('',#50191,#8542);
#7056=LINE('',#50193,#8543);
#7057=LINE('',#50195,#8544);
#7058=LINE('',#50196,#8545);
#7059=LINE('',#50199,#8546);
#7060=LINE('',#50201,#8547);
#7061=LINE('',#50202,#8548);
#7062=LINE('',#50205,#8549);
#7063=LINE('',#50207,#8550);
#7064=LINE('',#50208,#8551);
#7065=LINE('',#50211,#8552);
#7066=LINE('',#50213,#8553);
#7067=LINE('',#50214,#8554);
#7068=LINE('',#50217,#8555);
#7069=LINE('',#50219,#8556);
#7070=LINE('',#50220,#8557);
#7071=LINE('',#50222,#8558);
#7072=LINE('',#50223,#8559);
#7073=LINE('',#50233,#8560);
#7074=LINE('',#50242,#8561);
#7075=LINE('',#50246,#8562);
#7076=LINE('',#50250,#8563);
#7077=LINE('',#50257,#8564);
#7078=LINE('',#50259,#8565);
#7079=LINE('',#50264,#8566);
#7080=LINE('',#50336,#8567);
#7081=LINE('',#50423,#8568);
#7082=LINE('',#50513,#8569);
#7083=LINE('',#50600,#8570);
#7084=LINE('',#50690,#8571);
#7085=LINE('',#50777,#8572);
#7086=LINE('',#50864,#8573);
#7087=LINE('',#50954,#8574);
#7088=LINE('',#50970,#8575);
#7089=LINE('',#50996,#8576);
#7090=LINE('',#51033,#8577);
#7091=LINE('',#51070,#8578);
#7092=LINE('',#51108,#8579);
#7093=LINE('',#51145,#8580);
#7094=LINE('',#51182,#8581);
#7095=LINE('',#51220,#8582);
#7096=LINE('',#51258,#8583);
#7097=LINE('',#52423,#8584);
#7098=LINE('',#52435,#8585);
#7099=LINE('',#52439,#8586);
#7100=LINE('',#52443,#8587);
#7101=LINE('',#52447,#8588);
#7102=LINE('',#52448,#8589);
#7103=LINE('',#52449,#8590);
#7104=LINE('',#52458,#8591);
#7105=LINE('',#52468,#8592);
#7106=LINE('',#52472,#8593);
#7107=LINE('',#52476,#8594);
#7108=LINE('',#52483,#8595);
#7109=LINE('',#52487,#8596);
#7110=LINE('',#52491,#8597);
#7111=LINE('',#52496,#8598);
#7112=LINE('',#52498,#8599);
#7113=LINE('',#52500,#8600);
#7114=LINE('',#52501,#8601);
#7115=LINE('',#52504,#8602);
#7116=LINE('',#52506,#8603);
#7117=LINE('',#52507,#8604);
#7118=LINE('',#52510,#8605);
#7119=LINE('',#52512,#8606);
#7120=LINE('',#52513,#8607);
#7121=LINE('',#52516,#8608);
#7122=LINE('',#52518,#8609);
#7123=LINE('',#52519,#8610);
#7124=LINE('',#52522,#8611);
#7125=LINE('',#52524,#8612);
#7126=LINE('',#52525,#8613);
#7127=LINE('',#52527,#8614);
#7128=LINE('',#52528,#8615);
#7129=LINE('',#52538,#8616);
#7130=LINE('',#52542,#8617);
#7131=LINE('',#52546,#8618);
#7132=LINE('',#52553,#8619);
#7133=LINE('',#52557,#8620);
#7134=LINE('',#52561,#8621);
#7135=LINE('',#52566,#8622);
#7136=LINE('',#52568,#8623);
#7137=LINE('',#52570,#8624);
#7138=LINE('',#52571,#8625);
#7139=LINE('',#52574,#8626);
#7140=LINE('',#52576,#8627);
#7141=LINE('',#52577,#8628);
#7142=LINE('',#52580,#8629);
#7143=LINE('',#52582,#8630);
#7144=LINE('',#52583,#8631);
#7145=LINE('',#52586,#8632);
#7146=LINE('',#52588,#8633);
#7147=LINE('',#52589,#8634);
#7148=LINE('',#52592,#8635);
#7149=LINE('',#52594,#8636);
#7150=LINE('',#52595,#8637);
#7151=LINE('',#52597,#8638);
#7152=LINE('',#52598,#8639);
#7153=LINE('',#52626,#8640);
#7154=LINE('',#52656,#8641);
#7155=LINE('',#52743,#8642);
#7156=LINE('',#52833,#8643);
#7157=LINE('',#52920,#8644);
#7158=LINE('',#53007,#8645);
#7159=LINE('',#53094,#8646);
#7160=LINE('',#53181,#8647);
#7161=LINE('',#53268,#8648);
#7162=LINE('',#53340,#8649);
#7163=LINE('',#53391,#8650);
#7164=LINE('',#53439,#8651);
#7165=LINE('',#53487,#8652);
#7166=LINE('',#53538,#8653);
#7167=LINE('',#53589,#8654);
#7168=LINE('',#53637,#8655);
#7169=LINE('',#53688,#8656);
#7170=LINE('',#53739,#8657);
#7171=LINE('',#53787,#8658);
#7172=LINE('',#53835,#8659);
#7173=LINE('',#53886,#8660);
#7174=LINE('',#53937,#8661);
#7175=LINE('',#53985,#8662);
#7176=LINE('',#54036,#8663);
#7177=LINE('',#54087,#8664);
#7178=LINE('',#54135,#8665);
#7179=LINE('',#54183,#8666);
#7180=LINE('',#54234,#8667);
#7181=LINE('',#54285,#8668);
#7182=LINE('',#54333,#8669);
#7183=LINE('',#54384,#8670);
#7184=LINE('',#54435,#8671);
#7185=LINE('',#54483,#8672);
#7186=LINE('',#54531,#8673);
#7187=LINE('',#54582,#8674);
#7188=LINE('',#54633,#8675);
#7189=LINE('',#54681,#8676);
#7190=LINE('',#54732,#8677);
#7191=LINE('',#54783,#8678);
#7192=LINE('',#54831,#8679);
#7193=LINE('',#54879,#8680);
#7194=LINE('',#54930,#8681);
#7195=LINE('',#54981,#8682);
#7196=LINE('',#55029,#8683);
#7197=LINE('',#55080,#8684);
#7198=LINE('',#55131,#8685);
#7199=LINE('',#55179,#8686);
#7200=LINE('',#55227,#8687);
#7201=LINE('',#55278,#8688);
#7202=LINE('',#55329,#8689);
#7203=LINE('',#55377,#8690);
#7204=LINE('',#55428,#8691);
#7205=LINE('',#55479,#8692);
#7206=LINE('',#55527,#8693);
#7207=LINE('',#55575,#8694);
#7208=LINE('',#55626,#8695);
#7209=LINE('',#55692,#8696);
#7210=LINE('',#55782,#8697);
#7211=LINE('',#55869,#8698);
#7212=LINE('',#55956,#8699);
#7213=LINE('',#56043,#8700);
#7214=LINE('',#56130,#8701);
#7215=LINE('',#56217,#8702);
#7216=LINE('',#56307,#8703);
#7217=LINE('',#56317,#8704);
#7218=LINE('',#56353,#8705);
#7219=LINE('',#56391,#8706);
#7220=LINE('',#56427,#8707);
#7221=LINE('',#56465,#8708);
#7222=LINE('',#56501,#8709);
#7223=LINE('',#56539,#8710);
#7224=LINE('',#56576,#8711);
#7225=LINE('',#56611,#8712);
#7226=LINE('',#56638,#8713);
#7227=LINE('',#56662,#8714);
#7228=LINE('',#56686,#8715);
#7229=LINE('',#56710,#8716);
#7230=LINE('',#56736,#8717);
#7231=LINE('',#56760,#8718);
#7232=LINE('',#56784,#8719);
#7233=LINE('',#56810,#8720);
#7234=LINE('',#56834,#8721);
#7235=LINE('',#56858,#8722);
#7236=LINE('',#56882,#8723);
#7237=LINE('',#56908,#8724);
#7238=LINE('',#56932,#8725);
#7239=LINE('',#56956,#8726);
#7240=LINE('',#56982,#8727);
#7241=LINE('',#57006,#8728);
#7242=LINE('',#57030,#8729);
#7243=LINE('',#57054,#8730);
#7244=LINE('',#57080,#8731);
#7245=LINE('',#57104,#8732);
#7246=LINE('',#57128,#8733);
#7247=LINE('',#57154,#8734);
#7248=LINE('',#57178,#8735);
#7249=LINE('',#57202,#8736);
#7250=LINE('',#57226,#8737);
#7251=LINE('',#57252,#8738);
#7252=LINE('',#57276,#8739);
#7253=LINE('',#57300,#8740);
#7254=LINE('',#57326,#8741);
#7255=LINE('',#57350,#8742);
#7256=LINE('',#57374,#8743);
#7257=LINE('',#57398,#8744);
#7258=LINE('',#57424,#8745);
#7259=LINE('',#57448,#8746);
#7260=LINE('',#57472,#8747);
#7261=LINE('',#57498,#8748);
#7262=LINE('',#57522,#8749);
#7263=LINE('',#57546,#8750);
#7264=LINE('',#57570,#8751);
#7265=LINE('',#57596,#8752);
#7266=LINE('',#57620,#8753);
#7267=LINE('',#57644,#8754);
#7268=LINE('',#57670,#8755);
#7269=LINE('',#57694,#8756);
#7270=LINE('',#57718,#8757);
#7271=LINE('',#57743,#8758);
#7272=LINE('',#57770,#8759);
#7273=LINE('',#57807,#8760);
#7274=LINE('',#57843,#8761);
#7275=LINE('',#57881,#8762);
#7276=LINE('',#57917,#8763);
#7277=LINE('',#57955,#8764);
#7278=LINE('',#57992,#8765);
#7279=LINE('',#58108,#8766);
#7280=LINE('',#62242,#8767);
#7281=LINE('',#62244,#8768);
#7282=LINE('',#62246,#8769);
#7283=LINE('',#62247,#8770);
#7284=LINE('',#62252,#8771);
#7285=LINE('',#62253,#8772);
#7286=LINE('',#62256,#8773);
#7287=LINE('',#62257,#8774);
#7288=LINE('',#62260,#8775);
#7289=LINE('',#62261,#8776);
#7290=LINE('',#62268,#8777);
#7291=LINE('',#62278,#8778);
#7292=LINE('',#62286,#8779);
#7293=LINE('',#62292,#8780);
#7294=LINE('',#62300,#8781);
#7295=LINE('',#62338,#8782);
#7296=LINE('',#62377,#8783);
#7297=LINE('',#62382,#8784);
#7298=LINE('',#62388,#8785);
#7299=LINE('',#62397,#8786);
#7300=LINE('',#62402,#8787);
#7301=LINE('',#62432,#8788);
#7302=LINE('',#62471,#8789);
#7303=LINE('',#62475,#8790);
#7304=LINE('',#62477,#8791);
#7305=LINE('',#62479,#8792);
#7306=LINE('',#62481,#8793);
#7307=LINE('',#62483,#8794);
#7308=LINE('',#62484,#8795);
#7309=LINE('',#62487,#8796);
#7310=LINE('',#62489,#8797);
#7311=LINE('',#62490,#8798);
#7312=LINE('',#62493,#8799);
#7313=LINE('',#62495,#8800);
#7314=LINE('',#62497,#8801);
#7315=LINE('',#62499,#8802);
#7316=LINE('',#62500,#8803);
#7317=LINE('',#62510,#8804);
#7318=LINE('',#62521,#8805);
#7319=LINE('',#62527,#8806);
#7320=LINE('',#62536,#8807);
#7321=LINE('',#62542,#8808);
#7322=LINE('',#62550,#8809);
#7323=LINE('',#62552,#8810);
#7324=LINE('',#62554,#8811);
#7325=LINE('',#62556,#8812);
#7326=LINE('',#62558,#8813);
#7327=LINE('',#62560,#8814);
#7328=LINE('',#62562,#8815);
#7329=LINE('',#62563,#8816);
#7330=LINE('',#62566,#8817);
#7331=LINE('',#62568,#8818);
#7332=LINE('',#62569,#8819);
#7333=LINE('',#62572,#8820);
#7334=LINE('',#62573,#8821);
#7335=LINE('',#62576,#8822);
#7336=LINE('',#62577,#8823);
#7337=LINE('',#62580,#8824);
#7338=LINE('',#62581,#8825);
#7339=LINE('',#62585,#8826);
#7340=LINE('',#62586,#8827);
#7341=LINE('',#62588,#8828);
#7342=LINE('',#62589,#8829);
#7343=LINE('',#62591,#8830);
#7344=LINE('',#62593,#8831);
#7345=LINE('',#62595,#8832);
#7346=LINE('',#62601,#8833);
#7347=LINE('',#62603,#8834);
#7348=LINE('',#62605,#8835);
#7349=LINE('',#62606,#8836);
#7350=LINE('',#62609,#8837);
#7351=LINE('',#62611,#8838);
#7352=LINE('',#62612,#8839);
#7353=LINE('',#62615,#8840);
#7354=LINE('',#62617,#8841);
#7355=LINE('',#62618,#8842);
#7356=LINE('',#62621,#8843);
#7357=LINE('',#62623,#8844);
#7358=LINE('',#62624,#8845);
#7359=LINE('',#62627,#8846);
#7360=LINE('',#62629,#8847);
#7361=LINE('',#62630,#8848);
#7362=LINE('',#62632,#8849);
#7363=LINE('',#62633,#8850);
#7364=LINE('',#62641,#8851);
#7365=LINE('',#62645,#8852);
#7366=LINE('',#62649,#8853);
#7367=LINE('',#62656,#8854);
#7368=LINE('',#62662,#8855);
#7369=LINE('',#62673,#8856);
#7370=LINE('',#62677,#8857);
#7371=LINE('',#62681,#8858);
#7372=LINE('',#62688,#8859);
#7373=LINE('',#62692,#8860);
#7374=LINE('',#62696,#8861);
#7375=LINE('',#62701,#8862);
#7376=LINE('',#62703,#8863);
#7377=LINE('',#62705,#8864);
#7378=LINE('',#62706,#8865);
#7379=LINE('',#62709,#8866);
#7380=LINE('',#62711,#8867);
#7381=LINE('',#62712,#8868);
#7382=LINE('',#62715,#8869);
#7383=LINE('',#62717,#8870);
#7384=LINE('',#62718,#8871);
#7385=LINE('',#62721,#8872);
#7386=LINE('',#62723,#8873);
#7387=LINE('',#62724,#8874);
#7388=LINE('',#62727,#8875);
#7389=LINE('',#62729,#8876);
#7390=LINE('',#62730,#8877);
#7391=LINE('',#62732,#8878);
#7392=LINE('',#62733,#8879);
#7393=VECTOR('',#26473,0.210000000000001);
#7394=VECTOR('',#26480,0.21);
#7395=VECTOR('',#26487,0.329999999999998);
#7396=VECTOR('',#26494,0.329999999999998);
#7397=VECTOR('',#26501,0.275);
#7398=VECTOR('',#26508,0.275);
#7399=VECTOR('',#26515,0.210000000000001);
#7400=VECTOR('',#26522,0.21);
#7401=VECTOR('',#26529,0.21);
#7402=VECTOR('',#26536,0.210000000000001);
#7403=VECTOR('',#26541,1.);
#7404=VECTOR('',#26542,1.);
#7405=VECTOR('',#26543,1.);
#7406=VECTOR('',#26544,1.);
#7407=VECTOR('',#26547,1.);
#7408=VECTOR('',#26548,1.);
#7409=VECTOR('',#26549,1.);
#7410=VECTOR('',#26552,1.);
#7411=VECTOR('',#26553,1.);
#7412=VECTOR('',#26554,1.);
#7413=VECTOR('',#26557,1.);
#7414=VECTOR('',#26558,1.);
#7415=VECTOR('',#26567,1.);
#7416=VECTOR('',#26568,1.);
#7417=VECTOR('',#26569,1.);
#7418=VECTOR('',#26570,1.);
#7419=VECTOR('',#26573,1.);
#7420=VECTOR('',#26574,1.);
#7421=VECTOR('',#26575,1.);
#7422=VECTOR('',#26578,1.);
#7423=VECTOR('',#26579,1.);
#7424=VECTOR('',#26580,1.);
#7425=VECTOR('',#26583,1.);
#7426=VECTOR('',#26584,1.);
#7427=VECTOR('',#26593,1.);
#7428=VECTOR('',#26594,1.);
#7429=VECTOR('',#26595,1.);
#7430=VECTOR('',#26596,1.);
#7431=VECTOR('',#26599,1.);
#7432=VECTOR('',#26600,1.);
#7433=VECTOR('',#26601,1.);
#7434=VECTOR('',#26604,1.);
#7435=VECTOR('',#26605,1.);
#7436=VECTOR('',#26606,1.);
#7437=VECTOR('',#26609,1.);
#7438=VECTOR('',#26610,1.);
#7439=VECTOR('',#26619,0.5);
#7440=VECTOR('',#26622,1.);
#7441=VECTOR('',#26627,0.5);
#7442=VECTOR('',#26630,1.);
#7443=VECTOR('',#26637,0.164999999999999);
#7444=VECTOR('',#26644,0.164999999999999);
#7445=VECTOR('',#26651,0.165);
#7446=VECTOR('',#26658,0.164999999999999);
#7447=VECTOR('',#26665,0.5);
#7448=VECTOR('',#26676,1.);
#7449=VECTOR('',#26687,0.5);
#7450=VECTOR('',#26698,1.);
#7451=VECTOR('',#26707,1.);
#7452=VECTOR('',#26708,1.);
#7453=VECTOR('',#26709,1.);
#7454=VECTOR('',#26710,1.);
#7455=VECTOR('',#26711,1.);
#7456=VECTOR('',#26712,1.);
#7457=VECTOR('',#26717,0.274999999999999);
#7458=VECTOR('',#26722,0.275);
#7459=VECTOR('',#26727,0.275);
#7460=VECTOR('',#26732,0.274999999999999);
#7461=VECTOR('',#26735,1.);
#7462=VECTOR('',#26736,1.);
#7463=VECTOR('',#26737,1.);
#7464=VECTOR('',#26740,1.);
#7465=VECTOR('',#26741,1.);
#7466=VECTOR('',#26744,1.);
#7467=VECTOR('',#26745,1.);
#7468=VECTOR('',#26748,1.);
#7469=VECTOR('',#26757,0.165);
#7470=VECTOR('',#26764,0.165);
#7471=VECTOR('',#26771,0.165);
#7472=VECTOR('',#26778,1.6);
#7473=VECTOR('',#26787,1.4);
#7474=VECTOR('',#26794,0.21);
#7475=VECTOR('',#26803,0.21);
#7476=VECTOR('',#26810,1.);
#7477=VECTOR('',#26811,1.);
#7478=VECTOR('',#26812,1.);
#7479=VECTOR('',#26813,1.);
#7480=VECTOR('',#26816,1.);
#7481=VECTOR('',#26817,1.);
#7482=VECTOR('',#26818,1.);
#7483=VECTOR('',#26821,1.);
#7484=VECTOR('',#26822,1.);
#7485=VECTOR('',#26823,1.);
#7486=VECTOR('',#26826,1.);
#7487=VECTOR('',#26827,1.);
#7488=VECTOR('',#26838,0.225);
#7489=VECTOR('',#26845,0.225);
#7490=VECTOR('',#26852,0.225);
#7491=VECTOR('',#26859,1.59);
#7492=VECTOR('',#26868,1.2);
#7493=VECTOR('',#26875,2.4);
#7494=VECTOR('',#26888,0.165);
#7495=VECTOR('',#26895,0.165);
#7496=VECTOR('',#26902,0.165);
#7497=VECTOR('',#26909,2.35);
#7498=VECTOR('',#26920,2.15);
#7499=VECTOR('',#26925,0.25);
#7500=VECTOR('',#26934,0.25);
#7501=VECTOR('',#26941,1.);
#7502=VECTOR('',#26942,1.);
#7503=VECTOR('',#26943,1.);
#7504=VECTOR('',#26944,1.);
#7505=VECTOR('',#26947,1.);
#7506=VECTOR('',#26948,1.);
#7507=VECTOR('',#26949,1.);
#7508=VECTOR('',#26952,1.);
#7509=VECTOR('',#26953,1.);
#7510=VECTOR('',#26954,1.);
#7511=VECTOR('',#26957,1.);
#7512=VECTOR('',#26958,1.);
#7513=VECTOR('',#26969,0.225);
#7514=VECTOR('',#26976,0.225);
#7515=VECTOR('',#26983,0.225);
#7516=VECTOR('',#26988,1.);
#7517=VECTOR('',#26989,1.);
#7518=VECTOR('',#26990,1.);
#7519=VECTOR('',#26991,1.);
#7520=VECTOR('',#27004,2.34);
#7521=VECTOR('',#27015,1.8);
#7522=VECTOR('',#27024,0.475);
#7523=VECTOR('',#27035,0.275);
#7524=VECTOR('',#27038,1.);
#7525=VECTOR('',#27039,1.);
#7526=VECTOR('',#27040,1.);
#7527=VECTOR('',#27041,1.);
#7528=VECTOR('',#27044,1.);
#7529=VECTOR('',#27045,1.);
#7530=VECTOR('',#27046,1.);
#7531=VECTOR('',#27049,1.);
#7532=VECTOR('',#27050,1.);
#7533=VECTOR('',#27051,1.);
#7534=VECTOR('',#27054,1.);
#7535=VECTOR('',#27055,1.);
#7536=VECTOR('',#27066,0.475000000000001);
#7537=VECTOR('',#27077,0.274999999999999);
#7538=VECTOR('',#27080,1.);
#7539=VECTOR('',#27081,1.);
#7540=VECTOR('',#27082,1.);
#7541=VECTOR('',#27083,1.);
#7542=VECTOR('',#27086,1.);
#7543=VECTOR('',#27087,1.);
#7544=VECTOR('',#27088,1.);
#7545=VECTOR('',#27091,1.);
#7546=VECTOR('',#27092,1.);
#7547=VECTOR('',#27093,1.);
#7548=VECTOR('',#27096,1.);
#7549=VECTOR('',#27097,1.);
#7550=VECTOR('',#27108,0.375);
#7551=VECTOR('',#27119,0.375);
#7552=VECTOR('',#27130,0.375);
#7553=VECTOR('',#27141,0.375);
#7554=VECTOR('',#27152,0.225);
#7555=VECTOR('',#27157,0.225);
#7556=VECTOR('',#27162,0.225);
#7557=VECTOR('',#27167,0.225000000000001);
#7558=VECTOR('',#27170,1.);
#7559=VECTOR('',#27171,1.);
#7560=VECTOR('',#27172,1.);
#7561=VECTOR('',#27173,1.);
#7562=VECTOR('',#27176,1.);
#7563=VECTOR('',#27177,1.);
#7564=VECTOR('',#27178,1.);
#7565=VECTOR('',#27181,1.);
#7566=VECTOR('',#27182,1.);
#7567=VECTOR('',#27183,1.);
#7568=VECTOR('',#27186,1.);
#7569=VECTOR('',#27187,1.);
#7570=VECTOR('',#27188,1.);
#7571=VECTOR('',#27191,1.);
#7572=VECTOR('',#27192,1.);
#7573=VECTOR('',#27193,1.);
#7574=VECTOR('',#27196,1.);
#7575=VECTOR('',#27197,1.);
#7576=VECTOR('',#27198,1.);
#7577=VECTOR('',#27201,1.);
#7578=VECTOR('',#27202,1.);
#7579=VECTOR('',#27203,1.);
#7580=VECTOR('',#27206,1.);
#7581=VECTOR('',#27207,1.);
#7582=VECTOR('',#27208,1.);
#7583=VECTOR('',#27211,1.);
#7584=VECTOR('',#27212,1.);
#7585=VECTOR('',#27213,1.);
#7586=VECTOR('',#27216,1.);
#7587=VECTOR('',#27217,1.);
#7588=VECTOR('',#27218,1.);
#7589=VECTOR('',#27221,1.);
#7590=VECTOR('',#27222,1.);
#7591=VECTOR('',#27223,1.);
#7592=VECTOR('',#27226,1.);
#7593=VECTOR('',#27227,1.);
#7594=VECTOR('',#27250,1.070235);
#7595=VECTOR('',#27257,0.6);
#7596=VECTOR('',#27262,0.63);
#7597=VECTOR('',#27271,1.070235);
#7598=VECTOR('',#27278,0.63);
#7599=VECTOR('',#27297,1.129765);
#7600=VECTOR('',#27308,1.57);
#7601=VECTOR('',#27313,1.6);
#7602=VECTOR('',#27318,1.57);
#7603=VECTOR('',#27323,1.129765);
#7604=VECTOR('',#27370,1.123812);
#7605=VECTOR('',#27439,1.076188);
#7606=VECTOR('',#27468,1.119765);
#7607=VECTOR('',#27475,1.085235);
#7608=VECTOR('',#27486,1.119765);
#7609=VECTOR('',#27493,1.085235);
#7610=VECTOR('',#27522,1.63531);
#7611=VECTOR('',#27529,1.);
#7612=VECTOR('',#27534,1.05);
#7613=VECTOR('',#27543,1.63531);
#7614=VECTOR('',#27550,1.05);
#7615=VECTOR('',#27569,1.71469);
#7616=VECTOR('',#27580,2.3);
#7617=VECTOR('',#27585,2.35);
#7618=VECTOR('',#27590,2.3);
#7619=VECTOR('',#27595,1.71469);
#7620=VECTOR('',#27646,1.706752);
#7621=VECTOR('',#27723,1.643248);
#7622=VECTOR('',#27752,1.70469);
#7623=VECTOR('',#27759,1.65031);
#7624=VECTOR('',#27770,1.70469);
#7625=VECTOR('',#27777,1.65031);
#7626=VECTOR('',#27796,0.275);
#7627=VECTOR('',#27803,0.275);
#7628=VECTOR('',#27810,0.275);
#7629=VECTOR('',#27817,0.275);
#7630=VECTOR('',#27822,1.);
#7631=VECTOR('',#27823,1.);
#7632=VECTOR('',#27824,1.);
#7633=VECTOR('',#27825,1.);
#7634=VECTOR('',#27828,1.);
#7635=VECTOR('',#27829,1.);
#7636=VECTOR('',#27830,1.);
#7637=VECTOR('',#27833,1.);
#7638=VECTOR('',#27834,1.);
#7639=VECTOR('',#27835,1.);
#7640=VECTOR('',#27838,1.);
#7641=VECTOR('',#27839,1.);
#7642=VECTOR('',#27850,0.210000000000001);
#7643=VECTOR('',#27857,0.210000000000001);
#7644=VECTOR('',#27864,0.210000000000001);
#7645=VECTOR('',#27871,0.210000000000001);
#7646=VECTOR('',#27878,0.275);
#7647=VECTOR('',#27885,0.275);
#7648=VECTOR('',#27892,0.275);
#7649=VECTOR('',#27899,0.275);
#7650=VECTOR('',#27906,0.275);
#7651=VECTOR('',#27913,0.275);
#7652=VECTOR('',#27920,0.275);
#7653=VECTOR('',#27927,0.275);
#7654=VECTOR('',#27932,1.);
#7655=VECTOR('',#27933,1.);
#7656=VECTOR('',#27934,1.);
#7657=VECTOR('',#27935,1.);
#7658=VECTOR('',#27938,1.);
#7659=VECTOR('',#27939,1.);
#7660=VECTOR('',#27940,1.);
#7661=VECTOR('',#27943,1.);
#7662=VECTOR('',#27944,1.);
#7663=VECTOR('',#27945,1.);
#7664=VECTOR('',#27948,1.);
#7665=VECTOR('',#27949,1.);
#7666=VECTOR('',#27960,0.210000000000001);
#7667=VECTOR('',#27969,0.210000000000001);
#7668=VECTOR('',#27978,0.210000000000001);
#7669=VECTOR('',#27987,0.210000000000001);
#7670=VECTOR('',#27996,0.165);
#7671=VECTOR('',#28005,0.165);
#7672=VECTOR('',#28014,0.165);
#7673=VECTOR('',#28023,1.11);
#7674=VECTOR('',#28028,1.);
#7675=VECTOR('',#28029,1.);
#7676=VECTOR('',#28030,1.);
#7677=VECTOR('',#28031,1.);
#7678=VECTOR('',#28034,1.);
#7679=VECTOR('',#28035,1.);
#7680=VECTOR('',#28036,1.);
#7681=VECTOR('',#28039,1.);
#7682=VECTOR('',#28040,1.);
#7683=VECTOR('',#28041,1.);
#7684=VECTOR('',#28044,1.);
#7685=VECTOR('',#28045,1.);
#7686=VECTOR('',#28056,1.);
#7687=VECTOR('',#28061,1.);
#7688=VECTOR('',#28064,0.21);
#7689=VECTOR('',#28069,1.);
#7690=VECTOR('',#28072,1.);
#7691=VECTOR('',#28077,1.);
#7692=VECTOR('',#28080,0.21);
#7693=VECTOR('',#28085,1.);
#7694=VECTOR('',#28088,1.);
#7695=VECTOR('',#28093,1.);
#7696=VECTOR('',#28096,0.21);
#7697=VECTOR('',#28101,1.);
#7698=VECTOR('',#28104,1.);
#7699=VECTOR('',#28109,1.);
#7700=VECTOR('',#28112,0.21);
#7701=VECTOR('',#28117,1.);
#7702=VECTOR('',#28120,1.);
#7703=VECTOR('',#28121,1.);
#7704=VECTOR('',#28122,1.);
#7705=VECTOR('',#28123,1.);
#7706=VECTOR('',#28124,1.);
#7707=VECTOR('',#28125,1.);
#7708=VECTOR('',#28128,1.);
#7709=VECTOR('',#28129,1.);
#7710=VECTOR('',#28130,1.);
#7711=VECTOR('',#28131,1.);
#7712=VECTOR('',#28132,1.);
#7713=VECTOR('',#28133,1.);
#7714=VECTOR('',#28136,1.);
#7715=VECTOR('',#28137,1.);
#7716=VECTOR('',#28138,1.);
#7717=VECTOR('',#28139,1.);
#7718=VECTOR('',#28140,1.);
#7719=VECTOR('',#28141,1.);
#7720=VECTOR('',#28142,1.);
#7721=VECTOR('',#28143,1.);
#7722=VECTOR('',#28144,1.);
#7723=VECTOR('',#28145,1.);
#7724=VECTOR('',#28148,1.);
#7725=VECTOR('',#28149,1.);
#7726=VECTOR('',#28152,1.);
#7727=VECTOR('',#28153,1.);
#7728=VECTOR('',#28156,1.);
#7729=VECTOR('',#28157,1.);
#7730=VECTOR('',#28160,1.);
#7731=VECTOR('',#28161,1.);
#7732=VECTOR('',#28164,1.);
#7733=VECTOR('',#28167,1.);
#7734=VECTOR('',#28168,1.);
#7735=VECTOR('',#28171,1.);
#7736=VECTOR('',#28172,1.);
#7737=VECTOR('',#28175,1.);
#7738=VECTOR('',#28176,1.);
#7739=VECTOR('',#28179,1.);
#7740=VECTOR('',#28180,1.);
#7741=VECTOR('',#28183,1.);
#7742=VECTOR('',#28190,1.);
#7743=VECTOR('',#28191,1.);
#7744=VECTOR('',#28192,1.);
#7745=VECTOR('',#28193,1.);
#7746=VECTOR('',#28196,1.);
#7747=VECTOR('',#28197,1.);
#7748=VECTOR('',#28198,1.);
#7749=VECTOR('',#28201,1.);
#7750=VECTOR('',#28202,1.);
#7751=VECTOR('',#28203,1.);
#7752=VECTOR('',#28206,1.);
#7753=VECTOR('',#28207,1.);
#7754=VECTOR('',#28208,1.);
#7755=VECTOR('',#28211,1.);
#7756=VECTOR('',#28212,1.);
#7757=VECTOR('',#28213,1.);
#7758=VECTOR('',#28216,1.);
#7759=VECTOR('',#28217,1.);
#7760=VECTOR('',#28218,1.);
#7761=VECTOR('',#28221,1.);
#7762=VECTOR('',#28222,1.);
#7763=VECTOR('',#28223,1.);
#7764=VECTOR('',#28226,1.);
#7765=VECTOR('',#28227,1.);
#7766=VECTOR('',#28236,1.);
#7767=VECTOR('',#28237,1.);
#7768=VECTOR('',#28238,1.);
#7769=VECTOR('',#28239,1.);
#7770=VECTOR('',#28242,1.);
#7771=VECTOR('',#28243,1.);
#7772=VECTOR('',#28244,1.);
#7773=VECTOR('',#28247,1.);
#7774=VECTOR('',#28248,1.);
#7775=VECTOR('',#28249,1.);
#7776=VECTOR('',#28252,1.);
#7777=VECTOR('',#28253,1.);
#7778=VECTOR('',#28254,1.);
#7779=VECTOR('',#28257,1.);
#7780=VECTOR('',#28258,1.);
#7781=VECTOR('',#28259,1.);
#7782=VECTOR('',#28262,1.);
#7783=VECTOR('',#28263,1.);
#7784=VECTOR('',#28264,1.);
#7785=VECTOR('',#28267,1.);
#7786=VECTOR('',#28268,1.);
#7787=VECTOR('',#28269,1.);
#7788=VECTOR('',#28272,1.);
#7789=VECTOR('',#28273,1.);
#7790=VECTOR('',#28290,0.275);
#7791=VECTOR('',#28295,0.265);
#7792=VECTOR('',#28304,0.5);
#7793=VECTOR('',#28313,1.);
#7794=VECTOR('',#28314,1.);
#7795=VECTOR('',#28315,1.);
#7796=VECTOR('',#28316,1.);
#7797=VECTOR('',#28319,1.);
#7798=VECTOR('',#28320,1.);
#7799=VECTOR('',#28321,1.);
#7800=VECTOR('',#28324,1.);
#7801=VECTOR('',#28325,1.);
#7802=VECTOR('',#28326,1.);
#7803=VECTOR('',#28329,1.);
#7804=VECTOR('',#28330,1.);
#7805=VECTOR('',#28331,1.);
#7806=VECTOR('',#28334,1.);
#7807=VECTOR('',#28335,1.);
#7808=VECTOR('',#28336,1.);
#7809=VECTOR('',#28339,1.);
#7810=VECTOR('',#28340,1.);
#7811=VECTOR('',#28353,0.25);
#7812=VECTOR('',#28366,0.4);
#7813=VECTOR('',#28371,0.425);
#7814=VECTOR('',#28376,0.41);
#7815=VECTOR('',#28385,0.26);
#7816=VECTOR('',#28388,0.25);
#7817=VECTOR('',#28393,0.45);
#7818=VECTOR('',#28398,0.45);
#7819=VECTOR('',#28401,0.45);
#7820=VECTOR('',#28404,0.45);
#7821=VECTOR('',#28407,0.45);
#7822=VECTOR('',#28410,0.45);
#7823=VECTOR('',#28413,0.45);
#7824=VECTOR('',#28416,0.45);
#7825=VECTOR('',#28419,0.45);
#7826=VECTOR('',#28424,0.625);
#7827=VECTOR('',#28429,0.625);
#7828=VECTOR('',#28432,0.625);
#7829=VECTOR('',#28435,0.625);
#7830=VECTOR('',#28438,0.625);
#7831=VECTOR('',#28441,0.625);
#7832=VECTOR('',#28444,0.625);
#7833=VECTOR('',#28447,0.625);
#7834=VECTOR('',#28450,0.625);
#7835=VECTOR('',#28457,1.);
#7836=VECTOR('',#28472,0.225);
#7837=VECTOR('',#28477,0.225);
#7838=VECTOR('',#28482,0.225);
#7839=VECTOR('',#28485,1.);
#7840=VECTOR('',#28486,1.);
#7841=VECTOR('',#28487,1.);
#7842=VECTOR('',#28500,1.1);
#7843=VECTOR('',#28515,0.325);
#7844=VECTOR('',#28520,0.35);
#7845=VECTOR('',#28525,0.335);
#7846=VECTOR('',#28534,0.21);
#7847=VECTOR('',#28539,0.2);
#7848=VECTOR('',#28544,0.18);
#7849=VECTOR('',#28549,1.);
#7850=VECTOR('',#28550,1.);
#7851=VECTOR('',#28551,1.);
#7852=VECTOR('',#28552,1.);
#7853=VECTOR('',#28555,1.);
#7854=VECTOR('',#28556,1.);
#7855=VECTOR('',#28557,1.);
#7856=VECTOR('',#28560,1.);
#7857=VECTOR('',#28561,1.);
#7858=VECTOR('',#28562,1.);
#7859=VECTOR('',#28565,1.);
#7860=VECTOR('',#28566,1.);
#7861=VECTOR('',#28567,1.);
#7862=VECTOR('',#28570,1.);
#7863=VECTOR('',#28571,1.);
#7864=VECTOR('',#28572,1.);
#7865=VECTOR('',#28575,1.);
#7866=VECTOR('',#28576,1.);
#7867=VECTOR('',#28591,0.4);
#7868=VECTOR('',#28596,0.425);
#7869=VECTOR('',#28601,0.41);
#7870=VECTOR('',#28610,0.26);
#7871=VECTOR('',#28615,0.25);
#7872=VECTOR('',#28620,0.225);
#7873=VECTOR('',#28625,1.);
#7874=VECTOR('',#28626,1.);
#7875=VECTOR('',#28627,1.);
#7876=VECTOR('',#28628,1.);
#7877=VECTOR('',#28631,1.);
#7878=VECTOR('',#28632,1.);
#7879=VECTOR('',#28633,1.);
#7880=VECTOR('',#28636,1.);
#7881=VECTOR('',#28637,1.);
#7882=VECTOR('',#28638,1.);
#7883=VECTOR('',#28641,1.);
#7884=VECTOR('',#28642,1.);
#7885=VECTOR('',#28643,1.);
#7886=VECTOR('',#28646,1.);
#7887=VECTOR('',#28647,1.);
#7888=VECTOR('',#28648,1.);
#7889=VECTOR('',#28651,1.);
#7890=VECTOR('',#28652,1.);
#7891=VECTOR('',#28703,0.6);
#7892=VECTOR('',#28708,0.6);
#7893=VECTOR('',#28711,0.6);
#7894=VECTOR('',#28714,0.6);
#7895=VECTOR('',#28717,0.6);
#7896=VECTOR('',#28720,0.6);
#7897=VECTOR('',#28723,0.6);
#7898=VECTOR('',#28726,0.6);
#7899=VECTOR('',#28729,0.6);
#7900=VECTOR('',#28732,0.6);
#7901=VECTOR('',#28735,0.6);
#7902=VECTOR('',#28738,0.6);
#7903=VECTOR('',#28741,0.6);
#7904=VECTOR('',#28744,0.6);
#7905=VECTOR('',#28747,0.6);
#7906=VECTOR('',#28750,0.6);
#7907=VECTOR('',#28753,0.6);
#7908=VECTOR('',#28756,0.6);
#7909=VECTOR('',#28759,0.6);
#7910=VECTOR('',#28762,0.6);
#7911=VECTOR('',#28765,0.6);
#7912=VECTOR('',#28768,0.6);
#7913=VECTOR('',#28771,0.6);
#7914=VECTOR('',#28774,0.6);
#7915=VECTOR('',#28777,0.6);
#7916=VECTOR('',#28780,0.6);
#7917=VECTOR('',#28783,0.6);
#7918=VECTOR('',#28786,0.6);
#7919=VECTOR('',#28789,0.6);
#7920=VECTOR('',#28792,0.6);
#7921=VECTOR('',#28795,0.6);
#7922=VECTOR('',#28798,0.6);
#7923=VECTOR('',#28801,0.6);
#7924=VECTOR('',#28804,0.6);
#7925=VECTOR('',#28807,0.6);
#7926=VECTOR('',#28810,0.6);
#7927=VECTOR('',#28813,0.6);
#7928=VECTOR('',#28816,0.6);
#7929=VECTOR('',#28819,0.6);
#7930=VECTOR('',#28822,0.6);
#7931=VECTOR('',#28825,0.6);
#7932=VECTOR('',#28828,0.6);
#7933=VECTOR('',#28831,0.6);
#7934=VECTOR('',#28834,0.6);
#7935=VECTOR('',#28837,0.6);
#7936=VECTOR('',#28840,0.6);
#7937=VECTOR('',#28843,0.6);
#7938=VECTOR('',#28846,0.6);
#7939=VECTOR('',#28849,0.6);
#7940=VECTOR('',#28852,0.6);
#7941=VECTOR('',#28855,0.6);
#7942=VECTOR('',#28858,0.6);
#7943=VECTOR('',#28861,0.6);
#7944=VECTOR('',#28864,0.6);
#7945=VECTOR('',#28867,0.6);
#7946=VECTOR('',#28870,0.6);
#7947=VECTOR('',#28873,0.6);
#7948=VECTOR('',#28876,0.6);
#7949=VECTOR('',#28879,0.6);
#7950=VECTOR('',#28882,0.6);
#7951=VECTOR('',#28885,0.6);
#7952=VECTOR('',#28888,0.6);
#7953=VECTOR('',#28891,0.6);
#7954=VECTOR('',#28894,0.415875);
#7955=VECTOR('',#28899,0.415875);
#7956=VECTOR('',#28904,0.415875);
#7957=VECTOR('',#28907,0.415875);
#7958=VECTOR('',#28910,0.415875);
#7959=VECTOR('',#28913,0.415875);
#7960=VECTOR('',#28916,0.415875);
#7961=VECTOR('',#28919,0.415875);
#7962=VECTOR('',#28922,0.415875);
#7963=VECTOR('',#28925,0.415875);
#7964=VECTOR('',#28928,0.415875);
#7965=VECTOR('',#28931,0.415875);
#7966=VECTOR('',#28934,0.415875);
#7967=VECTOR('',#28937,0.415875);
#7968=VECTOR('',#28940,0.415875);
#7969=VECTOR('',#28943,0.415875);
#7970=VECTOR('',#28946,0.415875);
#7971=VECTOR('',#28949,0.415875);
#7972=VECTOR('',#28952,0.415875);
#7973=VECTOR('',#28955,0.415875);
#7974=VECTOR('',#28958,0.415875);
#7975=VECTOR('',#28961,0.415875);
#7976=VECTOR('',#28964,0.415875);
#7977=VECTOR('',#28967,0.415875);
#7978=VECTOR('',#28970,0.415875);
#7979=VECTOR('',#28973,0.415875);
#7980=VECTOR('',#28976,0.415875);
#7981=VECTOR('',#28979,0.415875);
#7982=VECTOR('',#28982,0.415875);
#7983=VECTOR('',#28985,0.415875);
#7984=VECTOR('',#28988,0.415875);
#7985=VECTOR('',#28991,0.415875);
#7986=VECTOR('',#28994,0.415875);
#7987=VECTOR('',#28997,0.415875);
#7988=VECTOR('',#29000,0.415875);
#7989=VECTOR('',#29003,0.415875);
#7990=VECTOR('',#29006,0.415875);
#7991=VECTOR('',#29009,0.415875);
#7992=VECTOR('',#29012,0.415875);
#7993=VECTOR('',#29015,0.415875);
#7994=VECTOR('',#29018,0.415875);
#7995=VECTOR('',#29021,0.415875);
#7996=VECTOR('',#29024,0.415875);
#7997=VECTOR('',#29027,0.415875);
#7998=VECTOR('',#29030,0.415875);
#7999=VECTOR('',#29033,0.415875);
#8000=VECTOR('',#29036,0.415875);
#8001=VECTOR('',#29039,0.415875);
#8002=VECTOR('',#29042,0.415875);
#8003=VECTOR('',#29045,0.415875);
#8004=VECTOR('',#29048,0.415875);
#8005=VECTOR('',#29051,0.415875);
#8006=VECTOR('',#29054,0.415875);
#8007=VECTOR('',#29057,0.415875);
#8008=VECTOR('',#29060,0.415875);
#8009=VECTOR('',#29063,0.415875);
#8010=VECTOR('',#29066,0.415875);
#8011=VECTOR('',#29069,0.415875);
#8012=VECTOR('',#29072,0.415875);
#8013=VECTOR('',#29075,0.415875);
#8014=VECTOR('',#29078,0.415875);
#8015=VECTOR('',#29081,0.415875);
#8016=VECTOR('',#29084,0.415875);
#8017=VECTOR('',#29093,0.6);
#8018=VECTOR('',#29102,1.);
#8019=VECTOR('',#29103,1.);
#8020=VECTOR('',#29104,1.);
#8021=VECTOR('',#29105,1.);
#8022=VECTOR('',#29110,1.);
#8023=VECTOR('',#29111,1.);
#8024=VECTOR('',#29114,1.);
#8025=VECTOR('',#29115,1.);
#8026=VECTOR('',#29118,1.);
#8027=VECTOR('',#29119,1.);
#8028=VECTOR('',#29128,1.);
#8029=VECTOR('',#29143,1.35);
#8030=VECTOR('',#29154,1.01);
#8031=VECTOR('',#29161,1.35);
#8032=VECTOR('',#29172,1.);
#8033=VECTOR('',#29179,0.210000000000001);
#8034=VECTOR('',#29182,1.);
#8035=VECTOR('',#29187,1.005);
#8036=VECTOR('',#29194,1.5);
#8037=VECTOR('',#29207,0.25);
#8038=VECTOR('',#29212,1.);
#8039=VECTOR('',#29219,0.210000000000001);
#8040=VECTOR('',#29222,1.);
#8041=VECTOR('',#29225,1.);
#8042=VECTOR('',#29226,1.);
#8043=VECTOR('',#29227,1.);
#8044=VECTOR('',#29228,1.);
#8045=VECTOR('',#29229,1.);
#8046=VECTOR('',#29230,1.);
#8047=VECTOR('',#29233,1.);
#8048=VECTOR('',#29234,1.);
#8049=VECTOR('',#29235,1.);
#8050=VECTOR('',#29238,1.);
#8051=VECTOR('',#29239,1.);
#8052=VECTOR('',#29240,1.);
#8053=VECTOR('',#29241,1.);
#8054=VECTOR('',#29242,1.);
#8055=VECTOR('',#29257,3.5);
#8056=VECTOR('',#29274,0.33);
#8057=VECTOR('',#29281,0.4);
#8058=VECTOR('',#29294,0.405);
#8059=VECTOR('',#29301,0.9);
#8060=VECTOR('',#29312,1.);
#8061=VECTOR('',#29313,1.);
#8062=VECTOR('',#29314,1.);
#8063=VECTOR('',#29315,1.);
#8064=VECTOR('',#29316,1.);
#8065=VECTOR('',#29317,1.);
#8066=VECTOR('',#29318,1.);
#8067=VECTOR('',#29319,1.);
#8068=VECTOR('',#29322,1.);
#8069=VECTOR('',#29323,1.);
#8070=VECTOR('',#29324,1.);
#8071=VECTOR('',#29327,1.);
#8072=VECTOR('',#29328,1.);
#8073=VECTOR('',#29331,1.);
#8074=VECTOR('',#29332,1.);
#8075=VECTOR('',#29335,1.);
#8076=VECTOR('',#29336,1.);
#8077=VECTOR('',#29339,1.);
#8078=VECTOR('',#29340,1.);
#8079=VECTOR('',#29341,1.);
#8080=VECTOR('',#29342,1.);
#8081=VECTOR('',#29345,1.);
#8082=VECTOR('',#29348,1.);
#8083=VECTOR('',#29351,1.);
#8084=VECTOR('',#29358,1.);
#8085=VECTOR('',#29359,1.);
#8086=VECTOR('',#29360,1.);
#8087=VECTOR('',#29361,1.);
#8088=VECTOR('',#29364,1.);
#8089=VECTOR('',#29365,1.);
#8090=VECTOR('',#29366,1.);
#8091=VECTOR('',#29369,1.);
#8092=VECTOR('',#29370,1.);
#8093=VECTOR('',#29371,1.);
#8094=VECTOR('',#29374,1.);
#8095=VECTOR('',#29375,1.);
#8096=VECTOR('',#29376,1.);
#8097=VECTOR('',#29379,1.);
#8098=VECTOR('',#29380,1.);
#8099=VECTOR('',#29381,1.);
#8100=VECTOR('',#29384,1.);
#8101=VECTOR('',#29385,1.);
#8102=VECTOR('',#29396,0.235);
#8103=VECTOR('',#29401,0.25);
#8104=VECTOR('',#29406,0.2125);
#8105=VECTOR('',#29415,0.32);
#8106=VECTOR('',#29422,0.6);
#8107=VECTOR('',#29439,0.475);
#8108=VECTOR('',#29444,0.5);
#8109=VECTOR('',#29449,0.485);
#8110=VECTOR('',#29458,0.31);
#8111=VECTOR('',#29463,0.3);
#8112=VECTOR('',#29468,0.27);
#8113=VECTOR('',#29473,1.);
#8114=VECTOR('',#29474,1.);
#8115=VECTOR('',#29475,1.);
#8116=VECTOR('',#29476,1.);
#8117=VECTOR('',#29479,1.);
#8118=VECTOR('',#29480,1.);
#8119=VECTOR('',#29481,1.);
#8120=VECTOR('',#29484,1.);
#8121=VECTOR('',#29485,1.);
#8122=VECTOR('',#29486,1.);
#8123=VECTOR('',#29489,1.);
#8124=VECTOR('',#29490,1.);
#8125=VECTOR('',#29491,1.);
#8126=VECTOR('',#29494,1.);
#8127=VECTOR('',#29495,1.);
#8128=VECTOR('',#29496,1.);
#8129=VECTOR('',#29499,1.);
#8130=VECTOR('',#29500,1.);
#8131=VECTOR('',#29609,0.550000000000001);
#8132=VECTOR('',#29618,0.550000000000001);
#8133=VECTOR('',#29627,0.550000000000001);
#8134=VECTOR('',#29636,0.550000000000001);
#8135=VECTOR('',#29645,0.550000000000001);
#8136=VECTOR('',#29654,0.550000000000001);
#8137=VECTOR('',#29663,0.550000000000001);
#8138=VECTOR('',#29672,0.550000000000001);
#8139=VECTOR('',#29681,0.5);
#8140=VECTOR('',#29692,0.5);
#8141=VECTOR('',#29703,0.5);
#8142=VECTOR('',#29714,0.5);
#8143=VECTOR('',#29725,0.275);
#8144=VECTOR('',#29730,0.274999999999999);
#8145=VECTOR('',#29735,0.275);
#8146=VECTOR('',#29740,0.274999999999999);
#8147=VECTOR('',#29745,0.210000000000001);
#8148=VECTOR('',#29752,0.21);
#8149=VECTOR('',#29759,0.329999999999998);
#8150=VECTOR('',#29766,0.329999999999998);
#8151=VECTOR('',#29773,0.275);
#8152=VECTOR('',#29780,0.275);
#8153=VECTOR('',#29787,0.210000000000001);
#8154=VECTOR('',#29794,0.21);
#8155=VECTOR('',#29801,0.21);
#8156=VECTOR('',#29808,0.210000000000001);
#8157=VECTOR('',#29813,1.);
#8158=VECTOR('',#29814,1.);
#8159=VECTOR('',#29815,1.);
#8160=VECTOR('',#29816,1.);
#8161=VECTOR('',#29819,1.);
#8162=VECTOR('',#29820,1.);
#8163=VECTOR('',#29821,1.);
#8164=VECTOR('',#29824,1.);
#8165=VECTOR('',#29825,1.);
#8166=VECTOR('',#29826,1.);
#8167=VECTOR('',#29829,1.);
#8168=VECTOR('',#29830,1.);
#8169=VECTOR('',#29839,0.5);
#8170=VECTOR('',#29842,1.);
#8171=VECTOR('',#29847,0.5);
#8172=VECTOR('',#29850,1.);
#8173=VECTOR('',#29857,0.164999999999999);
#8174=VECTOR('',#29864,0.164999999999999);
#8175=VECTOR('',#29871,0.165);
#8176=VECTOR('',#29878,0.164999999999999);
#8177=VECTOR('',#29885,0.5);
#8178=VECTOR('',#29896,1.);
#8179=VECTOR('',#29907,0.5);
#8180=VECTOR('',#29918,1.);
#8181=VECTOR('',#29927,1.);
#8182=VECTOR('',#29928,1.);
#8183=VECTOR('',#29929,1.);
#8184=VECTOR('',#29930,1.);
#8185=VECTOR('',#29931,1.);
#8186=VECTOR('',#29932,1.);
#8187=VECTOR('',#29937,0.274999999999999);
#8188=VECTOR('',#29942,0.275);
#8189=VECTOR('',#29947,0.275);
#8190=VECTOR('',#29952,0.274999999999999);
#8191=VECTOR('',#29955,1.);
#8192=VECTOR('',#29956,1.);
#8193=VECTOR('',#29957,1.);
#8194=VECTOR('',#29960,1.);
#8195=VECTOR('',#29961,1.);
#8196=VECTOR('',#29964,1.);
#8197=VECTOR('',#29965,1.);
#8198=VECTOR('',#29968,1.);
#8199=VECTOR('',#29977,0.165);
#8200=VECTOR('',#29984,0.165);
#8201=VECTOR('',#29991,0.165);
#8202=VECTOR('',#29998,1.6);
#8203=VECTOR('',#30007,1.4);
#8204=VECTOR('',#30014,0.21);
#8205=VECTOR('',#30023,0.21);
#8206=VECTOR('',#30030,1.);
#8207=VECTOR('',#30031,1.);
#8208=VECTOR('',#30032,1.);
#8209=VECTOR('',#30033,1.);
#8210=VECTOR('',#30036,1.);
#8211=VECTOR('',#30037,1.);
#8212=VECTOR('',#30038,1.);
#8213=VECTOR('',#30041,1.);
#8214=VECTOR('',#30042,1.);
#8215=VECTOR('',#30043,1.);
#8216=VECTOR('',#30046,1.);
#8217=VECTOR('',#30047,1.);
#8218=VECTOR('',#30058,0.225);
#8219=VECTOR('',#30065,0.225);
#8220=VECTOR('',#30072,0.225);
#8221=VECTOR('',#30079,1.59);
#8222=VECTOR('',#30088,1.2);
#8223=VECTOR('',#30095,2.4);
#8224=VECTOR('',#30108,0.165);
#8225=VECTOR('',#30115,0.165);
#8226=VECTOR('',#30122,0.165);
#8227=VECTOR('',#30129,2.35);
#8228=VECTOR('',#30140,2.15);
#8229=VECTOR('',#30145,0.25);
#8230=VECTOR('',#30154,0.25);
#8231=VECTOR('',#30161,1.);
#8232=VECTOR('',#30162,1.);
#8233=VECTOR('',#30163,1.);
#8234=VECTOR('',#30164,1.);
#8235=VECTOR('',#30167,1.);
#8236=VECTOR('',#30168,1.);
#8237=VECTOR('',#30169,1.);
#8238=VECTOR('',#30172,1.);
#8239=VECTOR('',#30173,1.);
#8240=VECTOR('',#30174,1.);
#8241=VECTOR('',#30177,1.);
#8242=VECTOR('',#30178,1.);
#8243=VECTOR('',#30189,0.225);
#8244=VECTOR('',#30196,0.225);
#8245=VECTOR('',#30203,0.225);
#8246=VECTOR('',#30208,1.);
#8247=VECTOR('',#30209,1.);
#8248=VECTOR('',#30210,1.);
#8249=VECTOR('',#30211,1.);
#8250=VECTOR('',#30224,2.34);
#8251=VECTOR('',#30235,1.8);
#8252=VECTOR('',#30244,0.475);
#8253=VECTOR('',#30255,0.275);
#8254=VECTOR('',#30258,1.);
#8255=VECTOR('',#30259,1.);
#8256=VECTOR('',#30260,1.);
#8257=VECTOR('',#30261,1.);
#8258=VECTOR('',#30264,1.);
#8259=VECTOR('',#30265,1.);
#8260=VECTOR('',#30266,1.);
#8261=VECTOR('',#30269,1.);
#8262=VECTOR('',#30270,1.);
#8263=VECTOR('',#30271,1.);
#8264=VECTOR('',#30274,1.);
#8265=VECTOR('',#30275,1.);
#8266=VECTOR('',#30286,0.475000000000001);
#8267=VECTOR('',#30297,0.274999999999999);
#8268=VECTOR('',#30300,1.);
#8269=VECTOR('',#30301,1.);
#8270=VECTOR('',#30302,1.);
#8271=VECTOR('',#30303,1.);
#8272=VECTOR('',#30306,1.);
#8273=VECTOR('',#30307,1.);
#8274=VECTOR('',#30308,1.);
#8275=VECTOR('',#30311,1.);
#8276=VECTOR('',#30312,1.);
#8277=VECTOR('',#30313,1.);
#8278=VECTOR('',#30316,1.);
#8279=VECTOR('',#30317,1.);
#8280=VECTOR('',#30328,0.375);
#8281=VECTOR('',#30339,0.375);
#8282=VECTOR('',#30350,0.375);
#8283=VECTOR('',#30361,0.375);
#8284=VECTOR('',#30372,0.225);
#8285=VECTOR('',#30377,0.225);
#8286=VECTOR('',#30382,0.225);
#8287=VECTOR('',#30387,0.225000000000001);
#8288=VECTOR('',#30390,1.);
#8289=VECTOR('',#30391,1.);
#8290=VECTOR('',#30392,1.);
#8291=VECTOR('',#30393,1.);
#8292=VECTOR('',#30396,1.);
#8293=VECTOR('',#30397,1.);
#8294=VECTOR('',#30398,1.);
#8295=VECTOR('',#30401,1.);
#8296=VECTOR('',#30402,1.);
#8297=VECTOR('',#30403,1.);
#8298=VECTOR('',#30406,1.);
#8299=VECTOR('',#30407,1.);
#8300=VECTOR('',#30408,1.);
#8301=VECTOR('',#30411,1.);
#8302=VECTOR('',#30412,1.);
#8303=VECTOR('',#30413,1.);
#8304=VECTOR('',#30416,1.);
#8305=VECTOR('',#30417,1.);
#8306=VECTOR('',#30418,1.);
#8307=VECTOR('',#30421,1.);
#8308=VECTOR('',#30422,1.);
#8309=VECTOR('',#30423,1.);
#8310=VECTOR('',#30426,1.);
#8311=VECTOR('',#30427,1.);
#8312=VECTOR('',#30428,1.);
#8313=VECTOR('',#30431,1.);
#8314=VECTOR('',#30432,1.);
#8315=VECTOR('',#30433,1.);
#8316=VECTOR('',#30436,1.);
#8317=VECTOR('',#30437,1.);
#8318=VECTOR('',#30438,1.);
#8319=VECTOR('',#30441,1.);
#8320=VECTOR('',#30442,1.);
#8321=VECTOR('',#30443,1.);
#8322=VECTOR('',#30446,1.);
#8323=VECTOR('',#30447,1.);
#8324=VECTOR('',#30470,1.070235);
#8325=VECTOR('',#30477,0.6);
#8326=VECTOR('',#30482,0.63);
#8327=VECTOR('',#30491,1.070235);
#8328=VECTOR('',#30498,0.63);
#8329=VECTOR('',#30517,1.129765);
#8330=VECTOR('',#30528,1.57);
#8331=VECTOR('',#30533,1.6);
#8332=VECTOR('',#30538,1.57);
#8333=VECTOR('',#30543,1.129765);
#8334=VECTOR('',#30590,1.123812);
#8335=VECTOR('',#30659,1.076188);
#8336=VECTOR('',#30688,1.119765);
#8337=VECTOR('',#30695,1.085235);
#8338=VECTOR('',#30706,1.119765);
#8339=VECTOR('',#30713,1.085235);
#8340=VECTOR('',#30742,1.63531);
#8341=VECTOR('',#30749,1.);
#8342=VECTOR('',#30754,1.05);
#8343=VECTOR('',#30763,1.63531);
#8344=VECTOR('',#30770,1.05);
#8345=VECTOR('',#30789,1.71469);
#8346=VECTOR('',#30800,2.3);
#8347=VECTOR('',#30805,2.35);
#8348=VECTOR('',#30810,2.3);
#8349=VECTOR('',#30815,1.71469);
#8350=VECTOR('',#30866,1.706752);
#8351=VECTOR('',#30943,1.643248);
#8352=VECTOR('',#30972,1.70469);
#8353=VECTOR('',#30979,1.65031);
#8354=VECTOR('',#30990,1.70469);
#8355=VECTOR('',#30997,1.65031);
#8356=VECTOR('',#31012,1.);
#8357=VECTOR('',#31013,1.);
#8358=VECTOR('',#31014,1.);
#8359=VECTOR('',#31015,1.);
#8360=VECTOR('',#31018,1.);
#8361=VECTOR('',#31019,1.);
#8362=VECTOR('',#31020,1.);
#8363=VECTOR('',#31023,1.);
#8364=VECTOR('',#31024,1.);
#8365=VECTOR('',#31025,1.);
#8366=VECTOR('',#31028,1.);
#8367=VECTOR('',#31029,1.);
#8368=VECTOR('',#31030,1.);
#8369=VECTOR('',#31033,1.);
#8370=VECTOR('',#31034,1.);
#8371=VECTOR('',#31035,1.);
#8372=VECTOR('',#31038,1.);
#8373=VECTOR('',#31039,1.);
#8374=VECTOR('',#31056,0.4);
#8375=VECTOR('',#31061,0.425);
#8376=VECTOR('',#31066,0.41);
#8377=VECTOR('',#31075,0.26);
#8378=VECTOR('',#31078,0.25);
#8379=VECTOR('',#31087,0.275);
#8380=VECTOR('',#31094,0.275);
#8381=VECTOR('',#31101,0.275);
#8382=VECTOR('',#31108,0.275);
#8383=VECTOR('',#31113,1.);
#8384=VECTOR('',#31114,1.);
#8385=VECTOR('',#31115,1.);
#8386=VECTOR('',#31116,1.);
#8387=VECTOR('',#31119,1.);
#8388=VECTOR('',#31120,1.);
#8389=VECTOR('',#31121,1.);
#8390=VECTOR('',#31124,1.);
#8391=VECTOR('',#31125,1.);
#8392=VECTOR('',#31126,1.);
#8393=VECTOR('',#31129,1.);
#8394=VECTOR('',#31130,1.);
#8395=VECTOR('',#31141,0.275);
#8396=VECTOR('',#31148,0.275);
#8397=VECTOR('',#31155,0.275);
#8398=VECTOR('',#31162,0.275);
#8399=VECTOR('',#31169,0.275);
#8400=VECTOR('',#31176,0.275);
#8401=VECTOR('',#31183,0.275);
#8402=VECTOR('',#31190,0.275);
#8403=VECTOR('',#31195,1.);
#8404=VECTOR('',#31196,1.);
#8405=VECTOR('',#31197,1.);
#8406=VECTOR('',#31198,1.);
#8407=VECTOR('',#31201,1.);
#8408=VECTOR('',#31202,1.);
#8409=VECTOR('',#31203,1.);
#8410=VECTOR('',#31206,1.);
#8411=VECTOR('',#31207,1.);
#8412=VECTOR('',#31208,1.);
#8413=VECTOR('',#31211,1.);
#8414=VECTOR('',#31212,1.);
#8415=VECTOR('',#31223,0.210000000000001);
#8416=VECTOR('',#31232,0.210000000000001);
#8417=VECTOR('',#31241,0.210000000000001);
#8418=VECTOR('',#31250,0.210000000000001);
#8419=VECTOR('',#31259,0.165);
#8420=VECTOR('',#31268,0.165);
#8421=VECTOR('',#31277,0.165);
#8422=VECTOR('',#31286,1.11);
#8423=VECTOR('',#31291,1.);
#8424=VECTOR('',#31292,1.);
#8425=VECTOR('',#31293,1.);
#8426=VECTOR('',#31294,1.);
#8427=VECTOR('',#31297,1.);
#8428=VECTOR('',#31298,1.);
#8429=VECTOR('',#31299,1.);
#8430=VECTOR('',#31302,1.);
#8431=VECTOR('',#31303,1.);
#8432=VECTOR('',#31304,1.);
#8433=VECTOR('',#31307,1.);
#8434=VECTOR('',#31308,1.);
#8435=VECTOR('',#31319,1.);
#8436=VECTOR('',#31324,1.);
#8437=VECTOR('',#31327,0.21);
#8438=VECTOR('',#31332,1.);
#8439=VECTOR('',#31335,1.);
#8440=VECTOR('',#31340,1.);
#8441=VECTOR('',#31343,0.21);
#8442=VECTOR('',#31348,1.);
#8443=VECTOR('',#31351,1.);
#8444=VECTOR('',#31356,1.);
#8445=VECTOR('',#31359,0.21);
#8446=VECTOR('',#31364,1.);
#8447=VECTOR('',#31367,1.);
#8448=VECTOR('',#31372,1.);
#8449=VECTOR('',#31375,0.21);
#8450=VECTOR('',#31380,1.);
#8451=VECTOR('',#31383,1.);
#8452=VECTOR('',#31384,1.);
#8453=VECTOR('',#31385,1.);
#8454=VECTOR('',#31386,1.);
#8455=VECTOR('',#31387,1.);
#8456=VECTOR('',#31388,1.);
#8457=VECTOR('',#31391,1.);
#8458=VECTOR('',#31392,1.);
#8459=VECTOR('',#31393,1.);
#8460=VECTOR('',#31394,1.);
#8461=VECTOR('',#31395,1.);
#8462=VECTOR('',#31396,1.);
#8463=VECTOR('',#31399,1.);
#8464=VECTOR('',#31400,1.);
#8465=VECTOR('',#31401,1.);
#8466=VECTOR('',#31402,1.);
#8467=VECTOR('',#31403,1.);
#8468=VECTOR('',#31404,1.);
#8469=VECTOR('',#31405,1.);
#8470=VECTOR('',#31406,1.);
#8471=VECTOR('',#31407,1.);
#8472=VECTOR('',#31408,1.);
#8473=VECTOR('',#31411,1.);
#8474=VECTOR('',#31412,1.);
#8475=VECTOR('',#31415,1.);
#8476=VECTOR('',#31416,1.);
#8477=VECTOR('',#31419,1.);
#8478=VECTOR('',#31420,1.);
#8479=VECTOR('',#31423,1.);
#8480=VECTOR('',#31424,1.);
#8481=VECTOR('',#31427,1.);
#8482=VECTOR('',#31430,1.);
#8483=VECTOR('',#31431,1.);
#8484=VECTOR('',#31434,1.);
#8485=VECTOR('',#31435,1.);
#8486=VECTOR('',#31438,1.);
#8487=VECTOR('',#31439,1.);
#8488=VECTOR('',#31442,1.);
#8489=VECTOR('',#31443,1.);
#8490=VECTOR('',#31446,1.);
#8491=VECTOR('',#31453,1.);
#8492=VECTOR('',#31454,1.);
#8493=VECTOR('',#31455,1.);
#8494=VECTOR('',#31456,1.);
#8495=VECTOR('',#31459,1.);
#8496=VECTOR('',#31460,1.);
#8497=VECTOR('',#31461,1.);
#8498=VECTOR('',#31464,1.);
#8499=VECTOR('',#31465,1.);
#8500=VECTOR('',#31466,1.);
#8501=VECTOR('',#31469,1.);
#8502=VECTOR('',#31470,1.);
#8503=VECTOR('',#31471,1.);
#8504=VECTOR('',#31474,1.);
#8505=VECTOR('',#31475,1.);
#8506=VECTOR('',#31476,1.);
#8507=VECTOR('',#31479,1.);
#8508=VECTOR('',#31480,1.);
#8509=VECTOR('',#31481,1.);
#8510=VECTOR('',#31484,1.);
#8511=VECTOR('',#31485,1.);
#8512=VECTOR('',#31486,1.);
#8513=VECTOR('',#31489,1.);
#8514=VECTOR('',#31490,1.);
#8515=VECTOR('',#31499,1.);
#8516=VECTOR('',#31500,1.);
#8517=VECTOR('',#31501,1.);
#8518=VECTOR('',#31502,1.);
#8519=VECTOR('',#31505,1.);
#8520=VECTOR('',#31506,1.);
#8521=VECTOR('',#31507,1.);
#8522=VECTOR('',#31510,1.);
#8523=VECTOR('',#31511,1.);
#8524=VECTOR('',#31512,1.);
#8525=VECTOR('',#31515,1.);
#8526=VECTOR('',#31516,1.);
#8527=VECTOR('',#31517,1.);
#8528=VECTOR('',#31520,1.);
#8529=VECTOR('',#31521,1.);
#8530=VECTOR('',#31522,1.);
#8531=VECTOR('',#31525,1.);
#8532=VECTOR('',#31526,1.);
#8533=VECTOR('',#31527,1.);
#8534=VECTOR('',#31530,1.);
#8535=VECTOR('',#31531,1.);
#8536=VECTOR('',#31532,1.);
#8537=VECTOR('',#31535,1.);
#8538=VECTOR('',#31536,1.);
#8539=VECTOR('',#31553,0.275);
#8540=VECTOR('',#31558,0.265);
#8541=VECTOR('',#31567,0.5);
#8542=VECTOR('',#31576,1.);
#8543=VECTOR('',#31577,1.);
#8544=VECTOR('',#31578,1.);
#8545=VECTOR('',#31579,1.);
#8546=VECTOR('',#31582,1.);
#8547=VECTOR('',#31583,1.);
#8548=VECTOR('',#31584,1.);
#8549=VECTOR('',#31587,1.);
#8550=VECTOR('',#31588,1.);
#8551=VECTOR('',#31589,1.);
#8552=VECTOR('',#31592,1.);
#8553=VECTOR('',#31593,1.);
#8554=VECTOR('',#31594,1.);
#8555=VECTOR('',#31597,1.);
#8556=VECTOR('',#31598,1.);
#8557=VECTOR('',#31599,1.);
#8558=VECTOR('',#31602,1.);
#8559=VECTOR('',#31603,1.);
#8560=VECTOR('',#31616,0.25);
#8561=VECTOR('',#31629,0.4);
#8562=VECTOR('',#31634,0.425);
#8563=VECTOR('',#31639,0.41);
#8564=VECTOR('',#31648,0.26);
#8565=VECTOR('',#31651,0.25);
#8566=VECTOR('',#31656,0.45);
#8567=VECTOR('',#31661,0.45);
#8568=VECTOR('',#31664,0.45);
#8569=VECTOR('',#31667,0.45);
#8570=VECTOR('',#31670,0.45);
#8571=VECTOR('',#31673,0.45);
#8572=VECTOR('',#31676,0.45);
#8573=VECTOR('',#31679,0.45);
#8574=VECTOR('',#31682,0.45);
#8575=VECTOR('',#31687,0.625);
#8576=VECTOR('',#31692,0.625);
#8577=VECTOR('',#31695,0.625);
#8578=VECTOR('',#31698,0.625);
#8579=VECTOR('',#31701,0.625);
#8580=VECTOR('',#31704,0.625);
#8581=VECTOR('',#31707,0.625);
#8582=VECTOR('',#31710,0.625);
#8583=VECTOR('',#31713,0.625);
#8584=VECTOR('',#31720,1.);
#8585=VECTOR('',#31735,0.225);
#8586=VECTOR('',#31740,0.225);
#8587=VECTOR('',#31745,0.225);
#8588=VECTOR('',#31748,1.);
#8589=VECTOR('',#31749,1.);
#8590=VECTOR('',#31750,1.);
#8591=VECTOR('',#31763,1.1);
#8592=VECTOR('',#31778,0.325);
#8593=VECTOR('',#31783,0.35);
#8594=VECTOR('',#31788,0.335);
#8595=VECTOR('',#31797,0.21);
#8596=VECTOR('',#31802,0.2);
#8597=VECTOR('',#31807,0.18);
#8598=VECTOR('',#31812,1.);
#8599=VECTOR('',#31813,1.);
#8600=VECTOR('',#31814,1.);
#8601=VECTOR('',#31815,1.);
#8602=VECTOR('',#31818,1.);
#8603=VECTOR('',#31819,1.);
#8604=VECTOR('',#31820,1.);
#8605=VECTOR('',#31823,1.);
#8606=VECTOR('',#31824,1.);
#8607=VECTOR('',#31825,1.);
#8608=VECTOR('',#31828,1.);
#8609=VECTOR('',#31829,1.);
#8610=VECTOR('',#31830,1.);
#8611=VECTOR('',#31833,1.);
#8612=VECTOR('',#31834,1.);
#8613=VECTOR('',#31835,1.);
#8614=VECTOR('',#31838,1.);
#8615=VECTOR('',#31839,1.);
#8616=VECTOR('',#31854,0.4);
#8617=VECTOR('',#31859,0.425);
#8618=VECTOR('',#31864,0.41);
#8619=VECTOR('',#31873,0.26);
#8620=VECTOR('',#31878,0.25);
#8621=VECTOR('',#31883,0.225);
#8622=VECTOR('',#31888,1.);
#8623=VECTOR('',#31889,1.);
#8624=VECTOR('',#31890,1.);
#8625=VECTOR('',#31891,1.);
#8626=VECTOR('',#31894,1.);
#8627=VECTOR('',#31895,1.);
#8628=VECTOR('',#31896,1.);
#8629=VECTOR('',#31899,1.);
#8630=VECTOR('',#31900,1.);
#8631=VECTOR('',#31901,1.);
#8632=VECTOR('',#31904,1.);
#8633=VECTOR('',#31905,1.);
#8634=VECTOR('',#31906,1.);
#8635=VECTOR('',#31909,1.);
#8636=VECTOR('',#31910,1.);
#8637=VECTOR('',#31911,1.);
#8638=VECTOR('',#31914,1.);
#8639=VECTOR('',#31915,1.);
#8640=VECTOR('',#31966,0.6);
#8641=VECTOR('',#31971,0.6);
#8642=VECTOR('',#31974,0.6);
#8643=VECTOR('',#31977,0.6);
#8644=VECTOR('',#31980,0.6);
#8645=VECTOR('',#31983,0.6);
#8646=VECTOR('',#31986,0.6);
#8647=VECTOR('',#31989,0.6);
#8648=VECTOR('',#31992,0.6);
#8649=VECTOR('',#31995,0.6);
#8650=VECTOR('',#31998,0.6);
#8651=VECTOR('',#32001,0.6);
#8652=VECTOR('',#32004,0.6);
#8653=VECTOR('',#32007,0.6);
#8654=VECTOR('',#32010,0.6);
#8655=VECTOR('',#32013,0.6);
#8656=VECTOR('',#32016,0.6);
#8657=VECTOR('',#32019,0.6);
#8658=VECTOR('',#32022,0.6);
#8659=VECTOR('',#32025,0.6);
#8660=VECTOR('',#32028,0.6);
#8661=VECTOR('',#32031,0.6);
#8662=VECTOR('',#32034,0.6);
#8663=VECTOR('',#32037,0.6);
#8664=VECTOR('',#32040,0.6);
#8665=VECTOR('',#32043,0.6);
#8666=VECTOR('',#32046,0.6);
#8667=VECTOR('',#32049,0.6);
#8668=VECTOR('',#32052,0.6);
#8669=VECTOR('',#32055,0.6);
#8670=VECTOR('',#32058,0.6);
#8671=VECTOR('',#32061,0.6);
#8672=VECTOR('',#32064,0.6);
#8673=VECTOR('',#32067,0.6);
#8674=VECTOR('',#32070,0.6);
#8675=VECTOR('',#32073,0.6);
#8676=VECTOR('',#32076,0.6);
#8677=VECTOR('',#32079,0.6);
#8678=VECTOR('',#32082,0.6);
#8679=VECTOR('',#32085,0.6);
#8680=VECTOR('',#32088,0.6);
#8681=VECTOR('',#32091,0.6);
#8682=VECTOR('',#32094,0.6);
#8683=VECTOR('',#32097,0.6);
#8684=VECTOR('',#32100,0.6);
#8685=VECTOR('',#32103,0.6);
#8686=VECTOR('',#32106,0.6);
#8687=VECTOR('',#32109,0.6);
#8688=VECTOR('',#32112,0.6);
#8689=VECTOR('',#32115,0.6);
#8690=VECTOR('',#32118,0.6);
#8691=VECTOR('',#32121,0.6);
#8692=VECTOR('',#32124,0.6);
#8693=VECTOR('',#32127,0.6);
#8694=VECTOR('',#32130,0.6);
#8695=VECTOR('',#32133,0.6);
#8696=VECTOR('',#32136,0.6);
#8697=VECTOR('',#32139,0.6);
#8698=VECTOR('',#32142,0.6);
#8699=VECTOR('',#32145,0.6);
#8700=VECTOR('',#32148,0.6);
#8701=VECTOR('',#32151,0.6);
#8702=VECTOR('',#32154,0.6);
#8703=VECTOR('',#32157,0.415875);
#8704=VECTOR('',#32162,0.415875);
#8705=VECTOR('',#32167,0.415875);
#8706=VECTOR('',#32170,0.415875);
#8707=VECTOR('',#32173,0.415875);
#8708=VECTOR('',#32176,0.415875);
#8709=VECTOR('',#32179,0.415875);
#8710=VECTOR('',#32182,0.415875);
#8711=VECTOR('',#32185,0.415875);
#8712=VECTOR('',#32188,0.415875);
#8713=VECTOR('',#32191,0.415875);
#8714=VECTOR('',#32194,0.415875);
#8715=VECTOR('',#32197,0.415875);
#8716=VECTOR('',#32200,0.415875);
#8717=VECTOR('',#32203,0.415875);
#8718=VECTOR('',#32206,0.415875);
#8719=VECTOR('',#32209,0.415875);
#8720=VECTOR('',#32212,0.415875);
#8721=VECTOR('',#32215,0.415875);
#8722=VECTOR('',#32218,0.415875);
#8723=VECTOR('',#32221,0.415875);
#8724=VECTOR('',#32224,0.415875);
#8725=VECTOR('',#32227,0.415875);
#8726=VECTOR('',#32230,0.415875);
#8727=VECTOR('',#32233,0.415875);
#8728=VECTOR('',#32236,0.415875);
#8729=VECTOR('',#32239,0.415875);
#8730=VECTOR('',#32242,0.415875);
#8731=VECTOR('',#32245,0.415875);
#8732=VECTOR('',#32248,0.415875);
#8733=VECTOR('',#32251,0.415875);
#8734=VECTOR('',#32254,0.415875);
#8735=VECTOR('',#32257,0.415875);
#8736=VECTOR('',#32260,0.415875);
#8737=VECTOR('',#32263,0.415875);
#8738=VECTOR('',#32266,0.415875);
#8739=VECTOR('',#32269,0.415875);
#8740=VECTOR('',#32272,0.415875);
#8741=VECTOR('',#32275,0.415875);
#8742=VECTOR('',#32278,0.415875);
#8743=VECTOR('',#32281,0.415875);
#8744=VECTOR('',#32284,0.415875);
#8745=VECTOR('',#32287,0.415875);
#8746=VECTOR('',#32290,0.415875);
#8747=VECTOR('',#32293,0.415875);
#8748=VECTOR('',#32296,0.415875);
#8749=VECTOR('',#32299,0.415875);
#8750=VECTOR('',#32302,0.415875);
#8751=VECTOR('',#32305,0.415875);
#8752=VECTOR('',#32308,0.415875);
#8753=VECTOR('',#32311,0.415875);
#8754=VECTOR('',#32314,0.415875);
#8755=VECTOR('',#32317,0.415875);
#8756=VECTOR('',#32320,0.415875);
#8757=VECTOR('',#32323,0.415875);
#8758=VECTOR('',#32326,0.415875);
#8759=VECTOR('',#32329,0.415875);
#8760=VECTOR('',#32332,0.415875);
#8761=VECTOR('',#32335,0.415875);
#8762=VECTOR('',#32338,0.415875);
#8763=VECTOR('',#32341,0.415875);
#8764=VECTOR('',#32344,0.415875);
#8765=VECTOR('',#32347,0.415875);
#8766=VECTOR('',#32356,0.6);
#8767=VECTOR('',#32365,1.);
#8768=VECTOR('',#32366,1.);
#8769=VECTOR('',#32367,1.);
#8770=VECTOR('',#32368,1.);
#8771=VECTOR('',#32373,1.);
#8772=VECTOR('',#32374,1.);
#8773=VECTOR('',#32377,1.);
#8774=VECTOR('',#32378,1.);
#8775=VECTOR('',#32381,1.);
#8776=VECTOR('',#32382,1.);
#8777=VECTOR('',#32391,1.);
#8778=VECTOR('',#32406,1.35);
#8779=VECTOR('',#32417,1.01);
#8780=VECTOR('',#32424,1.35);
#8781=VECTOR('',#32435,1.);
#8782=VECTOR('',#32442,0.210000000000001);
#8783=VECTOR('',#32445,1.);
#8784=VECTOR('',#32450,1.005);
#8785=VECTOR('',#32457,1.5);
#8786=VECTOR('',#32470,0.25);
#8787=VECTOR('',#32475,1.);
#8788=VECTOR('',#32482,0.210000000000001);
#8789=VECTOR('',#32485,1.);
#8790=VECTOR('',#32488,1.);
#8791=VECTOR('',#32489,1.);
#8792=VECTOR('',#32490,1.);
#8793=VECTOR('',#32491,1.);
#8794=VECTOR('',#32492,1.);
#8795=VECTOR('',#32493,1.);
#8796=VECTOR('',#32496,1.);
#8797=VECTOR('',#32497,1.);
#8798=VECTOR('',#32498,1.);
#8799=VECTOR('',#32501,1.);
#8800=VECTOR('',#32502,1.);
#8801=VECTOR('',#32503,1.);
#8802=VECTOR('',#32504,1.);
#8803=VECTOR('',#32505,1.);
#8804=VECTOR('',#32520,3.5);
#8805=VECTOR('',#32537,0.33);
#8806=VECTOR('',#32544,0.4);
#8807=VECTOR('',#32557,0.405);
#8808=VECTOR('',#32564,0.9);
#8809=VECTOR('',#32575,1.);
#8810=VECTOR('',#32576,1.);
#8811=VECTOR('',#32577,1.);
#8812=VECTOR('',#32578,1.);
#8813=VECTOR('',#32579,1.);
#8814=VECTOR('',#32580,1.);
#8815=VECTOR('',#32581,1.);
#8816=VECTOR('',#32582,1.);
#8817=VECTOR('',#32585,1.);
#8818=VECTOR('',#32586,1.);
#8819=VECTOR('',#32587,1.);
#8820=VECTOR('',#32590,1.);
#8821=VECTOR('',#32591,1.);
#8822=VECTOR('',#32594,1.);
#8823=VECTOR('',#32595,1.);
#8824=VECTOR('',#32598,1.);
#8825=VECTOR('',#32599,1.);
#8826=VECTOR('',#32602,1.);
#8827=VECTOR('',#32603,1.);
#8828=VECTOR('',#32604,1.);
#8829=VECTOR('',#32605,1.);
#8830=VECTOR('',#32608,1.);
#8831=VECTOR('',#32611,1.);
#8832=VECTOR('',#32614,1.);
#8833=VECTOR('',#32621,1.);
#8834=VECTOR('',#32622,1.);
#8835=VECTOR('',#32623,1.);
#8836=VECTOR('',#32624,1.);
#8837=VECTOR('',#32627,1.);
#8838=VECTOR('',#32628,1.);
#8839=VECTOR('',#32629,1.);
#8840=VECTOR('',#32632,1.);
#8841=VECTOR('',#32633,1.);
#8842=VECTOR('',#32634,1.);
#8843=VECTOR('',#32637,1.);
#8844=VECTOR('',#32638,1.);
#8845=VECTOR('',#32639,1.);
#8846=VECTOR('',#32642,1.);
#8847=VECTOR('',#32643,1.);
#8848=VECTOR('',#32644,1.);
#8849=VECTOR('',#32647,1.);
#8850=VECTOR('',#32648,1.);
#8851=VECTOR('',#32659,0.235);
#8852=VECTOR('',#32664,0.25);
#8853=VECTOR('',#32669,0.2125);
#8854=VECTOR('',#32678,0.32);
#8855=VECTOR('',#32685,0.6);
#8856=VECTOR('',#32702,0.475);
#8857=VECTOR('',#32707,0.5);
#8858=VECTOR('',#32712,0.485);
#8859=VECTOR('',#32721,0.31);
#8860=VECTOR('',#32726,0.3);
#8861=VECTOR('',#32731,0.27);
#8862=VECTOR('',#32736,1.);
#8863=VECTOR('',#32737,1.);
#8864=VECTOR('',#32738,1.);
#8865=VECTOR('',#32739,1.);
#8866=VECTOR('',#32742,1.);
#8867=VECTOR('',#32743,1.);
#8868=VECTOR('',#32744,1.);
#8869=VECTOR('',#32747,1.);
#8870=VECTOR('',#32748,1.);
#8871=VECTOR('',#32749,1.);
#8872=VECTOR('',#32752,1.);
#8873=VECTOR('',#32753,1.);
#8874=VECTOR('',#32754,1.);
#8875=VECTOR('',#32757,1.);
#8876=VECTOR('',#32758,1.);
#8877=VECTOR('',#32759,1.);
#8878=VECTOR('',#32762,1.);
#8879=VECTOR('',#32763,1.);
#8880=CIRCLE('',#24005,0.210000000000001);
#8881=CIRCLE('',#24006,0.210000000000001);
#8882=CIRCLE('',#24008,0.21);
#8883=CIRCLE('',#24009,0.21);
#8884=CIRCLE('',#24011,0.329999999999998);
#8885=CIRCLE('',#24012,0.329999999999998);
#8886=CIRCLE('',#24014,0.329999999999998);
#8887=CIRCLE('',#24015,0.329999999999998);
#8888=CIRCLE('',#24017,0.275);
#8889=CIRCLE('',#24018,0.275);
#8890=CIRCLE('',#24020,0.275);
#8891=CIRCLE('',#24021,0.275);
#8892=CIRCLE('',#24023,0.210000000000001);
#8893=CIRCLE('',#24024,0.210000000000001);
#8894=CIRCLE('',#24026,0.21);
#8895=CIRCLE('',#24027,0.21);
#8896=CIRCLE('',#24029,0.21);
#8897=CIRCLE('',#24030,0.21);
#8898=CIRCLE('',#24032,0.210000000000001);
#8899=CIRCLE('',#24033,0.210000000000001);
#8900=CIRCLE('',#24056,0.5);
#8901=CIRCLE('',#24057,0.5);
#8902=CIRCLE('',#24059,0.5);
#8903=CIRCLE('',#24060,0.5);
#8904=CIRCLE('',#24062,0.164999999999999);
#8905=CIRCLE('',#24063,0.164999999999999);
#8906=CIRCLE('',#24065,0.164999999999999);
#8907=CIRCLE('',#24066,0.164999999999999);
#8908=CIRCLE('',#24068,0.165);
#8909=CIRCLE('',#24069,0.165);
#8910=CIRCLE('',#24071,0.164999999999999);
#8911=CIRCLE('',#24072,0.164999999999999);
#8912=CIRCLE('',#24074,0.5);
#8913=CIRCLE('',#24075,0.5);
#8914=CIRCLE('',#24077,0.274999999999999);
#8915=CIRCLE('',#24079,0.5);
#8916=CIRCLE('',#24080,0.5);
#8917=CIRCLE('',#24082,0.275);
#8918=CIRCLE('',#24084,0.5);
#8919=CIRCLE('',#24085,0.5);
#8920=CIRCLE('',#24087,0.275);
#8921=CIRCLE('',#24089,0.5);
#8922=CIRCLE('',#24090,0.5);
#8923=CIRCLE('',#24092,0.274999999999999);
#8924=CIRCLE('',#24095,0.274999999999999);
#8925=CIRCLE('',#24097,0.275);
#8926=CIRCLE('',#24099,0.275);
#8927=CIRCLE('',#24101,0.274999999999999);
#8928=CIRCLE('',#24109,0.165);
#8929=CIRCLE('',#24110,0.165);
#8930=CIRCLE('',#24112,0.165);
#8931=CIRCLE('',#24113,0.165);
#8932=CIRCLE('',#24115,0.165);
#8933=CIRCLE('',#24116,0.165);
#8934=CIRCLE('',#24118,1.6);
#8935=CIRCLE('',#24119,1.6);
#8936=CIRCLE('',#24121,1.4);
#8937=CIRCLE('',#24123,1.4);
#8938=CIRCLE('',#24125,0.21);
#8939=CIRCLE('',#24126,0.21);
#8940=CIRCLE('',#24129,0.21);
#8941=CIRCLE('',#24130,0.21);
#8942=CIRCLE('',#24140,0.225);
#8943=CIRCLE('',#24141,0.225);
#8944=CIRCLE('',#24143,0.225);
#8945=CIRCLE('',#24144,0.225);
#8946=CIRCLE('',#24146,0.225);
#8947=CIRCLE('',#24147,0.225);
#8948=CIRCLE('',#24149,1.59);
#8949=CIRCLE('',#24150,1.59);
#8950=CIRCLE('',#24152,1.2);
#8951=CIRCLE('',#24154,1.2);
#8952=CIRCLE('',#24156,2.4);
#8953=CIRCLE('',#24157,2.4);
#8954=CIRCLE('',#24162,0.165);
#8955=CIRCLE('',#24163,0.165);
#8956=CIRCLE('',#24165,0.165);
#8957=CIRCLE('',#24166,0.165);
#8958=CIRCLE('',#24168,0.165);
#8959=CIRCLE('',#24169,0.165);
#8960=CIRCLE('',#24171,2.35);
#8961=CIRCLE('',#24172,2.35);
#8962=CIRCLE('',#24174,2.15);
#8963=CIRCLE('',#24176,2.15);
#8964=CIRCLE('',#24178,0.25);
#8965=CIRCLE('',#24179,0.25);
#8966=CIRCLE('',#24182,0.25);
#8967=CIRCLE('',#24183,0.25);
#8968=CIRCLE('',#24193,0.225);
#8969=CIRCLE('',#24194,0.225);
#8970=CIRCLE('',#24196,0.225);
#8971=CIRCLE('',#24197,0.225);
#8972=CIRCLE('',#24199,0.225);
#8973=CIRCLE('',#24200,0.225);
#8974=CIRCLE('',#24203,3.);
#8975=CIRCLE('',#24204,2.34);
#8976=CIRCLE('',#24206,3.);
#8977=CIRCLE('',#24208,2.34);
#8978=CIRCLE('',#24210,1.8);
#8979=CIRCLE('',#24212,1.8);
#8980=CIRCLE('',#24216,0.475);
#8981=CIRCLE('',#24217,0.475);
#8982=CIRCLE('',#24219,0.275);
#8983=CIRCLE('',#24221,0.275);
#8984=CIRCLE('',#24230,0.475000000000001);
#8985=CIRCLE('',#24231,0.475000000000001);
#8986=CIRCLE('',#24233,0.274999999999999);
#8987=CIRCLE('',#24235,0.274999999999999);
#8988=CIRCLE('',#24244,0.375);
#8989=CIRCLE('',#24245,0.375);
#8990=CIRCLE('',#24247,0.225);
#8991=CIRCLE('',#24249,0.375);
#8992=CIRCLE('',#24250,0.375);
#8993=CIRCLE('',#24252,0.225);
#8994=CIRCLE('',#24254,0.375);
#8995=CIRCLE('',#24255,0.375);
#8996=CIRCLE('',#24257,0.225);
#8997=CIRCLE('',#24259,0.375);
#8998=CIRCLE('',#24260,0.375);
#8999=CIRCLE('',#24262,0.225000000000001);
#9000=CIRCLE('',#24264,0.225);
#9001=CIRCLE('',#24266,0.225);
#9002=CIRCLE('',#24268,0.225);
#9003=CIRCLE('',#24270,0.225000000000001);
#9004=CIRCLE('',#24288,1.070235);
#9005=CIRCLE('',#24289,1.070235);
#9006=CIRCLE('',#24290,0.309556);
#9007=CIRCLE('',#24291,1.070235);
#9008=CIRCLE('',#24292,1.070235);
#9009=CIRCLE('',#24294,1.070235);
#9010=CIRCLE('',#24296,0.6);
#9011=CIRCLE('',#24297,0.6);
#9012=CIRCLE('',#24299,0.66);
#9013=CIRCLE('',#24302,1.070235);
#9014=CIRCLE('',#24304,0.66);
#9015=CIRCLE('',#24308,1.129765);
#9016=CIRCLE('',#24309,1.129765);
#9017=CIRCLE('',#24310,0.309556);
#9018=CIRCLE('',#24311,1.129765);
#9019=CIRCLE('',#24312,1.129765);
#9020=CIRCLE('',#24314,1.129765);
#9021=CIRCLE('',#24316,1.54);
#9022=CIRCLE('',#24317,1.129765);
#9023=CIRCLE('',#24319,1.6);
#9024=CIRCLE('',#24321,1.6);
#9025=CIRCLE('',#24323,1.54);
#9026=CIRCLE('',#24328,0.29765);
#9027=CIRCLE('',#24330,0.29765);
#9028=CIRCLE('',#24332,0.29765);
#9029=CIRCLE('',#24334,0.29765);
#9030=CIRCLE('',#24336,0.29765);
#9031=CIRCLE('',#24338,0.29765);
#9032=CIRCLE('',#24340,0.29765);
#9033=CIRCLE('',#24343,0.303778037777585);
#9034=CIRCLE('',#24344,0.303778037777585);
#9035=CIRCLE('',#24346,1.123812);
#9036=CIRCLE('',#24347,1.123812);
#9037=CIRCLE('',#24348,1.123812);
#9038=CIRCLE('',#24349,1.123812);
#9039=CIRCLE('',#24350,1.123812);
#9040=CIRCLE('',#24351,1.123812);
#9041=CIRCLE('',#24352,1.123812);
#9042=CIRCLE('',#24353,1.123812);
#9043=CIRCLE('',#24354,1.123812);
#9044=CIRCLE('',#24356,1.076188);
#9045=CIRCLE('',#24357,0.303778037777585);
#9046=CIRCLE('',#24359,0.303778037777585);
#9047=CIRCLE('',#24361,1.076188);
#9048=CIRCLE('',#24362,0.303778037777585);
#9049=CIRCLE('',#24364,0.303778037777585);
#9050=CIRCLE('',#24366,1.076188);
#9051=CIRCLE('',#24367,1.076188);
#9052=CIRCLE('',#24368,0.303778037777585);
#9053=CIRCLE('',#24370,0.303778037777585);
#9054=CIRCLE('',#24372,1.076188);
#9055=CIRCLE('',#24373,0.303778037777585);
#9056=CIRCLE('',#24375,0.303778037777585);
#9057=CIRCLE('',#24377,1.076188);
#9058=CIRCLE('',#24378,0.303778037777585);
#9059=CIRCLE('',#24380,0.303778037777585);
#9060=CIRCLE('',#24382,1.076188);
#9061=CIRCLE('',#24383,1.076188);
#9062=CIRCLE('',#24384,1.076188);
#9063=CIRCLE('',#24386,0.303778037777585);
#9064=CIRCLE('',#24388,0.303778037777585);
#9065=CIRCLE('',#24393,1.119765);
#9066=CIRCLE('',#24394,1.085235);
#9067=CIRCLE('',#24396,1.119765);
#9068=CIRCLE('',#24398,1.085235);
#9069=CIRCLE('',#24401,1.119765);
#9070=CIRCLE('',#24402,1.085235);
#9071=CIRCLE('',#24404,1.119765);
#9072=CIRCLE('',#24406,1.085235);
#9073=CIRCLE('',#24416,1.63531);
#9074=CIRCLE('',#24417,1.63531);
#9075=CIRCLE('',#24418,0.412776);
#9076=CIRCLE('',#24419,1.63531);
#9077=CIRCLE('',#24420,1.63531);
#9078=CIRCLE('',#24422,1.63531);
#9079=CIRCLE('',#24424,1.);
#9080=CIRCLE('',#24425,1.);
#9081=CIRCLE('',#24427,1.1);
#9082=CIRCLE('',#24430,1.63531);
#9083=CIRCLE('',#24432,1.1);
#9084=CIRCLE('',#24436,1.71469);
#9085=CIRCLE('',#24437,1.71469);
#9086=CIRCLE('',#24438,0.412776);
#9087=CIRCLE('',#24439,1.71469);
#9088=CIRCLE('',#24440,1.71469);
#9089=CIRCLE('',#24442,1.71469);
#9090=CIRCLE('',#24444,2.25);
#9091=CIRCLE('',#24445,1.71469);
#9092=CIRCLE('',#24447,2.35);
#9093=CIRCLE('',#24449,2.35);
#9094=CIRCLE('',#24451,2.25);
#9095=CIRCLE('',#24456,0.3969);
#9096=CIRCLE('',#24458,0.3969);
#9097=CIRCLE('',#24460,0.3969);
#9098=CIRCLE('',#24462,0.3969);
#9099=CIRCLE('',#24464,0.3969);
#9100=CIRCLE('',#24466,0.3969);
#9101=CIRCLE('',#24468,0.3969);
#9102=CIRCLE('',#24470,0.3969);
#9103=CIRCLE('',#24473,0.405071403305639);
#9104=CIRCLE('',#24474,0.405071403305639);
#9105=CIRCLE('',#24476,1.706752);
#9106=CIRCLE('',#24477,1.706752);
#9107=CIRCLE('',#24478,1.706752);
#9108=CIRCLE('',#24479,1.706752);
#9109=CIRCLE('',#24480,1.706752);
#9110=CIRCLE('',#24481,1.706752);
#9111=CIRCLE('',#24482,1.706752);
#9112=CIRCLE('',#24483,1.706752);
#9113=CIRCLE('',#24484,1.706752);
#9114=CIRCLE('',#24486,1.643248);
#9115=CIRCLE('',#24487,0.405071403305639);
#9116=CIRCLE('',#24489,0.405071403305639);
#9117=CIRCLE('',#24491,1.643248);
#9118=CIRCLE('',#24492,0.405071403305639);
#9119=CIRCLE('',#24494,0.405071403305639);
#9120=CIRCLE('',#24496,1.643248);
#9121=CIRCLE('',#24497,0.405071403305639);
#9122=CIRCLE('',#24499,0.405071403305639);
#9123=CIRCLE('',#24501,1.643248);
#9124=CIRCLE('',#24502,0.405071403305639);
#9125=CIRCLE('',#24504,0.405071403305639);
#9126=CIRCLE('',#24506,1.643248);
#9127=CIRCLE('',#24507,0.405071403305639);
#9128=CIRCLE('',#24509,0.405071403305639);
#9129=CIRCLE('',#24511,1.643248);
#9130=CIRCLE('',#24512,0.405071403305639);
#9131=CIRCLE('',#24514,0.405071403305639);
#9132=CIRCLE('',#24516,1.643248);
#9133=CIRCLE('',#24517,1.643248);
#9134=CIRCLE('',#24518,1.643248);
#9135=CIRCLE('',#24520,0.405071403305639);
#9136=CIRCLE('',#24522,0.405071403305639);
#9137=CIRCLE('',#24527,1.70469);
#9138=CIRCLE('',#24528,1.65031);
#9139=CIRCLE('',#24530,1.70469);
#9140=CIRCLE('',#24532,1.65031);
#9141=CIRCLE('',#24535,1.70469);
#9142=CIRCLE('',#24536,1.65031);
#9143=CIRCLE('',#24538,1.70469);
#9144=CIRCLE('',#24540,1.65031);
#9145=CIRCLE('',#24550,0.275);
#9146=CIRCLE('',#24551,0.275);
#9147=CIRCLE('',#24553,0.275);
#9148=CIRCLE('',#24554,0.275);
#9149=CIRCLE('',#24556,0.275);
#9150=CIRCLE('',#24557,0.275);
#9151=CIRCLE('',#24559,0.275);
#9152=CIRCLE('',#24560,0.275);
#9153=CIRCLE('',#24569,0.210000000000001);
#9154=CIRCLE('',#24570,0.210000000000001);
#9155=CIRCLE('',#24572,0.210000000000001);
#9156=CIRCLE('',#24573,0.210000000000001);
#9157=CIRCLE('',#24575,0.210000000000001);
#9158=CIRCLE('',#24576,0.210000000000001);
#9159=CIRCLE('',#24578,0.210000000000001);
#9160=CIRCLE('',#24579,0.210000000000001);
#9161=CIRCLE('',#24581,0.275);
#9162=CIRCLE('',#24582,0.275);
#9163=CIRCLE('',#24584,0.275);
#9164=CIRCLE('',#24585,0.275);
#9165=CIRCLE('',#24587,0.275);
#9166=CIRCLE('',#24588,0.275);
#9167=CIRCLE('',#24590,0.275);
#9168=CIRCLE('',#24591,0.275);
#9169=CIRCLE('',#24593,0.275);
#9170=CIRCLE('',#24594,0.275);
#9171=CIRCLE('',#24596,0.275);
#9172=CIRCLE('',#24597,0.275);
#9173=CIRCLE('',#24599,0.275);
#9174=CIRCLE('',#24600,0.275);
#9175=CIRCLE('',#24602,0.275);
#9176=CIRCLE('',#24603,0.275);
#9177=CIRCLE('',#24612,0.210000000000001);
#9178=CIRCLE('',#24613,0.210000000000001);
#9179=CIRCLE('',#24616,0.210000000000001);
#9180=CIRCLE('',#24617,0.210000000000001);
#9181=CIRCLE('',#24620,0.210000000000001);
#9182=CIRCLE('',#24621,0.210000000000001);
#9183=CIRCLE('',#24624,0.210000000000001);
#9184=CIRCLE('',#24625,0.210000000000001);
#9185=CIRCLE('',#24628,0.165);
#9186=CIRCLE('',#24629,0.165);
#9187=CIRCLE('',#24632,0.165);
#9188=CIRCLE('',#24633,0.165);
#9189=CIRCLE('',#24636,0.165);
#9190=CIRCLE('',#24637,0.165);
#9191=CIRCLE('',#24640,1.11);
#9192=CIRCLE('',#24641,1.11);
#9193=CIRCLE('',#24651,0.21);
#9194=CIRCLE('',#24653,0.21);
#9195=CIRCLE('',#24654,0.21);
#9196=CIRCLE('',#24655,0.21);
#9197=CIRCLE('',#24657,0.21);
#9198=CIRCLE('',#24659,0.21);
#9199=CIRCLE('',#24660,0.21);
#9200=CIRCLE('',#24661,0.21);
#9201=CIRCLE('',#24663,0.21);
#9202=CIRCLE('',#24665,0.21);
#9203=CIRCLE('',#24666,0.21);
#9204=CIRCLE('',#24667,0.21);
#9205=CIRCLE('',#24669,0.21);
#9206=CIRCLE('',#24671,0.21);
#9207=CIRCLE('',#24672,0.21);
#9208=CIRCLE('',#24673,0.21);
#9209=CIRCLE('',#24715,0.285);
#9210=CIRCLE('',#24716,0.265);
#9211=CIRCLE('',#24718,0.265);
#9212=CIRCLE('',#24720,0.5);
#9213=CIRCLE('',#24722,0.5);
#9214=CIRCLE('',#24734,0.25);
#9215=CIRCLE('',#24735,0.24505);
#9216=CIRCLE('',#24737,0.25);
#9217=CIRCLE('',#24740,0.375);
#9218=CIRCLE('',#24742,0.425);
#9219=CIRCLE('',#24744,0.425);
#9220=CIRCLE('',#24746,0.395);
#9221=CIRCLE('',#24748,0.27);
#9222=CIRCLE('',#24750,0.24505);
#9223=CIRCLE('',#24754,0.457875);
#9224=CIRCLE('',#24763,0.457875);
#9225=CIRCLE('',#24765,0.625);
#9226=CIRCLE('',#24774,0.625);
#9227=CIRCLE('',#24777,1.9);
#9228=CIRCLE('',#24778,0.457875);
#9229=CIRCLE('',#24779,0.225);
#9230=CIRCLE('',#24780,0.225);
#9231=CIRCLE('',#24781,0.225);
#9232=CIRCLE('',#24783,0.225);
#9233=CIRCLE('',#24785,0.225);
#9234=CIRCLE('',#24787,0.225);
#9235=CIRCLE('',#24790,1.9);
#9236=CIRCLE('',#24791,1.1);
#9237=CIRCLE('',#24795,1.1);
#9238=CIRCLE('',#24799,0.3);
#9239=CIRCLE('',#24801,0.35);
#9240=CIRCLE('',#24803,0.35);
#9241=CIRCLE('',#24805,0.32);
#9242=CIRCLE('',#24807,0.22);
#9243=CIRCLE('',#24809,0.1954);
#9244=CIRCLE('',#24811,0.1954);
#9245=CIRCLE('',#24813,0.16);
#9246=CIRCLE('',#24825,0.375);
#9247=CIRCLE('',#24827,0.425);
#9248=CIRCLE('',#24829,0.425);
#9249=CIRCLE('',#24831,0.395);
#9250=CIRCLE('',#24833,0.27);
#9251=CIRCLE('',#24835,0.24505);
#9252=CIRCLE('',#24837,0.24505);
#9253=CIRCLE('',#24839,0.2);
#9254=CIRCLE('',#24872,0.5941);
#9255=CIRCLE('',#24936,0.415875);
#9256=CIRCLE('',#24938,0.415875);
#9257=CIRCLE('',#25001,0.6);
#9258=CIRCLE('',#25002,0.415875);
#9259=CIRCLE('',#25004,0.6);
#9260=CIRCLE('',#25009,1.);
#9261=CIRCLE('',#25013,1.);
#9262=CIRCLE('',#25015,1.);
#9263=CIRCLE('',#25016,1.);
#9264=CIRCLE('',#25019,1.35);
#9265=CIRCLE('',#25020,0.5941);
#9266=CIRCLE('',#25022,1.35);
#9267=CIRCLE('',#25027,1.01);
#9268=CIRCLE('',#25028,1.01);
#9269=CIRCLE('',#25030,1.35);
#9270=CIRCLE('',#25031,1.35);
#9271=CIRCLE('',#25036,0.210000000000001);
#9272=CIRCLE('',#25038,0.210000000000001);
#9273=CIRCLE('',#25041,1.005);
#9274=CIRCLE('',#25042,1.005);
#9275=CIRCLE('',#25044,1.5);
#9276=CIRCLE('',#25045,1.5);
#9277=CIRCLE('',#25050,0.25);
#9278=CIRCLE('',#25051,0.25);
#9279=CIRCLE('',#25053,0.210000000000001);
#9280=CIRCLE('',#25055,0.210000000000001);
#9281=CIRCLE('',#25061,3.5);
#9282=CIRCLE('',#25062,1.);
#9283=CIRCLE('',#25064,3.5);
#9284=CIRCLE('',#25065,1.5);
#9285=CIRCLE('',#25068,1.);
#9286=CIRCLE('',#25070,1.5);
#9287=CIRCLE('',#25074,0.33);
#9288=CIRCLE('',#25075,0.33);
#9289=CIRCLE('',#25077,0.4);
#9290=CIRCLE('',#25078,0.4);
#9291=CIRCLE('',#25083,0.405);
#9292=CIRCLE('',#25084,0.405);
#9293=CIRCLE('',#25086,0.9);
#9294=CIRCLE('',#25087,0.9);
#9295=CIRCLE('',#25110,0.22);
#9296=CIRCLE('',#25112,0.24505);
#9297=CIRCLE('',#25114,0.24505);
#9298=CIRCLE('',#25116,0.175);
#9299=CIRCLE('',#25120,0.32);
#9300=CIRCLE('',#25121,0.32);
#9301=CIRCLE('',#25123,0.6);
#9302=CIRCLE('',#25124,0.6);
#9303=CIRCLE('',#25129,0.45);
#9304=CIRCLE('',#25131,0.5);
#9305=CIRCLE('',#25133,0.5);
#9306=CIRCLE('',#25135,0.47);
#9307=CIRCLE('',#25137,0.32);
#9308=CIRCLE('',#25139,0.2942);
#9309=CIRCLE('',#25141,0.2942);
#9310=CIRCLE('',#25143,0.24);
#9311=CIRCLE('',#25204,0.550000000000001);
#9312=CIRCLE('',#25205,0.550000000000001);
#9313=CIRCLE('',#25208,0.550000000000001);
#9314=CIRCLE('',#25209,0.550000000000001);
#9315=CIRCLE('',#25212,0.550000000000001);
#9316=CIRCLE('',#25213,0.550000000000001);
#9317=CIRCLE('',#25216,0.550000000000001);
#9318=CIRCLE('',#25217,0.550000000000001);
#9319=CIRCLE('',#25220,0.550000000000001);
#9320=CIRCLE('',#25221,0.550000000000001);
#9321=CIRCLE('',#25224,0.550000000000001);
#9322=CIRCLE('',#25225,0.550000000000001);
#9323=CIRCLE('',#25228,0.550000000000001);
#9324=CIRCLE('',#25229,0.550000000000001);
#9325=CIRCLE('',#25232,0.550000000000001);
#9326=CIRCLE('',#25233,0.550000000000001);
#9327=CIRCLE('',#25236,0.5);
#9328=CIRCLE('',#25237,0.5);
#9329=CIRCLE('',#25239,0.275);
#9330=CIRCLE('',#25241,0.5);
#9331=CIRCLE('',#25242,0.5);
#9332=CIRCLE('',#25244,0.274999999999999);
#9333=CIRCLE('',#25246,0.5);
#9334=CIRCLE('',#25247,0.5);
#9335=CIRCLE('',#25249,0.275);
#9336=CIRCLE('',#25251,0.5);
#9337=CIRCLE('',#25252,0.5);
#9338=CIRCLE('',#25254,0.274999999999999);
#9339=CIRCLE('',#25256,0.275);
#9340=CIRCLE('',#25258,0.274999999999999);
#9341=CIRCLE('',#25260,0.275);
#9342=CIRCLE('',#25262,0.274999999999999);
#9343=CIRCLE('',#25264,0.210000000000001);
#9344=CIRCLE('',#25265,0.210000000000001);
#9345=CIRCLE('',#25267,0.21);
#9346=CIRCLE('',#25268,0.21);
#9347=CIRCLE('',#25270,0.329999999999998);
#9348=CIRCLE('',#25271,0.329999999999998);
#9349=CIRCLE('',#25273,0.329999999999998);
#9350=CIRCLE('',#25274,0.329999999999998);
#9351=CIRCLE('',#25276,0.275);
#9352=CIRCLE('',#25277,0.275);
#9353=CIRCLE('',#25279,0.275);
#9354=CIRCLE('',#25280,0.275);
#9355=CIRCLE('',#25282,0.210000000000001);
#9356=CIRCLE('',#25283,0.210000000000001);
#9357=CIRCLE('',#25285,0.21);
#9358=CIRCLE('',#25286,0.21);
#9359=CIRCLE('',#25288,0.21);
#9360=CIRCLE('',#25289,0.21);
#9361=CIRCLE('',#25291,0.210000000000001);
#9362=CIRCLE('',#25292,0.210000000000001);
#9363=CIRCLE('',#25301,0.5);
#9364=CIRCLE('',#25302,0.5);
#9365=CIRCLE('',#25304,0.5);
#9366=CIRCLE('',#25305,0.5);
#9367=CIRCLE('',#25307,0.164999999999999);
#9368=CIRCLE('',#25308,0.164999999999999);
#9369=CIRCLE('',#25310,0.164999999999999);
#9370=CIRCLE('',#25311,0.164999999999999);
#9371=CIRCLE('',#25313,0.165);
#9372=CIRCLE('',#25314,0.165);
#9373=CIRCLE('',#25316,0.164999999999999);
#9374=CIRCLE('',#25317,0.164999999999999);
#9375=CIRCLE('',#25319,0.5);
#9376=CIRCLE('',#25320,0.5);
#9377=CIRCLE('',#25322,0.274999999999999);
#9378=CIRCLE('',#25324,0.5);
#9379=CIRCLE('',#25325,0.5);
#9380=CIRCLE('',#25327,0.275);
#9381=CIRCLE('',#25329,0.5);
#9382=CIRCLE('',#25330,0.5);
#9383=CIRCLE('',#25332,0.275);
#9384=CIRCLE('',#25334,0.5);
#9385=CIRCLE('',#25335,0.5);
#9386=CIRCLE('',#25337,0.274999999999999);
#9387=CIRCLE('',#25340,0.274999999999999);
#9388=CIRCLE('',#25342,0.275);
#9389=CIRCLE('',#25344,0.275);
#9390=CIRCLE('',#25346,0.274999999999999);
#9391=CIRCLE('',#25354,0.165);
#9392=CIRCLE('',#25355,0.165);
#9393=CIRCLE('',#25357,0.165);
#9394=CIRCLE('',#25358,0.165);
#9395=CIRCLE('',#25360,0.165);
#9396=CIRCLE('',#25361,0.165);
#9397=CIRCLE('',#25363,1.6);
#9398=CIRCLE('',#25364,1.6);
#9399=CIRCLE('',#25366,1.4);
#9400=CIRCLE('',#25368,1.4);
#9401=CIRCLE('',#25370,0.21);
#9402=CIRCLE('',#25371,0.21);
#9403=CIRCLE('',#25374,0.21);
#9404=CIRCLE('',#25375,0.21);
#9405=CIRCLE('',#25385,0.225);
#9406=CIRCLE('',#25386,0.225);
#9407=CIRCLE('',#25388,0.225);
#9408=CIRCLE('',#25389,0.225);
#9409=CIRCLE('',#25391,0.225);
#9410=CIRCLE('',#25392,0.225);
#9411=CIRCLE('',#25394,1.59);
#9412=CIRCLE('',#25395,1.59);
#9413=CIRCLE('',#25397,1.2);
#9414=CIRCLE('',#25399,1.2);
#9415=CIRCLE('',#25401,2.4);
#9416=CIRCLE('',#25402,2.4);
#9417=CIRCLE('',#25407,0.165);
#9418=CIRCLE('',#25408,0.165);
#9419=CIRCLE('',#25410,0.165);
#9420=CIRCLE('',#25411,0.165);
#9421=CIRCLE('',#25413,0.165);
#9422=CIRCLE('',#25414,0.165);
#9423=CIRCLE('',#25416,2.35);
#9424=CIRCLE('',#25417,2.35);
#9425=CIRCLE('',#25419,2.15);
#9426=CIRCLE('',#25421,2.15);
#9427=CIRCLE('',#25423,0.25);
#9428=CIRCLE('',#25424,0.25);
#9429=CIRCLE('',#25427,0.25);
#9430=CIRCLE('',#25428,0.25);
#9431=CIRCLE('',#25438,0.225);
#9432=CIRCLE('',#25439,0.225);
#9433=CIRCLE('',#25441,0.225);
#9434=CIRCLE('',#25442,0.225);
#9435=CIRCLE('',#25444,0.225);
#9436=CIRCLE('',#25445,0.225);
#9437=CIRCLE('',#25448,3.);
#9438=CIRCLE('',#25449,2.34);
#9439=CIRCLE('',#25451,3.);
#9440=CIRCLE('',#25453,2.34);
#9441=CIRCLE('',#25455,1.8);
#9442=CIRCLE('',#25457,1.8);
#9443=CIRCLE('',#25461,0.475);
#9444=CIRCLE('',#25462,0.475);
#9445=CIRCLE('',#25464,0.275);
#9446=CIRCLE('',#25466,0.275);
#9447=CIRCLE('',#25475,0.475000000000001);
#9448=CIRCLE('',#25476,0.475000000000001);
#9449=CIRCLE('',#25478,0.274999999999999);
#9450=CIRCLE('',#25480,0.274999999999999);
#9451=CIRCLE('',#25489,0.375);
#9452=CIRCLE('',#25490,0.375);
#9453=CIRCLE('',#25492,0.225);
#9454=CIRCLE('',#25494,0.375);
#9455=CIRCLE('',#25495,0.375);
#9456=CIRCLE('',#25497,0.225);
#9457=CIRCLE('',#25499,0.375);
#9458=CIRCLE('',#25500,0.375);
#9459=CIRCLE('',#25502,0.225);
#9460=CIRCLE('',#25504,0.375);
#9461=CIRCLE('',#25505,0.375);
#9462=CIRCLE('',#25507,0.225000000000001);
#9463=CIRCLE('',#25509,0.225);
#9464=CIRCLE('',#25511,0.225);
#9465=CIRCLE('',#25513,0.225);
#9466=CIRCLE('',#25515,0.225000000000001);
#9467=CIRCLE('',#25533,1.070235);
#9468=CIRCLE('',#25534,1.070235);
#9469=CIRCLE('',#25535,0.309556);
#9470=CIRCLE('',#25536,1.070235);
#9471=CIRCLE('',#25537,1.070235);
#9472=CIRCLE('',#25539,1.070235);
#9473=CIRCLE('',#25541,0.6);
#9474=CIRCLE('',#25542,0.6);
#9475=CIRCLE('',#25544,0.66);
#9476=CIRCLE('',#25547,1.070235);
#9477=CIRCLE('',#25549,0.66);
#9478=CIRCLE('',#25553,1.129765);
#9479=CIRCLE('',#25554,1.129765);
#9480=CIRCLE('',#25555,0.309556);
#9481=CIRCLE('',#25556,1.129765);
#9482=CIRCLE('',#25557,1.129765);
#9483=CIRCLE('',#25559,1.129765);
#9484=CIRCLE('',#25561,1.54);
#9485=CIRCLE('',#25562,1.129765);
#9486=CIRCLE('',#25564,1.6);
#9487=CIRCLE('',#25566,1.6);
#9488=CIRCLE('',#25568,1.54);
#9489=CIRCLE('',#25573,0.29765);
#9490=CIRCLE('',#25575,0.29765);
#9491=CIRCLE('',#25577,0.29765);
#9492=CIRCLE('',#25579,0.29765);
#9493=CIRCLE('',#25581,0.29765);
#9494=CIRCLE('',#25583,0.29765);
#9495=CIRCLE('',#25585,0.29765);
#9496=CIRCLE('',#25588,0.303778037777585);
#9497=CIRCLE('',#25589,0.303778037777585);
#9498=CIRCLE('',#25591,1.123812);
#9499=CIRCLE('',#25592,1.123812);
#9500=CIRCLE('',#25593,1.123812);
#9501=CIRCLE('',#25594,1.123812);
#9502=CIRCLE('',#25595,1.123812);
#9503=CIRCLE('',#25596,1.123812);
#9504=CIRCLE('',#25597,1.123812);
#9505=CIRCLE('',#25598,1.123812);
#9506=CIRCLE('',#25599,1.123812);
#9507=CIRCLE('',#25601,1.076188);
#9508=CIRCLE('',#25602,0.303778037777585);
#9509=CIRCLE('',#25604,0.303778037777585);
#9510=CIRCLE('',#25606,1.076188);
#9511=CIRCLE('',#25607,0.303778037777585);
#9512=CIRCLE('',#25609,0.303778037777585);
#9513=CIRCLE('',#25611,1.076188);
#9514=CIRCLE('',#25612,1.076188);
#9515=CIRCLE('',#25613,0.303778037777585);
#9516=CIRCLE('',#25615,0.303778037777585);
#9517=CIRCLE('',#25617,1.076188);
#9518=CIRCLE('',#25618,0.303778037777585);
#9519=CIRCLE('',#25620,0.303778037777585);
#9520=CIRCLE('',#25622,1.076188);
#9521=CIRCLE('',#25623,0.303778037777585);
#9522=CIRCLE('',#25625,0.303778037777585);
#9523=CIRCLE('',#25627,1.076188);
#9524=CIRCLE('',#25628,1.076188);
#9525=CIRCLE('',#25629,1.076188);
#9526=CIRCLE('',#25631,0.303778037777585);
#9527=CIRCLE('',#25633,0.303778037777585);
#9528=CIRCLE('',#25638,1.119765);
#9529=CIRCLE('',#25639,1.085235);
#9530=CIRCLE('',#25641,1.119765);
#9531=CIRCLE('',#25643,1.085235);
#9532=CIRCLE('',#25646,1.119765);
#9533=CIRCLE('',#25647,1.085235);
#9534=CIRCLE('',#25649,1.119765);
#9535=CIRCLE('',#25651,1.085235);
#9536=CIRCLE('',#25661,1.63531);
#9537=CIRCLE('',#25662,1.63531);
#9538=CIRCLE('',#25663,0.412776);
#9539=CIRCLE('',#25664,1.63531);
#9540=CIRCLE('',#25665,1.63531);
#9541=CIRCLE('',#25667,1.63531);
#9542=CIRCLE('',#25669,1.);
#9543=CIRCLE('',#25670,1.);
#9544=CIRCLE('',#25672,1.1);
#9545=CIRCLE('',#25675,1.63531);
#9546=CIRCLE('',#25677,1.1);
#9547=CIRCLE('',#25681,1.71469);
#9548=CIRCLE('',#25682,1.71469);
#9549=CIRCLE('',#25683,0.412776);
#9550=CIRCLE('',#25684,1.71469);
#9551=CIRCLE('',#25685,1.71469);
#9552=CIRCLE('',#25687,1.71469);
#9553=CIRCLE('',#25689,2.25);
#9554=CIRCLE('',#25690,1.71469);
#9555=CIRCLE('',#25692,2.35);
#9556=CIRCLE('',#25694,2.35);
#9557=CIRCLE('',#25696,2.25);
#9558=CIRCLE('',#25701,0.3969);
#9559=CIRCLE('',#25703,0.3969);
#9560=CIRCLE('',#25705,0.3969);
#9561=CIRCLE('',#25707,0.3969);
#9562=CIRCLE('',#25709,0.3969);
#9563=CIRCLE('',#25711,0.3969);
#9564=CIRCLE('',#25713,0.3969);
#9565=CIRCLE('',#25715,0.3969);
#9566=CIRCLE('',#25718,0.405071403305639);
#9567=CIRCLE('',#25719,0.405071403305639);
#9568=CIRCLE('',#25721,1.706752);
#9569=CIRCLE('',#25722,1.706752);
#9570=CIRCLE('',#25723,1.706752);
#9571=CIRCLE('',#25724,1.706752);
#9572=CIRCLE('',#25725,1.706752);
#9573=CIRCLE('',#25726,1.706752);
#9574=CIRCLE('',#25727,1.706752);
#9575=CIRCLE('',#25728,1.706752);
#9576=CIRCLE('',#25729,1.706752);
#9577=CIRCLE('',#25731,1.643248);
#9578=CIRCLE('',#25732,0.405071403305639);
#9579=CIRCLE('',#25734,0.405071403305639);
#9580=CIRCLE('',#25736,1.643248);
#9581=CIRCLE('',#25737,0.405071403305639);
#9582=CIRCLE('',#25739,0.405071403305639);
#9583=CIRCLE('',#25741,1.643248);
#9584=CIRCLE('',#25742,0.405071403305639);
#9585=CIRCLE('',#25744,0.405071403305639);
#9586=CIRCLE('',#25746,1.643248);
#9587=CIRCLE('',#25747,0.405071403305639);
#9588=CIRCLE('',#25749,0.405071403305639);
#9589=CIRCLE('',#25751,1.643248);
#9590=CIRCLE('',#25752,0.405071403305639);
#9591=CIRCLE('',#25754,0.405071403305639);
#9592=CIRCLE('',#25756,1.643248);
#9593=CIRCLE('',#25757,0.405071403305639);
#9594=CIRCLE('',#25759,0.405071403305639);
#9595=CIRCLE('',#25761,1.643248);
#9596=CIRCLE('',#25762,1.643248);
#9597=CIRCLE('',#25763,1.643248);
#9598=CIRCLE('',#25765,0.405071403305639);
#9599=CIRCLE('',#25767,0.405071403305639);
#9600=CIRCLE('',#25772,1.70469);
#9601=CIRCLE('',#25773,1.65031);
#9602=CIRCLE('',#25775,1.70469);
#9603=CIRCLE('',#25777,1.65031);
#9604=CIRCLE('',#25780,1.70469);
#9605=CIRCLE('',#25781,1.65031);
#9606=CIRCLE('',#25783,1.70469);
#9607=CIRCLE('',#25785,1.65031);
#9608=CIRCLE('',#25802,0.24505);
#9609=CIRCLE('',#25804,0.375);
#9610=CIRCLE('',#25806,0.425);
#9611=CIRCLE('',#25808,0.425);
#9612=CIRCLE('',#25810,0.395);
#9613=CIRCLE('',#25812,0.27);
#9614=CIRCLE('',#25814,0.24505);
#9615=CIRCLE('',#25819,0.275);
#9616=CIRCLE('',#25820,0.275);
#9617=CIRCLE('',#25822,0.275);
#9618=CIRCLE('',#25823,0.275);
#9619=CIRCLE('',#25825,0.275);
#9620=CIRCLE('',#25826,0.275);
#9621=CIRCLE('',#25828,0.275);
#9622=CIRCLE('',#25829,0.275);
#9623=CIRCLE('',#25838,0.275);
#9624=CIRCLE('',#25839,0.275);
#9625=CIRCLE('',#25841,0.275);
#9626=CIRCLE('',#25842,0.275);
#9627=CIRCLE('',#25844,0.275);
#9628=CIRCLE('',#25845,0.275);
#9629=CIRCLE('',#25847,0.275);
#9630=CIRCLE('',#25848,0.275);
#9631=CIRCLE('',#25850,0.275);
#9632=CIRCLE('',#25851,0.275);
#9633=CIRCLE('',#25853,0.275);
#9634=CIRCLE('',#25854,0.275);
#9635=CIRCLE('',#25856,0.275);
#9636=CIRCLE('',#25857,0.275);
#9637=CIRCLE('',#25859,0.275);
#9638=CIRCLE('',#25860,0.275);
#9639=CIRCLE('',#25869,0.210000000000001);
#9640=CIRCLE('',#25870,0.210000000000001);
#9641=CIRCLE('',#25873,0.210000000000001);
#9642=CIRCLE('',#25874,0.210000000000001);
#9643=CIRCLE('',#25877,0.210000000000001);
#9644=CIRCLE('',#25878,0.210000000000001);
#9645=CIRCLE('',#25881,0.210000000000001);
#9646=CIRCLE('',#25882,0.210000000000001);
#9647=CIRCLE('',#25885,0.165);
#9648=CIRCLE('',#25886,0.165);
#9649=CIRCLE('',#25889,0.165);
#9650=CIRCLE('',#25890,0.165);
#9651=CIRCLE('',#25893,0.165);
#9652=CIRCLE('',#25894,0.165);
#9653=CIRCLE('',#25897,1.11);
#9654=CIRCLE('',#25898,1.11);
#9655=CIRCLE('',#25908,0.21);
#9656=CIRCLE('',#25910,0.21);
#9657=CIRCLE('',#25911,0.21);
#9658=CIRCLE('',#25912,0.21);
#9659=CIRCLE('',#25914,0.21);
#9660=CIRCLE('',#25916,0.21);
#9661=CIRCLE('',#25917,0.21);
#9662=CIRCLE('',#25918,0.21);
#9663=CIRCLE('',#25920,0.21);
#9664=CIRCLE('',#25922,0.21);
#9665=CIRCLE('',#25923,0.21);
#9666=CIRCLE('',#25924,0.21);
#9667=CIRCLE('',#25926,0.21);
#9668=CIRCLE('',#25928,0.21);
#9669=CIRCLE('',#25929,0.21);
#9670=CIRCLE('',#25930,0.21);
#9671=CIRCLE('',#25972,0.285);
#9672=CIRCLE('',#25973,0.265);
#9673=CIRCLE('',#25975,0.265);
#9674=CIRCLE('',#25977,0.5);
#9675=CIRCLE('',#25979,0.5);
#9676=CIRCLE('',#25991,0.25);
#9677=CIRCLE('',#25992,0.24505);
#9678=CIRCLE('',#25994,0.25);
#9679=CIRCLE('',#25997,0.375);
#9680=CIRCLE('',#25999,0.425);
#9681=CIRCLE('',#26001,0.425);
#9682=CIRCLE('',#26003,0.395);
#9683=CIRCLE('',#26005,0.27);
#9684=CIRCLE('',#26007,0.24505);
#9685=CIRCLE('',#26011,0.457875);
#9686=CIRCLE('',#26020,0.457875);
#9687=CIRCLE('',#26022,0.625);
#9688=CIRCLE('',#26031,0.625);
#9689=CIRCLE('',#26034,1.9);
#9690=CIRCLE('',#26035,0.457875);
#9691=CIRCLE('',#26036,0.225);
#9692=CIRCLE('',#26037,0.225);
#9693=CIRCLE('',#26038,0.225);
#9694=CIRCLE('',#26040,0.225);
#9695=CIRCLE('',#26042,0.225);
#9696=CIRCLE('',#26044,0.225);
#9697=CIRCLE('',#26047,1.9);
#9698=CIRCLE('',#26048,1.1);
#9699=CIRCLE('',#26052,1.1);
#9700=CIRCLE('',#26056,0.3);
#9701=CIRCLE('',#26058,0.35);
#9702=CIRCLE('',#26060,0.35);
#9703=CIRCLE('',#26062,0.32);
#9704=CIRCLE('',#26064,0.22);
#9705=CIRCLE('',#26066,0.1954);
#9706=CIRCLE('',#26068,0.1954);
#9707=CIRCLE('',#26070,0.16);
#9708=CIRCLE('',#26082,0.375);
#9709=CIRCLE('',#26084,0.425);
#9710=CIRCLE('',#26086,0.425);
#9711=CIRCLE('',#26088,0.395);
#9712=CIRCLE('',#26090,0.27);
#9713=CIRCLE('',#26092,0.24505);
#9714=CIRCLE('',#26094,0.24505);
#9715=CIRCLE('',#26096,0.2);
#9716=CIRCLE('',#26129,0.5941);
#9717=CIRCLE('',#26193,0.415875);
#9718=CIRCLE('',#26195,0.415875);
#9719=CIRCLE('',#26258,0.6);
#9720=CIRCLE('',#26259,0.415875);
#9721=CIRCLE('',#26261,0.6);
#9722=CIRCLE('',#26266,1.);
#9723=CIRCLE('',#26270,1.);
#9724=CIRCLE('',#26272,1.);
#9725=CIRCLE('',#26273,1.);
#9726=CIRCLE('',#26276,1.35);
#9727=CIRCLE('',#26277,0.5941);
#9728=CIRCLE('',#26279,1.35);
#9729=CIRCLE('',#26284,1.01);
#9730=CIRCLE('',#26285,1.01);
#9731=CIRCLE('',#26287,1.35);
#9732=CIRCLE('',#26288,1.35);
#9733=CIRCLE('',#26293,0.210000000000001);
#9734=CIRCLE('',#26295,0.210000000000001);
#9735=CIRCLE('',#26298,1.005);
#9736=CIRCLE('',#26299,1.005);
#9737=CIRCLE('',#26301,1.5);
#9738=CIRCLE('',#26302,1.5);
#9739=CIRCLE('',#26307,0.25);
#9740=CIRCLE('',#26308,0.25);
#9741=CIRCLE('',#26310,0.210000000000001);
#9742=CIRCLE('',#26312,0.210000000000001);
#9743=CIRCLE('',#26318,3.5);
#9744=CIRCLE('',#26319,1.);
#9745=CIRCLE('',#26321,3.5);
#9746=CIRCLE('',#26322,1.5);
#9747=CIRCLE('',#26325,1.);
#9748=CIRCLE('',#26327,1.5);
#9749=CIRCLE('',#26331,0.33);
#9750=CIRCLE('',#26332,0.33);
#9751=CIRCLE('',#26334,0.4);
#9752=CIRCLE('',#26335,0.4);
#9753=CIRCLE('',#26340,0.405);
#9754=CIRCLE('',#26341,0.405);
#9755=CIRCLE('',#26343,0.9);
#9756=CIRCLE('',#26344,0.9);
#9757=CIRCLE('',#26367,0.22);
#9758=CIRCLE('',#26369,0.24505);
#9759=CIRCLE('',#26371,0.24505);
#9760=CIRCLE('',#26373,0.175);
#9761=CIRCLE('',#26377,0.32);
#9762=CIRCLE('',#26378,0.32);
#9763=CIRCLE('',#26380,0.6);
#9764=CIRCLE('',#26381,0.6);
#9765=CIRCLE('',#26386,0.45);
#9766=CIRCLE('',#26388,0.5);
#9767=CIRCLE('',#26390,0.5);
#9768=CIRCLE('',#26392,0.47);
#9769=CIRCLE('',#26394,0.32);
#9770=CIRCLE('',#26396,0.2942);
#9771=CIRCLE('',#26398,0.2942);
#9772=CIRCLE('',#26400,0.24);
#9773=VERTEX_POINT('',#32875);
#9774=VERTEX_POINT('',#32877);
#9775=VERTEX_POINT('',#32881);
#9776=VERTEX_POINT('',#32883);
#9777=VERTEX_POINT('',#32887);
#9778=VERTEX_POINT('',#32889);
#9779=VERTEX_POINT('',#32893);
#9780=VERTEX_POINT('',#32895);
#9781=VERTEX_POINT('',#32899);
#9782=VERTEX_POINT('',#32901);
#9783=VERTEX_POINT('',#32905);
#9784=VERTEX_POINT('',#32907);
#9785=VERTEX_POINT('',#32911);
#9786=VERTEX_POINT('',#32913);
#9787=VERTEX_POINT('',#32917);
#9788=VERTEX_POINT('',#32919);
#9789=VERTEX_POINT('',#32923);
#9790=VERTEX_POINT('',#32925);
#9791=VERTEX_POINT('',#32929);
#9792=VERTEX_POINT('',#32931);
#9793=VERTEX_POINT('',#32935);
#9794=VERTEX_POINT('',#32936);
#9795=VERTEX_POINT('',#32938);
#9796=VERTEX_POINT('',#32940);
#9797=VERTEX_POINT('',#32944);
#9798=VERTEX_POINT('',#32946);
#9799=VERTEX_POINT('',#32950);
#9800=VERTEX_POINT('',#32952);
#9801=VERTEX_POINT('',#32962);
#9802=VERTEX_POINT('',#32963);
#9803=VERTEX_POINT('',#32965);
#9804=VERTEX_POINT('',#32967);
#9805=VERTEX_POINT('',#32971);
#9806=VERTEX_POINT('',#32973);
#9807=VERTEX_POINT('',#32977);
#9808=VERTEX_POINT('',#32979);
#9809=VERTEX_POINT('',#32989);
#9810=VERTEX_POINT('',#32990);
#9811=VERTEX_POINT('',#32992);
#9812=VERTEX_POINT('',#32994);
#9813=VERTEX_POINT('',#32998);
#9814=VERTEX_POINT('',#33000);
#9815=VERTEX_POINT('',#33004);
#9816=VERTEX_POINT('',#33006);
#9817=VERTEX_POINT('',#33016);
#9818=VERTEX_POINT('',#33017);
#9819=VERTEX_POINT('',#33019);
#9820=VERTEX_POINT('',#33021);
#9821=VERTEX_POINT('',#33025);
#9822=VERTEX_POINT('',#33026);
#9823=VERTEX_POINT('',#33028);
#9824=VERTEX_POINT('',#33030);
#9825=VERTEX_POINT('',#33034);
#9826=VERTEX_POINT('',#33036);
#9827=VERTEX_POINT('',#33040);
#9828=VERTEX_POINT('',#33042);
#9829=VERTEX_POINT('',#33046);
#9830=VERTEX_POINT('',#33048);
#9831=VERTEX_POINT('',#33052);
#9832=VERTEX_POINT('',#33054);
#9833=VERTEX_POINT('',#33058);
#9834=VERTEX_POINT('',#33060);
#9835=VERTEX_POINT('',#33064);
#9836=VERTEX_POINT('',#33071);
#9837=VERTEX_POINT('',#33074);
#9838=VERTEX_POINT('',#33076);
#9839=VERTEX_POINT('',#33080);
#9840=VERTEX_POINT('',#33087);
#9841=VERTEX_POINT('',#33090);
#9842=VERTEX_POINT('',#33091);
#9843=VERTEX_POINT('',#33093);
#9844=VERTEX_POINT('',#33095);
#9845=VERTEX_POINT('',#33101);
#9846=VERTEX_POINT('',#33105);
#9847=VERTEX_POINT('',#33109);
#9848=VERTEX_POINT('',#33113);
#9849=VERTEX_POINT('',#33117);
#9850=VERTEX_POINT('',#33118);
#9851=VERTEX_POINT('',#33123);
#9852=VERTEX_POINT('',#33127);
#9853=VERTEX_POINT('',#33135);
#9854=VERTEX_POINT('',#33137);
#9855=VERTEX_POINT('',#33141);
#9856=VERTEX_POINT('',#33143);
#9857=VERTEX_POINT('',#33147);
#9858=VERTEX_POINT('',#33149);
#9859=VERTEX_POINT('',#33153);
#9860=VERTEX_POINT('',#33155);
#9861=VERTEX_POINT('',#33159);
#9862=VERTEX_POINT('',#33162);
#9863=VERTEX_POINT('',#33166);
#9864=VERTEX_POINT('',#33168);
#9865=VERTEX_POINT('',#33173);
#9866=VERTEX_POINT('',#33175);
#9867=VERTEX_POINT('',#33180);
#9868=VERTEX_POINT('',#33181);
#9869=VERTEX_POINT('',#33183);
#9870=VERTEX_POINT('',#33185);
#9871=VERTEX_POINT('',#33189);
#9872=VERTEX_POINT('',#33191);
#9873=VERTEX_POINT('',#33195);
#9874=VERTEX_POINT('',#33197);
#9875=VERTEX_POINT('',#33207);
#9876=VERTEX_POINT('',#33209);
#9877=VERTEX_POINT('',#33213);
#9878=VERTEX_POINT('',#33215);
#9879=VERTEX_POINT('',#33219);
#9880=VERTEX_POINT('',#33221);
#9881=VERTEX_POINT('',#33225);
#9882=VERTEX_POINT('',#33227);
#9883=VERTEX_POINT('',#33231);
#9884=VERTEX_POINT('',#33234);
#9885=VERTEX_POINT('',#33238);
#9886=VERTEX_POINT('',#33240);
#9887=VERTEX_POINT('',#33247);
#9888=VERTEX_POINT('',#33249);
#9889=VERTEX_POINT('',#33253);
#9890=VERTEX_POINT('',#33255);
#9891=VERTEX_POINT('',#33259);
#9892=VERTEX_POINT('',#33261);
#9893=VERTEX_POINT('',#33265);
#9894=VERTEX_POINT('',#33267);
#9895=VERTEX_POINT('',#33271);
#9896=VERTEX_POINT('',#33274);
#9897=VERTEX_POINT('',#33278);
#9898=VERTEX_POINT('',#33280);
#9899=VERTEX_POINT('',#33285);
#9900=VERTEX_POINT('',#33287);
#9901=VERTEX_POINT('',#33292);
#9902=VERTEX_POINT('',#33293);
#9903=VERTEX_POINT('',#33295);
#9904=VERTEX_POINT('',#33297);
#9905=VERTEX_POINT('',#33301);
#9906=VERTEX_POINT('',#33303);
#9907=VERTEX_POINT('',#33307);
#9908=VERTEX_POINT('',#33309);
#9909=VERTEX_POINT('',#33319);
#9910=VERTEX_POINT('',#33321);
#9911=VERTEX_POINT('',#33325);
#9912=VERTEX_POINT('',#33327);
#9913=VERTEX_POINT('',#33331);
#9914=VERTEX_POINT('',#33333);
#9915=VERTEX_POINT('',#33337);
#9916=VERTEX_POINT('',#33338);
#9917=VERTEX_POINT('',#33340);
#9918=VERTEX_POINT('',#33342);
#9919=VERTEX_POINT('',#33347);
#9920=VERTEX_POINT('',#33352);
#9921=VERTEX_POINT('',#33356);
#9922=VERTEX_POINT('',#33359);
#9923=VERTEX_POINT('',#33365);
#9924=VERTEX_POINT('',#33367);
#9925=VERTEX_POINT('',#33371);
#9926=VERTEX_POINT('',#33374);
#9927=VERTEX_POINT('',#33378);
#9928=VERTEX_POINT('',#33379);
#9929=VERTEX_POINT('',#33381);
#9930=VERTEX_POINT('',#33383);
#9931=VERTEX_POINT('',#33387);
#9932=VERTEX_POINT('',#33389);
#9933=VERTEX_POINT('',#33393);
#9934=VERTEX_POINT('',#33395);
#9935=VERTEX_POINT('',#33405);
#9936=VERTEX_POINT('',#33407);
#9937=VERTEX_POINT('',#33411);
#9938=VERTEX_POINT('',#33414);
#9939=VERTEX_POINT('',#33418);
#9940=VERTEX_POINT('',#33419);
#9941=VERTEX_POINT('',#33421);
#9942=VERTEX_POINT('',#33423);
#9943=VERTEX_POINT('',#33427);
#9944=VERTEX_POINT('',#33429);
#9945=VERTEX_POINT('',#33433);
#9946=VERTEX_POINT('',#33435);
#9947=VERTEX_POINT('',#33445);
#9948=VERTEX_POINT('',#33447);
#9949=VERTEX_POINT('',#33451);
#9950=VERTEX_POINT('',#33454);
#9951=VERTEX_POINT('',#33456);
#9952=VERTEX_POINT('',#33460);
#9953=VERTEX_POINT('',#33463);
#9954=VERTEX_POINT('',#33465);
#9955=VERTEX_POINT('',#33469);
#9956=VERTEX_POINT('',#33472);
#9957=VERTEX_POINT('',#33474);
#9958=VERTEX_POINT('',#33478);
#9959=VERTEX_POINT('',#33481);
#9960=VERTEX_POINT('',#33485);
#9961=VERTEX_POINT('',#33489);
#9962=VERTEX_POINT('',#33493);
#9963=VERTEX_POINT('',#33497);
#9964=VERTEX_POINT('',#33498);
#9965=VERTEX_POINT('',#33500);
#9966=VERTEX_POINT('',#33502);
#9967=VERTEX_POINT('',#33506);
#9968=VERTEX_POINT('',#33508);
#9969=VERTEX_POINT('',#33512);
#9970=VERTEX_POINT('',#33514);
#9971=VERTEX_POINT('',#33518);
#9972=VERTEX_POINT('',#33520);
#9973=VERTEX_POINT('',#33524);
#9974=VERTEX_POINT('',#33526);
#9975=VERTEX_POINT('',#33530);
#9976=VERTEX_POINT('',#33532);
#9977=VERTEX_POINT('',#33536);
#9978=VERTEX_POINT('',#33538);
#9979=VERTEX_POINT('',#33542);
#9980=VERTEX_POINT('',#33544);
#9981=VERTEX_POINT('',#33548);
#9982=VERTEX_POINT('',#33550);
#9983=VERTEX_POINT('',#33554);
#9984=VERTEX_POINT('',#33556);
#9985=VERTEX_POINT('',#33560);
#9986=VERTEX_POINT('',#33562);
#9987=VERTEX_POINT('',#33573);
#9988=VERTEX_POINT('',#33574);
#9989=VERTEX_POINT('',#33577);
#9990=VERTEX_POINT('',#33579);
#9991=VERTEX_POINT('',#33583);
#9992=VERTEX_POINT('',#33587);
#9993=VERTEX_POINT('',#33589);
#9994=VERTEX_POINT('',#33593);
#9995=VERTEX_POINT('',#33598);
#9996=VERTEX_POINT('',#33602);
#9997=VERTEX_POINT('',#33608);
#9998=VERTEX_POINT('',#33609);
#9999=VERTEX_POINT('',#33612);
#10000=VERTEX_POINT('',#33614);
#10001=VERTEX_POINT('',#33618);
#10002=VERTEX_POINT('',#33622);
#10003=VERTEX_POINT('',#33624);
#10004=VERTEX_POINT('',#33627);
#10005=VERTEX_POINT('',#33631);
#10006=VERTEX_POINT('',#33635);
#10007=VERTEX_POINT('',#33643);
#10008=VERTEX_POINT('',#33644);
#10009=VERTEX_POINT('',#33647);
#10010=VERTEX_POINT('',#33648);
#10011=VERTEX_POINT('',#33651);
#10012=VERTEX_POINT('',#33652);
#10013=VERTEX_POINT('',#33655);
#10014=VERTEX_POINT('',#33656);
#10015=VERTEX_POINT('',#33659);
#10016=VERTEX_POINT('',#33660);
#10017=VERTEX_POINT('',#33663);
#10018=VERTEX_POINT('',#33664);
#10019=VERTEX_POINT('',#33667);
#10020=VERTEX_POINT('',#33668);
#10021=VERTEX_POINT('',#33672);
#10022=VERTEX_POINT('',#33673);
#10023=VERTEX_POINT('',#33696);
#10024=VERTEX_POINT('',#33698);
#10025=VERTEX_POINT('',#33723);
#10026=VERTEX_POINT('',#33725);
#10027=VERTEX_POINT('',#33748);
#10028=VERTEX_POINT('',#33750);
#10029=VERTEX_POINT('',#33773);
#10030=VERTEX_POINT('',#33775);
#10031=VERTEX_POINT('',#33778);
#10032=VERTEX_POINT('',#33780);
#10033=VERTEX_POINT('',#33803);
#10034=VERTEX_POINT('',#33805);
#10035=VERTEX_POINT('',#33828);
#10036=VERTEX_POINT('',#33830);
#10037=VERTEX_POINT('',#33853);
#10038=VERTEX_POINT('',#33855);
#10039=VERTEX_POINT('',#33880);
#10040=VERTEX_POINT('',#33884);
#10041=VERTEX_POINT('',#33909);
#10042=VERTEX_POINT('',#33913);
#10043=VERTEX_POINT('',#33938);
#10044=VERTEX_POINT('',#33940);
#10045=VERTEX_POINT('',#33944);
#10046=VERTEX_POINT('',#33969);
#10047=VERTEX_POINT('',#33973);
#10048=VERTEX_POINT('',#33998);
#10049=VERTEX_POINT('',#34002);
#10050=VERTEX_POINT('',#34027);
#10051=VERTEX_POINT('',#34030);
#10052=VERTEX_POINT('',#34032);
#10053=VERTEX_POINT('',#34064);
#10054=VERTEX_POINT('',#34066);
#10055=VERTEX_POINT('',#34069);
#10056=VERTEX_POINT('',#34073);
#10057=VERTEX_POINT('',#34078);
#10058=VERTEX_POINT('',#34080);
#10059=VERTEX_POINT('',#34083);
#10060=VERTEX_POINT('',#34087);
#10061=VERTEX_POINT('',#34099);
#10062=VERTEX_POINT('',#34100);
#10063=VERTEX_POINT('',#34103);
#10064=VERTEX_POINT('',#34105);
#10065=VERTEX_POINT('',#34109);
#10066=VERTEX_POINT('',#34113);
#10067=VERTEX_POINT('',#34115);
#10068=VERTEX_POINT('',#34119);
#10069=VERTEX_POINT('',#34124);
#10070=VERTEX_POINT('',#34128);
#10071=VERTEX_POINT('',#34134);
#10072=VERTEX_POINT('',#34135);
#10073=VERTEX_POINT('',#34138);
#10074=VERTEX_POINT('',#34140);
#10075=VERTEX_POINT('',#34144);
#10076=VERTEX_POINT('',#34148);
#10077=VERTEX_POINT('',#34150);
#10078=VERTEX_POINT('',#34153);
#10079=VERTEX_POINT('',#34157);
#10080=VERTEX_POINT('',#34161);
#10081=VERTEX_POINT('',#34169);
#10082=VERTEX_POINT('',#34170);
#10083=VERTEX_POINT('',#34173);
#10084=VERTEX_POINT('',#34174);
#10085=VERTEX_POINT('',#34177);
#10086=VERTEX_POINT('',#34178);
#10087=VERTEX_POINT('',#34181);
#10088=VERTEX_POINT('',#34182);
#10089=VERTEX_POINT('',#34185);
#10090=VERTEX_POINT('',#34186);
#10091=VERTEX_POINT('',#34189);
#10092=VERTEX_POINT('',#34190);
#10093=VERTEX_POINT('',#34193);
#10094=VERTEX_POINT('',#34194);
#10095=VERTEX_POINT('',#34197);
#10096=VERTEX_POINT('',#34198);
#10097=VERTEX_POINT('',#34202);
#10098=VERTEX_POINT('',#34203);
#10099=VERTEX_POINT('',#34226);
#10100=VERTEX_POINT('',#34228);
#10101=VERTEX_POINT('',#34253);
#10102=VERTEX_POINT('',#34255);
#10103=VERTEX_POINT('',#34278);
#10104=VERTEX_POINT('',#34280);
#10105=VERTEX_POINT('',#34303);
#10106=VERTEX_POINT('',#34305);
#10107=VERTEX_POINT('',#34318);
#10108=VERTEX_POINT('',#34321);
#10109=VERTEX_POINT('',#34334);
#10110=VERTEX_POINT('',#34336);
#10111=VERTEX_POINT('',#34359);
#10112=VERTEX_POINT('',#34361);
#10113=VERTEX_POINT('',#34384);
#10114=VERTEX_POINT('',#34386);
#10115=VERTEX_POINT('',#34409);
#10116=VERTEX_POINT('',#34411);
#10117=VERTEX_POINT('',#34436);
#10118=VERTEX_POINT('',#34440);
#10119=VERTEX_POINT('',#34465);
#10120=VERTEX_POINT('',#34469);
#10121=VERTEX_POINT('',#34494);
#10122=VERTEX_POINT('',#34498);
#10123=VERTEX_POINT('',#34499);
#10124=VERTEX_POINT('',#34526);
#10125=VERTEX_POINT('',#34530);
#10126=VERTEX_POINT('',#34555);
#10127=VERTEX_POINT('',#34559);
#10128=VERTEX_POINT('',#34584);
#10129=VERTEX_POINT('',#34588);
#10130=VERTEX_POINT('',#34613);
#10131=VERTEX_POINT('',#34616);
#10132=VERTEX_POINT('',#34618);
#10133=VERTEX_POINT('',#34650);
#10134=VERTEX_POINT('',#34652);
#10135=VERTEX_POINT('',#34655);
#10136=VERTEX_POINT('',#34659);
#10137=VERTEX_POINT('',#34664);
#10138=VERTEX_POINT('',#34666);
#10139=VERTEX_POINT('',#34669);
#10140=VERTEX_POINT('',#34673);
#10141=VERTEX_POINT('',#34685);
#10142=VERTEX_POINT('',#34687);
#10143=VERTEX_POINT('',#34691);
#10144=VERTEX_POINT('',#34693);
#10145=VERTEX_POINT('',#34697);
#10146=VERTEX_POINT('',#34699);
#10147=VERTEX_POINT('',#34703);
#10148=VERTEX_POINT('',#34705);
#10149=VERTEX_POINT('',#34709);
#10150=VERTEX_POINT('',#34710);
#10151=VERTEX_POINT('',#34712);
#10152=VERTEX_POINT('',#34714);
#10153=VERTEX_POINT('',#34718);
#10154=VERTEX_POINT('',#34720);
#10155=VERTEX_POINT('',#34724);
#10156=VERTEX_POINT('',#34726);
#10157=VERTEX_POINT('',#34736);
#10158=VERTEX_POINT('',#34738);
#10159=VERTEX_POINT('',#34742);
#10160=VERTEX_POINT('',#34744);
#10161=VERTEX_POINT('',#34748);
#10162=VERTEX_POINT('',#34750);
#10163=VERTEX_POINT('',#34754);
#10164=VERTEX_POINT('',#34756);
#10165=VERTEX_POINT('',#34760);
#10166=VERTEX_POINT('',#34762);
#10167=VERTEX_POINT('',#34766);
#10168=VERTEX_POINT('',#34768);
#10169=VERTEX_POINT('',#34772);
#10170=VERTEX_POINT('',#34774);
#10171=VERTEX_POINT('',#34778);
#10172=VERTEX_POINT('',#34780);
#10173=VERTEX_POINT('',#34784);
#10174=VERTEX_POINT('',#34786);
#10175=VERTEX_POINT('',#34790);
#10176=VERTEX_POINT('',#34792);
#10177=VERTEX_POINT('',#34796);
#10178=VERTEX_POINT('',#34798);
#10179=VERTEX_POINT('',#34802);
#10180=VERTEX_POINT('',#34804);
#10181=VERTEX_POINT('',#34808);
#10182=VERTEX_POINT('',#34809);
#10183=VERTEX_POINT('',#34811);
#10184=VERTEX_POINT('',#34813);
#10185=VERTEX_POINT('',#34817);
#10186=VERTEX_POINT('',#34819);
#10187=VERTEX_POINT('',#34823);
#10188=VERTEX_POINT('',#34825);
#10189=VERTEX_POINT('',#34835);
#10190=VERTEX_POINT('',#34837);
#10191=VERTEX_POINT('',#34842);
#10192=VERTEX_POINT('',#34844);
#10193=VERTEX_POINT('',#34849);
#10194=VERTEX_POINT('',#34851);
#10195=VERTEX_POINT('',#34856);
#10196=VERTEX_POINT('',#34858);
#10197=VERTEX_POINT('',#34863);
#10198=VERTEX_POINT('',#34865);
#10199=VERTEX_POINT('',#34870);
#10200=VERTEX_POINT('',#34872);
#10201=VERTEX_POINT('',#34877);
#10202=VERTEX_POINT('',#34879);
#10203=VERTEX_POINT('',#34884);
#10204=VERTEX_POINT('',#34886);
#10205=VERTEX_POINT('',#34890);
#10206=VERTEX_POINT('',#34891);
#10207=VERTEX_POINT('',#34893);
#10208=VERTEX_POINT('',#34895);
#10209=VERTEX_POINT('',#34899);
#10210=VERTEX_POINT('',#34901);
#10211=VERTEX_POINT('',#34905);
#10212=VERTEX_POINT('',#34907);
#10213=VERTEX_POINT('',#34918);
#10214=VERTEX_POINT('',#34919);
#10215=VERTEX_POINT('',#34923);
#10216=VERTEX_POINT('',#34925);
#10217=VERTEX_POINT('',#34927);
#10218=VERTEX_POINT('',#34930);
#10219=VERTEX_POINT('',#34934);
#10220=VERTEX_POINT('',#34935);
#10221=VERTEX_POINT('',#34939);
#10222=VERTEX_POINT('',#34941);
#10223=VERTEX_POINT('',#34943);
#10224=VERTEX_POINT('',#34946);
#10225=VERTEX_POINT('',#34950);
#10226=VERTEX_POINT('',#34951);
#10227=VERTEX_POINT('',#34955);
#10228=VERTEX_POINT('',#34957);
#10229=VERTEX_POINT('',#34959);
#10230=VERTEX_POINT('',#34962);
#10231=VERTEX_POINT('',#34966);
#10232=VERTEX_POINT('',#34967);
#10233=VERTEX_POINT('',#34971);
#10234=VERTEX_POINT('',#34973);
#10235=VERTEX_POINT('',#34975);
#10236=VERTEX_POINT('',#34978);
#10237=VERTEX_POINT('',#34983);
#10238=VERTEX_POINT('',#34985);
#10239=VERTEX_POINT('',#34987);
#10240=VERTEX_POINT('',#34989);
#10241=VERTEX_POINT('',#34994);
#10242=VERTEX_POINT('',#34996);
#10243=VERTEX_POINT('',#34998);
#10244=VERTEX_POINT('',#35000);
#10245=VERTEX_POINT('',#35004);
#10246=VERTEX_POINT('',#35006);
#10247=VERTEX_POINT('',#35008);
#10248=VERTEX_POINT('',#35010);
#10249=VERTEX_POINT('',#35013);
#10250=VERTEX_POINT('',#35015);
#10251=VERTEX_POINT('',#35017);
#10252=VERTEX_POINT('',#35019);
#10253=VERTEX_POINT('',#35023);
#10254=VERTEX_POINT('',#35027);
#10255=VERTEX_POINT('',#35031);
#10256=VERTEX_POINT('',#35035);
#10257=VERTEX_POINT('',#35041);
#10258=VERTEX_POINT('',#35045);
#10259=VERTEX_POINT('',#35049);
#10260=VERTEX_POINT('',#35053);
#10261=VERTEX_POINT('',#35061);
#10262=VERTEX_POINT('',#35062);
#10263=VERTEX_POINT('',#35064);
#10264=VERTEX_POINT('',#35066);
#10265=VERTEX_POINT('',#35070);
#10266=VERTEX_POINT('',#35072);
#10267=VERTEX_POINT('',#35076);
#10268=VERTEX_POINT('',#35078);
#10269=VERTEX_POINT('',#35082);
#10270=VERTEX_POINT('',#35084);
#10271=VERTEX_POINT('',#35088);
#10272=VERTEX_POINT('',#35090);
#10273=VERTEX_POINT('',#35094);
#10274=VERTEX_POINT('',#35096);
#10275=VERTEX_POINT('',#35100);
#10276=VERTEX_POINT('',#35102);
#10277=VERTEX_POINT('',#35112);
#10278=VERTEX_POINT('',#35113);
#10279=VERTEX_POINT('',#35115);
#10280=VERTEX_POINT('',#35117);
#10281=VERTEX_POINT('',#35121);
#10282=VERTEX_POINT('',#35123);
#10283=VERTEX_POINT('',#35127);
#10284=VERTEX_POINT('',#35129);
#10285=VERTEX_POINT('',#35133);
#10286=VERTEX_POINT('',#35135);
#10287=VERTEX_POINT('',#35139);
#10288=VERTEX_POINT('',#35141);
#10289=VERTEX_POINT('',#35145);
#10290=VERTEX_POINT('',#35147);
#10291=VERTEX_POINT('',#35151);
#10292=VERTEX_POINT('',#35153);
#10293=VERTEX_POINT('',#35166);
#10294=VERTEX_POINT('',#35168);
#10295=VERTEX_POINT('',#35172);
#10296=VERTEX_POINT('',#35176);
#10297=VERTEX_POINT('',#35179);
#10298=VERTEX_POINT('',#35185);
#10299=VERTEX_POINT('',#35186);
#10300=VERTEX_POINT('',#35188);
#10301=VERTEX_POINT('',#35190);
#10302=VERTEX_POINT('',#35194);
#10303=VERTEX_POINT('',#35196);
#10304=VERTEX_POINT('',#35200);
#10305=VERTEX_POINT('',#35202);
#10306=VERTEX_POINT('',#35206);
#10307=VERTEX_POINT('',#35208);
#10308=VERTEX_POINT('',#35212);
#10309=VERTEX_POINT('',#35214);
#10310=VERTEX_POINT('',#35223);
#10311=VERTEX_POINT('',#35225);
#10312=VERTEX_POINT('',#35228);
#10313=VERTEX_POINT('',#35233);
#10314=VERTEX_POINT('',#35236);
#10315=VERTEX_POINT('',#35240);
#10316=VERTEX_POINT('',#35244);
#10317=VERTEX_POINT('',#35248);
#10318=VERTEX_POINT('',#35251);
#10319=VERTEX_POINT('',#35258);
#10320=VERTEX_POINT('',#35259);
#10321=VERTEX_POINT('',#35261);
#10322=VERTEX_POINT('',#35287);
#10323=VERTEX_POINT('',#35330);
#10324=VERTEX_POINT('',#35331);
#10325=VERTEX_POINT('',#35417);
#10326=VERTEX_POINT('',#35418);
#10327=VERTEX_POINT('',#35507);
#10328=VERTEX_POINT('',#35508);
#10329=VERTEX_POINT('',#35594);
#10330=VERTEX_POINT('',#35595);
#10331=VERTEX_POINT('',#35684);
#10332=VERTEX_POINT('',#35685);
#10333=VERTEX_POINT('',#35771);
#10334=VERTEX_POINT('',#35772);
#10335=VERTEX_POINT('',#35858);
#10336=VERTEX_POINT('',#35859);
#10337=VERTEX_POINT('',#35948);
#10338=VERTEX_POINT('',#35949);
#10339=VERTEX_POINT('',#35951);
#10340=VERTEX_POINT('',#35964);
#10341=VERTEX_POINT('',#35965);
#10342=VERTEX_POINT('',#35967);
#10343=VERTEX_POINT('',#35975);
#10344=VERTEX_POINT('',#35990);
#10345=VERTEX_POINT('',#35991);
#10346=VERTEX_POINT('',#36027);
#10347=VERTEX_POINT('',#36028);
#10348=VERTEX_POINT('',#36064);
#10349=VERTEX_POINT('',#36065);
#10350=VERTEX_POINT('',#36102);
#10351=VERTEX_POINT('',#36103);
#10352=VERTEX_POINT('',#36139);
#10353=VERTEX_POINT('',#36140);
#10354=VERTEX_POINT('',#36176);
#10355=VERTEX_POINT('',#36177);
#10356=VERTEX_POINT('',#36214);
#10357=VERTEX_POINT('',#36215);
#10358=VERTEX_POINT('',#36252);
#10359=VERTEX_POINT('',#36253);
#10360=VERTEX_POINT('',#36255);
#10361=VERTEX_POINT('',#36261);
#10362=VERTEX_POINT('',#37325);
#10363=VERTEX_POINT('',#37417);
#10364=VERTEX_POINT('',#37418);
#10365=VERTEX_POINT('',#37422);
#10366=VERTEX_POINT('',#37424);
#10367=VERTEX_POINT('',#37426);
#10368=VERTEX_POINT('',#37429);
#10369=VERTEX_POINT('',#37433);
#10370=VERTEX_POINT('',#37437);
#10371=VERTEX_POINT('',#37441);
#10372=VERTEX_POINT('',#37442);
#10373=VERTEX_POINT('',#37448);
#10374=VERTEX_POINT('',#37453);
#10375=VERTEX_POINT('',#37459);
#10376=VERTEX_POINT('',#37462);
#10377=VERTEX_POINT('',#37466);
#10378=VERTEX_POINT('',#37470);
#10379=VERTEX_POINT('',#37474);
#10380=VERTEX_POINT('',#37477);
#10381=VERTEX_POINT('',#37481);
#10382=VERTEX_POINT('',#37485);
#10383=VERTEX_POINT('',#37490);
#10384=VERTEX_POINT('',#37491);
#10385=VERTEX_POINT('',#37493);
#10386=VERTEX_POINT('',#37495);
#10387=VERTEX_POINT('',#37499);
#10388=VERTEX_POINT('',#37501);
#10389=VERTEX_POINT('',#37505);
#10390=VERTEX_POINT('',#37507);
#10391=VERTEX_POINT('',#37511);
#10392=VERTEX_POINT('',#37513);
#10393=VERTEX_POINT('',#37517);
#10394=VERTEX_POINT('',#37519);
#10395=VERTEX_POINT('',#37529);
#10396=VERTEX_POINT('',#37532);
#10397=VERTEX_POINT('',#37536);
#10398=VERTEX_POINT('',#37540);
#10399=VERTEX_POINT('',#37544);
#10400=VERTEX_POINT('',#37547);
#10401=VERTEX_POINT('',#37551);
#10402=VERTEX_POINT('',#37555);
#10403=VERTEX_POINT('',#37560);
#10404=VERTEX_POINT('',#37561);
#10405=VERTEX_POINT('',#37563);
#10406=VERTEX_POINT('',#37565);
#10407=VERTEX_POINT('',#37569);
#10408=VERTEX_POINT('',#37571);
#10409=VERTEX_POINT('',#37575);
#10410=VERTEX_POINT('',#37577);
#10411=VERTEX_POINT('',#37581);
#10412=VERTEX_POINT('',#37583);
#10413=VERTEX_POINT('',#37587);
#10414=VERTEX_POINT('',#37589);
#10415=VERTEX_POINT('',#37620);
#10416=VERTEX_POINT('',#37621);
#10417=VERTEX_POINT('',#37623);
#10418=VERTEX_POINT('',#37643);
#10419=VERTEX_POINT('',#37650);
#10420=VERTEX_POINT('',#37651);
#10421=VERTEX_POINT('',#37737);
#10422=VERTEX_POINT('',#37738);
#10423=VERTEX_POINT('',#37827);
#10424=VERTEX_POINT('',#37828);
#10425=VERTEX_POINT('',#37914);
#10426=VERTEX_POINT('',#37915);
#10427=VERTEX_POINT('',#38001);
#10428=VERTEX_POINT('',#38002);
#10429=VERTEX_POINT('',#38088);
#10430=VERTEX_POINT('',#38089);
#10431=VERTEX_POINT('',#38175);
#10432=VERTEX_POINT('',#38176);
#10433=VERTEX_POINT('',#38262);
#10434=VERTEX_POINT('',#38263);
#10435=VERTEX_POINT('',#38334);
#10436=VERTEX_POINT('',#38335);
#10437=VERTEX_POINT('',#38385);
#10438=VERTEX_POINT('',#38386);
#10439=VERTEX_POINT('',#38433);
#10440=VERTEX_POINT('',#38434);
#10441=VERTEX_POINT('',#38481);
#10442=VERTEX_POINT('',#38482);
#10443=VERTEX_POINT('',#38532);
#10444=VERTEX_POINT('',#38533);
#10445=VERTEX_POINT('',#38583);
#10446=VERTEX_POINT('',#38584);
#10447=VERTEX_POINT('',#38631);
#10448=VERTEX_POINT('',#38632);
#10449=VERTEX_POINT('',#38682);
#10450=VERTEX_POINT('',#38683);
#10451=VERTEX_POINT('',#38733);
#10452=VERTEX_POINT('',#38734);
#10453=VERTEX_POINT('',#38781);
#10454=VERTEX_POINT('',#38782);
#10455=VERTEX_POINT('',#38829);
#10456=VERTEX_POINT('',#38830);
#10457=VERTEX_POINT('',#38880);
#10458=VERTEX_POINT('',#38881);
#10459=VERTEX_POINT('',#38931);
#10460=VERTEX_POINT('',#38932);
#10461=VERTEX_POINT('',#38979);
#10462=VERTEX_POINT('',#38980);
#10463=VERTEX_POINT('',#39030);
#10464=VERTEX_POINT('',#39031);
#10465=VERTEX_POINT('',#39081);
#10466=VERTEX_POINT('',#39082);
#10467=VERTEX_POINT('',#39129);
#10468=VERTEX_POINT('',#39130);
#10469=VERTEX_POINT('',#39177);
#10470=VERTEX_POINT('',#39178);
#10471=VERTEX_POINT('',#39228);
#10472=VERTEX_POINT('',#39229);
#10473=VERTEX_POINT('',#39279);
#10474=VERTEX_POINT('',#39280);
#10475=VERTEX_POINT('',#39327);
#10476=VERTEX_POINT('',#39328);
#10477=VERTEX_POINT('',#39378);
#10478=VERTEX_POINT('',#39379);
#10479=VERTEX_POINT('',#39429);
#10480=VERTEX_POINT('',#39430);
#10481=VERTEX_POINT('',#39477);
#10482=VERTEX_POINT('',#39478);
#10483=VERTEX_POINT('',#39525);
#10484=VERTEX_POINT('',#39526);
#10485=VERTEX_POINT('',#39576);
#10486=VERTEX_POINT('',#39577);
#10487=VERTEX_POINT('',#39627);
#10488=VERTEX_POINT('',#39628);
#10489=VERTEX_POINT('',#39675);
#10490=VERTEX_POINT('',#39676);
#10491=VERTEX_POINT('',#39726);
#10492=VERTEX_POINT('',#39727);
#10493=VERTEX_POINT('',#39777);
#10494=VERTEX_POINT('',#39778);
#10495=VERTEX_POINT('',#39825);
#10496=VERTEX_POINT('',#39826);
#10497=VERTEX_POINT('',#39873);
#10498=VERTEX_POINT('',#39874);
#10499=VERTEX_POINT('',#39924);
#10500=VERTEX_POINT('',#39925);
#10501=VERTEX_POINT('',#39975);
#10502=VERTEX_POINT('',#39976);
#10503=VERTEX_POINT('',#40023);
#10504=VERTEX_POINT('',#40024);
#10505=VERTEX_POINT('',#40074);
#10506=VERTEX_POINT('',#40075);
#10507=VERTEX_POINT('',#40125);
#10508=VERTEX_POINT('',#40126);
#10509=VERTEX_POINT('',#40173);
#10510=VERTEX_POINT('',#40174);
#10511=VERTEX_POINT('',#40221);
#10512=VERTEX_POINT('',#40222);
#10513=VERTEX_POINT('',#40272);
#10514=VERTEX_POINT('',#40273);
#10515=VERTEX_POINT('',#40323);
#10516=VERTEX_POINT('',#40324);
#10517=VERTEX_POINT('',#40371);
#10518=VERTEX_POINT('',#40372);
#10519=VERTEX_POINT('',#40422);
#10520=VERTEX_POINT('',#40423);
#10521=VERTEX_POINT('',#40473);
#10522=VERTEX_POINT('',#40474);
#10523=VERTEX_POINT('',#40521);
#10524=VERTEX_POINT('',#40522);
#10525=VERTEX_POINT('',#40569);
#10526=VERTEX_POINT('',#40570);
#10527=VERTEX_POINT('',#40620);
#10528=VERTEX_POINT('',#40621);
#10529=VERTEX_POINT('',#40686);
#10530=VERTEX_POINT('',#40687);
#10531=VERTEX_POINT('',#40776);
#10532=VERTEX_POINT('',#40777);
#10533=VERTEX_POINT('',#40863);
#10534=VERTEX_POINT('',#40864);
#10535=VERTEX_POINT('',#40950);
#10536=VERTEX_POINT('',#40951);
#10537=VERTEX_POINT('',#41037);
#10538=VERTEX_POINT('',#41038);
#10539=VERTEX_POINT('',#41124);
#10540=VERTEX_POINT('',#41125);
#10541=VERTEX_POINT('',#41211);
#10542=VERTEX_POINT('',#41212);
#10543=VERTEX_POINT('',#41301);
#10544=VERTEX_POINT('',#41302);
#10545=VERTEX_POINT('',#41304);
#10546=VERTEX_POINT('',#41311);
#10547=VERTEX_POINT('',#41312);
#10548=VERTEX_POINT('',#41331);
#10549=VERTEX_POINT('',#41347);
#10550=VERTEX_POINT('',#41348);
#10551=VERTEX_POINT('',#41385);
#10552=VERTEX_POINT('',#41386);
#10553=VERTEX_POINT('',#41421);
#10554=VERTEX_POINT('',#41422);
#10555=VERTEX_POINT('',#41459);
#10556=VERTEX_POINT('',#41460);
#10557=VERTEX_POINT('',#41495);
#10558=VERTEX_POINT('',#41496);
#10559=VERTEX_POINT('',#41533);
#10560=VERTEX_POINT('',#41534);
#10561=VERTEX_POINT('',#41570);
#10562=VERTEX_POINT('',#41571);
#10563=VERTEX_POINT('',#41605);
#10564=VERTEX_POINT('',#41606);
#10565=VERTEX_POINT('',#41632);
#10566=VERTEX_POINT('',#41633);
#10567=VERTEX_POINT('',#41656);
#10568=VERTEX_POINT('',#41657);
#10569=VERTEX_POINT('',#41680);
#10570=VERTEX_POINT('',#41681);
#10571=VERTEX_POINT('',#41704);
#10572=VERTEX_POINT('',#41705);
#10573=VERTEX_POINT('',#41730);
#10574=VERTEX_POINT('',#41731);
#10575=VERTEX_POINT('',#41754);
#10576=VERTEX_POINT('',#41755);
#10577=VERTEX_POINT('',#41778);
#10578=VERTEX_POINT('',#41779);
#10579=VERTEX_POINT('',#41804);
#10580=VERTEX_POINT('',#41805);
#10581=VERTEX_POINT('',#41828);
#10582=VERTEX_POINT('',#41829);
#10583=VERTEX_POINT('',#41852);
#10584=VERTEX_POINT('',#41853);
#10585=VERTEX_POINT('',#41876);
#10586=VERTEX_POINT('',#41877);
#10587=VERTEX_POINT('',#41902);
#10588=VERTEX_POINT('',#41903);
#10589=VERTEX_POINT('',#41926);
#10590=VERTEX_POINT('',#41927);
#10591=VERTEX_POINT('',#41950);
#10592=VERTEX_POINT('',#41951);
#10593=VERTEX_POINT('',#41976);
#10594=VERTEX_POINT('',#41977);
#10595=VERTEX_POINT('',#42000);
#10596=VERTEX_POINT('',#42001);
#10597=VERTEX_POINT('',#42024);
#10598=VERTEX_POINT('',#42025);
#10599=VERTEX_POINT('',#42048);
#10600=VERTEX_POINT('',#42049);
#10601=VERTEX_POINT('',#42074);
#10602=VERTEX_POINT('',#42075);
#10603=VERTEX_POINT('',#42098);
#10604=VERTEX_POINT('',#42099);
#10605=VERTEX_POINT('',#42122);
#10606=VERTEX_POINT('',#42123);
#10607=VERTEX_POINT('',#42148);
#10608=VERTEX_POINT('',#42149);
#10609=VERTEX_POINT('',#42172);
#10610=VERTEX_POINT('',#42173);
#10611=VERTEX_POINT('',#42196);
#10612=VERTEX_POINT('',#42197);
#10613=VERTEX_POINT('',#42220);
#10614=VERTEX_POINT('',#42221);
#10615=VERTEX_POINT('',#42246);
#10616=VERTEX_POINT('',#42247);
#10617=VERTEX_POINT('',#42270);
#10618=VERTEX_POINT('',#42271);
#10619=VERTEX_POINT('',#42294);
#10620=VERTEX_POINT('',#42295);
#10621=VERTEX_POINT('',#42320);
#10622=VERTEX_POINT('',#42321);
#10623=VERTEX_POINT('',#42344);
#10624=VERTEX_POINT('',#42345);
#10625=VERTEX_POINT('',#42368);
#10626=VERTEX_POINT('',#42369);
#10627=VERTEX_POINT('',#42392);
#10628=VERTEX_POINT('',#42393);
#10629=VERTEX_POINT('',#42418);
#10630=VERTEX_POINT('',#42419);
#10631=VERTEX_POINT('',#42442);
#10632=VERTEX_POINT('',#42443);
#10633=VERTEX_POINT('',#42466);
#10634=VERTEX_POINT('',#42467);
#10635=VERTEX_POINT('',#42492);
#10636=VERTEX_POINT('',#42493);
#10637=VERTEX_POINT('',#42516);
#10638=VERTEX_POINT('',#42517);
#10639=VERTEX_POINT('',#42540);
#10640=VERTEX_POINT('',#42541);
#10641=VERTEX_POINT('',#42564);
#10642=VERTEX_POINT('',#42565);
#10643=VERTEX_POINT('',#42590);
#10644=VERTEX_POINT('',#42591);
#10645=VERTEX_POINT('',#42614);
#10646=VERTEX_POINT('',#42615);
#10647=VERTEX_POINT('',#42638);
#10648=VERTEX_POINT('',#42639);
#10649=VERTEX_POINT('',#42664);
#10650=VERTEX_POINT('',#42665);
#10651=VERTEX_POINT('',#42688);
#10652=VERTEX_POINT('',#42689);
#10653=VERTEX_POINT('',#42712);
#10654=VERTEX_POINT('',#42713);
#10655=VERTEX_POINT('',#42737);
#10656=VERTEX_POINT('',#42738);
#10657=VERTEX_POINT('',#42764);
#10658=VERTEX_POINT('',#42765);
#10659=VERTEX_POINT('',#42801);
#10660=VERTEX_POINT('',#42802);
#10661=VERTEX_POINT('',#42837);
#10662=VERTEX_POINT('',#42838);
#10663=VERTEX_POINT('',#42875);
#10664=VERTEX_POINT('',#42876);
#10665=VERTEX_POINT('',#42911);
#10666=VERTEX_POINT('',#42912);
#10667=VERTEX_POINT('',#42949);
#10668=VERTEX_POINT('',#42950);
#10669=VERTEX_POINT('',#42986);
#10670=VERTEX_POINT('',#42987);
#10671=VERTEX_POINT('',#43023);
#10672=VERTEX_POINT('',#43025);
#10673=VERTEX_POINT('',#43063);
#10674=VERTEX_POINT('',#43103);
#10675=VERTEX_POINT('',#45099);
#10676=VERTEX_POINT('',#47184);
#10677=VERTEX_POINT('',#47236);
#10678=VERTEX_POINT('',#47237);
#10679=VERTEX_POINT('',#47239);
#10680=VERTEX_POINT('',#47241);
#10681=VERTEX_POINT('',#47245);
#10682=VERTEX_POINT('',#47247);
#10683=VERTEX_POINT('',#47251);
#10684=VERTEX_POINT('',#47255);
#10685=VERTEX_POINT('',#47261);
#10686=VERTEX_POINT('',#47263);
#10687=VERTEX_POINT('',#47268);
#10688=VERTEX_POINT('',#47272);
#10689=VERTEX_POINT('',#47279);
#10690=VERTEX_POINT('',#47281);
#10691=VERTEX_POINT('',#47285);
#10692=VERTEX_POINT('',#47287);
#10693=VERTEX_POINT('',#47294);
#10694=VERTEX_POINT('',#47295);
#10695=VERTEX_POINT('',#47299);
#10696=VERTEX_POINT('',#47300);
#10697=VERTEX_POINT('',#47309);
#10698=VERTEX_POINT('',#47333);
#10699=VERTEX_POINT('',#47335);
#10700=VERTEX_POINT('',#47375);
#10701=VERTEX_POINT('',#47377);
#10702=VERTEX_POINT('',#47381);
#10703=VERTEX_POINT('',#47383);
#10704=VERTEX_POINT('',#47390);
#10705=VERTEX_POINT('',#47392);
#10706=VERTEX_POINT('',#47396);
#10707=VERTEX_POINT('',#47397);
#10708=VERTEX_POINT('',#47401);
#10709=VERTEX_POINT('',#47402);
#10710=VERTEX_POINT('',#47409);
#10711=VERTEX_POINT('',#47427);
#10712=VERTEX_POINT('',#47429);
#10713=VERTEX_POINT('',#47469);
#10714=VERTEX_POINT('',#47470);
#10715=VERTEX_POINT('',#47472);
#10716=VERTEX_POINT('',#47474);
#10717=VERTEX_POINT('',#47476);
#10718=VERTEX_POINT('',#47478);
#10719=VERTEX_POINT('',#47482);
#10720=VERTEX_POINT('',#47484);
#10721=VERTEX_POINT('',#47488);
#10722=VERTEX_POINT('',#47490);
#10723=VERTEX_POINT('',#47492);
#10724=VERTEX_POINT('',#47494);
#10725=VERTEX_POINT('',#47498);
#10726=VERTEX_POINT('',#47502);
#10727=VERTEX_POINT('',#47514);
#10728=VERTEX_POINT('',#47516);
#10729=VERTEX_POINT('',#47520);
#10730=VERTEX_POINT('',#47522);
#10731=VERTEX_POINT('',#47529);
#10732=VERTEX_POINT('',#47531);
#10733=VERTEX_POINT('',#47535);
#10734=VERTEX_POINT('',#47537);
#10735=VERTEX_POINT('',#47544);
#10736=VERTEX_POINT('',#47545);
#10737=VERTEX_POINT('',#47547);
#10738=VERTEX_POINT('',#47549);
#10739=VERTEX_POINT('',#47551);
#10740=VERTEX_POINT('',#47553);
#10741=VERTEX_POINT('',#47555);
#10742=VERTEX_POINT('',#47557);
#10743=VERTEX_POINT('',#47561);
#10744=VERTEX_POINT('',#47563);
#10745=VERTEX_POINT('',#47567);
#10746=VERTEX_POINT('',#47571);
#10747=VERTEX_POINT('',#47575);
#10748=VERTEX_POINT('',#47579);
#10749=VERTEX_POINT('',#47580);
#10750=VERTEX_POINT('',#47583);
#10751=VERTEX_POINT('',#47595);
#10752=VERTEX_POINT('',#47596);
#10753=VERTEX_POINT('',#47598);
#10754=VERTEX_POINT('',#47600);
#10755=VERTEX_POINT('',#47604);
#10756=VERTEX_POINT('',#47606);
#10757=VERTEX_POINT('',#47610);
#10758=VERTEX_POINT('',#47612);
#10759=VERTEX_POINT('',#47616);
#10760=VERTEX_POINT('',#47618);
#10761=VERTEX_POINT('',#47622);
#10762=VERTEX_POINT('',#47624);
#10763=VERTEX_POINT('',#47632);
#10764=VERTEX_POINT('',#47635);
#10765=VERTEX_POINT('',#47639);
#10766=VERTEX_POINT('',#47643);
#10767=VERTEX_POINT('',#47649);
#10768=VERTEX_POINT('',#47651);
#10769=VERTEX_POINT('',#47655);
#10770=VERTEX_POINT('',#47657);
#10771=VERTEX_POINT('',#47664);
#10772=VERTEX_POINT('',#47667);
#10773=VERTEX_POINT('',#47671);
#10774=VERTEX_POINT('',#47675);
#10775=VERTEX_POINT('',#47679);
#10776=VERTEX_POINT('',#47682);
#10777=VERTEX_POINT('',#47686);
#10778=VERTEX_POINT('',#47690);
#10779=VERTEX_POINT('',#47695);
#10780=VERTEX_POINT('',#47696);
#10781=VERTEX_POINT('',#47698);
#10782=VERTEX_POINT('',#47700);
#10783=VERTEX_POINT('',#47704);
#10784=VERTEX_POINT('',#47706);
#10785=VERTEX_POINT('',#47710);
#10786=VERTEX_POINT('',#47712);
#10787=VERTEX_POINT('',#47716);
#10788=VERTEX_POINT('',#47718);
#10789=VERTEX_POINT('',#47722);
#10790=VERTEX_POINT('',#47724);
#10791=VERTEX_POINT('',#47783);
#10792=VERTEX_POINT('',#47785);
#10793=VERTEX_POINT('',#47790);
#10794=VERTEX_POINT('',#47792);
#10795=VERTEX_POINT('',#47797);
#10796=VERTEX_POINT('',#47799);
#10797=VERTEX_POINT('',#47804);
#10798=VERTEX_POINT('',#47806);
#10799=VERTEX_POINT('',#47811);
#10800=VERTEX_POINT('',#47813);
#10801=VERTEX_POINT('',#47818);
#10802=VERTEX_POINT('',#47820);
#10803=VERTEX_POINT('',#47825);
#10804=VERTEX_POINT('',#47827);
#10805=VERTEX_POINT('',#47832);
#10806=VERTEX_POINT('',#47834);
#10807=VERTEX_POINT('',#47839);
#10808=VERTEX_POINT('',#47841);
#10809=VERTEX_POINT('',#47845);
#10810=VERTEX_POINT('',#47848);
#10811=VERTEX_POINT('',#47850);
#10812=VERTEX_POINT('',#47854);
#10813=VERTEX_POINT('',#47857);
#10814=VERTEX_POINT('',#47859);
#10815=VERTEX_POINT('',#47863);
#10816=VERTEX_POINT('',#47866);
#10817=VERTEX_POINT('',#47868);
#10818=VERTEX_POINT('',#47872);
#10819=VERTEX_POINT('',#47875);
#10820=VERTEX_POINT('',#47879);
#10821=VERTEX_POINT('',#47883);
#10822=VERTEX_POINT('',#47887);
#10823=VERTEX_POINT('',#47891);
#10824=VERTEX_POINT('',#47893);
#10825=VERTEX_POINT('',#47897);
#10826=VERTEX_POINT('',#47899);
#10827=VERTEX_POINT('',#47903);
#10828=VERTEX_POINT('',#47905);
#10829=VERTEX_POINT('',#47909);
#10830=VERTEX_POINT('',#47911);
#10831=VERTEX_POINT('',#47915);
#10832=VERTEX_POINT('',#47917);
#10833=VERTEX_POINT('',#47921);
#10834=VERTEX_POINT('',#47923);
#10835=VERTEX_POINT('',#47927);
#10836=VERTEX_POINT('',#47929);
#10837=VERTEX_POINT('',#47933);
#10838=VERTEX_POINT('',#47935);
#10839=VERTEX_POINT('',#47939);
#10840=VERTEX_POINT('',#47941);
#10841=VERTEX_POINT('',#47945);
#10842=VERTEX_POINT('',#47947);
#10843=VERTEX_POINT('',#47951);
#10844=VERTEX_POINT('',#47952);
#10845=VERTEX_POINT('',#47954);
#10846=VERTEX_POINT('',#47956);
#10847=VERTEX_POINT('',#47960);
#10848=VERTEX_POINT('',#47962);
#10849=VERTEX_POINT('',#47966);
#10850=VERTEX_POINT('',#47968);
#10851=VERTEX_POINT('',#47978);
#10852=VERTEX_POINT('',#47979);
#10853=VERTEX_POINT('',#47981);
#10854=VERTEX_POINT('',#47983);
#10855=VERTEX_POINT('',#47987);
#10856=VERTEX_POINT('',#47988);
#10857=VERTEX_POINT('',#47990);
#10858=VERTEX_POINT('',#47992);
#10859=VERTEX_POINT('',#47996);
#10860=VERTEX_POINT('',#47998);
#10861=VERTEX_POINT('',#48002);
#10862=VERTEX_POINT('',#48004);
#10863=VERTEX_POINT('',#48008);
#10864=VERTEX_POINT('',#48010);
#10865=VERTEX_POINT('',#48014);
#10866=VERTEX_POINT('',#48016);
#10867=VERTEX_POINT('',#48020);
#10868=VERTEX_POINT('',#48022);
#10869=VERTEX_POINT('',#48026);
#10870=VERTEX_POINT('',#48033);
#10871=VERTEX_POINT('',#48036);
#10872=VERTEX_POINT('',#48038);
#10873=VERTEX_POINT('',#48042);
#10874=VERTEX_POINT('',#48049);
#10875=VERTEX_POINT('',#48052);
#10876=VERTEX_POINT('',#48053);
#10877=VERTEX_POINT('',#48055);
#10878=VERTEX_POINT('',#48057);
#10879=VERTEX_POINT('',#48063);
#10880=VERTEX_POINT('',#48067);
#10881=VERTEX_POINT('',#48071);
#10882=VERTEX_POINT('',#48075);
#10883=VERTEX_POINT('',#48079);
#10884=VERTEX_POINT('',#48080);
#10885=VERTEX_POINT('',#48085);
#10886=VERTEX_POINT('',#48089);
#10887=VERTEX_POINT('',#48097);
#10888=VERTEX_POINT('',#48099);
#10889=VERTEX_POINT('',#48103);
#10890=VERTEX_POINT('',#48105);
#10891=VERTEX_POINT('',#48109);
#10892=VERTEX_POINT('',#48111);
#10893=VERTEX_POINT('',#48115);
#10894=VERTEX_POINT('',#48117);
#10895=VERTEX_POINT('',#48121);
#10896=VERTEX_POINT('',#48124);
#10897=VERTEX_POINT('',#48128);
#10898=VERTEX_POINT('',#48130);
#10899=VERTEX_POINT('',#48135);
#10900=VERTEX_POINT('',#48137);
#10901=VERTEX_POINT('',#48142);
#10902=VERTEX_POINT('',#48143);
#10903=VERTEX_POINT('',#48145);
#10904=VERTEX_POINT('',#48147);
#10905=VERTEX_POINT('',#48151);
#10906=VERTEX_POINT('',#48153);
#10907=VERTEX_POINT('',#48157);
#10908=VERTEX_POINT('',#48159);
#10909=VERTEX_POINT('',#48169);
#10910=VERTEX_POINT('',#48171);
#10911=VERTEX_POINT('',#48175);
#10912=VERTEX_POINT('',#48177);
#10913=VERTEX_POINT('',#48181);
#10914=VERTEX_POINT('',#48183);
#10915=VERTEX_POINT('',#48187);
#10916=VERTEX_POINT('',#48189);
#10917=VERTEX_POINT('',#48193);
#10918=VERTEX_POINT('',#48196);
#10919=VERTEX_POINT('',#48200);
#10920=VERTEX_POINT('',#48202);
#10921=VERTEX_POINT('',#48209);
#10922=VERTEX_POINT('',#48211);
#10923=VERTEX_POINT('',#48215);
#10924=VERTEX_POINT('',#48217);
#10925=VERTEX_POINT('',#48221);
#10926=VERTEX_POINT('',#48223);
#10927=VERTEX_POINT('',#48227);
#10928=VERTEX_POINT('',#48229);
#10929=VERTEX_POINT('',#48233);
#10930=VERTEX_POINT('',#48236);
#10931=VERTEX_POINT('',#48240);
#10932=VERTEX_POINT('',#48242);
#10933=VERTEX_POINT('',#48247);
#10934=VERTEX_POINT('',#48249);
#10935=VERTEX_POINT('',#48254);
#10936=VERTEX_POINT('',#48255);
#10937=VERTEX_POINT('',#48257);
#10938=VERTEX_POINT('',#48259);
#10939=VERTEX_POINT('',#48263);
#10940=VERTEX_POINT('',#48265);
#10941=VERTEX_POINT('',#48269);
#10942=VERTEX_POINT('',#48271);
#10943=VERTEX_POINT('',#48281);
#10944=VERTEX_POINT('',#48283);
#10945=VERTEX_POINT('',#48287);
#10946=VERTEX_POINT('',#48289);
#10947=VERTEX_POINT('',#48293);
#10948=VERTEX_POINT('',#48295);
#10949=VERTEX_POINT('',#48299);
#10950=VERTEX_POINT('',#48300);
#10951=VERTEX_POINT('',#48302);
#10952=VERTEX_POINT('',#48304);
#10953=VERTEX_POINT('',#48309);
#10954=VERTEX_POINT('',#48314);
#10955=VERTEX_POINT('',#48318);
#10956=VERTEX_POINT('',#48321);
#10957=VERTEX_POINT('',#48327);
#10958=VERTEX_POINT('',#48329);
#10959=VERTEX_POINT('',#48333);
#10960=VERTEX_POINT('',#48336);
#10961=VERTEX_POINT('',#48340);
#10962=VERTEX_POINT('',#48341);
#10963=VERTEX_POINT('',#48343);
#10964=VERTEX_POINT('',#48345);
#10965=VERTEX_POINT('',#48349);
#10966=VERTEX_POINT('',#48351);
#10967=VERTEX_POINT('',#48355);
#10968=VERTEX_POINT('',#48357);
#10969=VERTEX_POINT('',#48367);
#10970=VERTEX_POINT('',#48369);
#10971=VERTEX_POINT('',#48373);
#10972=VERTEX_POINT('',#48376);
#10973=VERTEX_POINT('',#48380);
#10974=VERTEX_POINT('',#48381);
#10975=VERTEX_POINT('',#48383);
#10976=VERTEX_POINT('',#48385);
#10977=VERTEX_POINT('',#48389);
#10978=VERTEX_POINT('',#48391);
#10979=VERTEX_POINT('',#48395);
#10980=VERTEX_POINT('',#48397);
#10981=VERTEX_POINT('',#48407);
#10982=VERTEX_POINT('',#48409);
#10983=VERTEX_POINT('',#48413);
#10984=VERTEX_POINT('',#48416);
#10985=VERTEX_POINT('',#48418);
#10986=VERTEX_POINT('',#48422);
#10987=VERTEX_POINT('',#48425);
#10988=VERTEX_POINT('',#48427);
#10989=VERTEX_POINT('',#48431);
#10990=VERTEX_POINT('',#48434);
#10991=VERTEX_POINT('',#48436);
#10992=VERTEX_POINT('',#48440);
#10993=VERTEX_POINT('',#48443);
#10994=VERTEX_POINT('',#48447);
#10995=VERTEX_POINT('',#48451);
#10996=VERTEX_POINT('',#48455);
#10997=VERTEX_POINT('',#48459);
#10998=VERTEX_POINT('',#48460);
#10999=VERTEX_POINT('',#48462);
#11000=VERTEX_POINT('',#48464);
#11001=VERTEX_POINT('',#48468);
#11002=VERTEX_POINT('',#48470);
#11003=VERTEX_POINT('',#48474);
#11004=VERTEX_POINT('',#48476);
#11005=VERTEX_POINT('',#48480);
#11006=VERTEX_POINT('',#48482);
#11007=VERTEX_POINT('',#48486);
#11008=VERTEX_POINT('',#48488);
#11009=VERTEX_POINT('',#48492);
#11010=VERTEX_POINT('',#48494);
#11011=VERTEX_POINT('',#48498);
#11012=VERTEX_POINT('',#48500);
#11013=VERTEX_POINT('',#48504);
#11014=VERTEX_POINT('',#48506);
#11015=VERTEX_POINT('',#48510);
#11016=VERTEX_POINT('',#48512);
#11017=VERTEX_POINT('',#48516);
#11018=VERTEX_POINT('',#48518);
#11019=VERTEX_POINT('',#48522);
#11020=VERTEX_POINT('',#48524);
#11021=VERTEX_POINT('',#48535);
#11022=VERTEX_POINT('',#48536);
#11023=VERTEX_POINT('',#48539);
#11024=VERTEX_POINT('',#48541);
#11025=VERTEX_POINT('',#48545);
#11026=VERTEX_POINT('',#48549);
#11027=VERTEX_POINT('',#48551);
#11028=VERTEX_POINT('',#48555);
#11029=VERTEX_POINT('',#48560);
#11030=VERTEX_POINT('',#48564);
#11031=VERTEX_POINT('',#48570);
#11032=VERTEX_POINT('',#48571);
#11033=VERTEX_POINT('',#48574);
#11034=VERTEX_POINT('',#48576);
#11035=VERTEX_POINT('',#48580);
#11036=VERTEX_POINT('',#48584);
#11037=VERTEX_POINT('',#48586);
#11038=VERTEX_POINT('',#48589);
#11039=VERTEX_POINT('',#48593);
#11040=VERTEX_POINT('',#48597);
#11041=VERTEX_POINT('',#48605);
#11042=VERTEX_POINT('',#48606);
#11043=VERTEX_POINT('',#48609);
#11044=VERTEX_POINT('',#48610);
#11045=VERTEX_POINT('',#48613);
#11046=VERTEX_POINT('',#48614);
#11047=VERTEX_POINT('',#48617);
#11048=VERTEX_POINT('',#48618);
#11049=VERTEX_POINT('',#48621);
#11050=VERTEX_POINT('',#48622);
#11051=VERTEX_POINT('',#48625);
#11052=VERTEX_POINT('',#48626);
#11053=VERTEX_POINT('',#48629);
#11054=VERTEX_POINT('',#48630);
#11055=VERTEX_POINT('',#48634);
#11056=VERTEX_POINT('',#48635);
#11057=VERTEX_POINT('',#48658);
#11058=VERTEX_POINT('',#48660);
#11059=VERTEX_POINT('',#48685);
#11060=VERTEX_POINT('',#48687);
#11061=VERTEX_POINT('',#48710);
#11062=VERTEX_POINT('',#48712);
#11063=VERTEX_POINT('',#48735);
#11064=VERTEX_POINT('',#48737);
#11065=VERTEX_POINT('',#48740);
#11066=VERTEX_POINT('',#48742);
#11067=VERTEX_POINT('',#48765);
#11068=VERTEX_POINT('',#48767);
#11069=VERTEX_POINT('',#48790);
#11070=VERTEX_POINT('',#48792);
#11071=VERTEX_POINT('',#48815);
#11072=VERTEX_POINT('',#48817);
#11073=VERTEX_POINT('',#48842);
#11074=VERTEX_POINT('',#48846);
#11075=VERTEX_POINT('',#48871);
#11076=VERTEX_POINT('',#48875);
#11077=VERTEX_POINT('',#48900);
#11078=VERTEX_POINT('',#48902);
#11079=VERTEX_POINT('',#48906);
#11080=VERTEX_POINT('',#48931);
#11081=VERTEX_POINT('',#48935);
#11082=VERTEX_POINT('',#48960);
#11083=VERTEX_POINT('',#48964);
#11084=VERTEX_POINT('',#48989);
#11085=VERTEX_POINT('',#48992);
#11086=VERTEX_POINT('',#48994);
#11087=VERTEX_POINT('',#49026);
#11088=VERTEX_POINT('',#49028);
#11089=VERTEX_POINT('',#49031);
#11090=VERTEX_POINT('',#49035);
#11091=VERTEX_POINT('',#49040);
#11092=VERTEX_POINT('',#49042);
#11093=VERTEX_POINT('',#49045);
#11094=VERTEX_POINT('',#49049);
#11095=VERTEX_POINT('',#49061);
#11096=VERTEX_POINT('',#49062);
#11097=VERTEX_POINT('',#49065);
#11098=VERTEX_POINT('',#49067);
#11099=VERTEX_POINT('',#49071);
#11100=VERTEX_POINT('',#49075);
#11101=VERTEX_POINT('',#49077);
#11102=VERTEX_POINT('',#49081);
#11103=VERTEX_POINT('',#49086);
#11104=VERTEX_POINT('',#49090);
#11105=VERTEX_POINT('',#49096);
#11106=VERTEX_POINT('',#49097);
#11107=VERTEX_POINT('',#49100);
#11108=VERTEX_POINT('',#49102);
#11109=VERTEX_POINT('',#49106);
#11110=VERTEX_POINT('',#49110);
#11111=VERTEX_POINT('',#49112);
#11112=VERTEX_POINT('',#49115);
#11113=VERTEX_POINT('',#49119);
#11114=VERTEX_POINT('',#49123);
#11115=VERTEX_POINT('',#49131);
#11116=VERTEX_POINT('',#49132);
#11117=VERTEX_POINT('',#49135);
#11118=VERTEX_POINT('',#49136);
#11119=VERTEX_POINT('',#49139);
#11120=VERTEX_POINT('',#49140);
#11121=VERTEX_POINT('',#49143);
#11122=VERTEX_POINT('',#49144);
#11123=VERTEX_POINT('',#49147);
#11124=VERTEX_POINT('',#49148);
#11125=VERTEX_POINT('',#49151);
#11126=VERTEX_POINT('',#49152);
#11127=VERTEX_POINT('',#49155);
#11128=VERTEX_POINT('',#49156);
#11129=VERTEX_POINT('',#49159);
#11130=VERTEX_POINT('',#49160);
#11131=VERTEX_POINT('',#49164);
#11132=VERTEX_POINT('',#49165);
#11133=VERTEX_POINT('',#49188);
#11134=VERTEX_POINT('',#49190);
#11135=VERTEX_POINT('',#49215);
#11136=VERTEX_POINT('',#49217);
#11137=VERTEX_POINT('',#49240);
#11138=VERTEX_POINT('',#49242);
#11139=VERTEX_POINT('',#49265);
#11140=VERTEX_POINT('',#49267);
#11141=VERTEX_POINT('',#49280);
#11142=VERTEX_POINT('',#49283);
#11143=VERTEX_POINT('',#49296);
#11144=VERTEX_POINT('',#49298);
#11145=VERTEX_POINT('',#49321);
#11146=VERTEX_POINT('',#49323);
#11147=VERTEX_POINT('',#49346);
#11148=VERTEX_POINT('',#49348);
#11149=VERTEX_POINT('',#49371);
#11150=VERTEX_POINT('',#49373);
#11151=VERTEX_POINT('',#49398);
#11152=VERTEX_POINT('',#49402);
#11153=VERTEX_POINT('',#49427);
#11154=VERTEX_POINT('',#49431);
#11155=VERTEX_POINT('',#49456);
#11156=VERTEX_POINT('',#49460);
#11157=VERTEX_POINT('',#49461);
#11158=VERTEX_POINT('',#49488);
#11159=VERTEX_POINT('',#49492);
#11160=VERTEX_POINT('',#49517);
#11161=VERTEX_POINT('',#49521);
#11162=VERTEX_POINT('',#49546);
#11163=VERTEX_POINT('',#49550);
#11164=VERTEX_POINT('',#49575);
#11165=VERTEX_POINT('',#49578);
#11166=VERTEX_POINT('',#49580);
#11167=VERTEX_POINT('',#49612);
#11168=VERTEX_POINT('',#49614);
#11169=VERTEX_POINT('',#49617);
#11170=VERTEX_POINT('',#49621);
#11171=VERTEX_POINT('',#49626);
#11172=VERTEX_POINT('',#49628);
#11173=VERTEX_POINT('',#49631);
#11174=VERTEX_POINT('',#49635);
#11175=VERTEX_POINT('',#49646);
#11176=VERTEX_POINT('',#49647);
#11177=VERTEX_POINT('',#49649);
#11178=VERTEX_POINT('',#49651);
#11179=VERTEX_POINT('',#49655);
#11180=VERTEX_POINT('',#49657);
#11181=VERTEX_POINT('',#49661);
#11182=VERTEX_POINT('',#49663);
#11183=VERTEX_POINT('',#49667);
#11184=VERTEX_POINT('',#49669);
#11185=VERTEX_POINT('',#49673);
#11186=VERTEX_POINT('',#49675);
#11187=VERTEX_POINT('',#49684);
#11188=VERTEX_POINT('',#49687);
#11189=VERTEX_POINT('',#49690);
#11190=VERTEX_POINT('',#49694);
#11191=VERTEX_POINT('',#49698);
#11192=VERTEX_POINT('',#49702);
#11193=VERTEX_POINT('',#49705);
#11194=VERTEX_POINT('',#49713);
#11195=VERTEX_POINT('',#49715);
#11196=VERTEX_POINT('',#49719);
#11197=VERTEX_POINT('',#49721);
#11198=VERTEX_POINT('',#49725);
#11199=VERTEX_POINT('',#49727);
#11200=VERTEX_POINT('',#49731);
#11201=VERTEX_POINT('',#49733);
#11202=VERTEX_POINT('',#49737);
#11203=VERTEX_POINT('',#49738);
#11204=VERTEX_POINT('',#49740);
#11205=VERTEX_POINT('',#49742);
#11206=VERTEX_POINT('',#49746);
#11207=VERTEX_POINT('',#49748);
#11208=VERTEX_POINT('',#49752);
#11209=VERTEX_POINT('',#49754);
#11210=VERTEX_POINT('',#49764);
#11211=VERTEX_POINT('',#49766);
#11212=VERTEX_POINT('',#49770);
#11213=VERTEX_POINT('',#49772);
#11214=VERTEX_POINT('',#49776);
#11215=VERTEX_POINT('',#49778);
#11216=VERTEX_POINT('',#49782);
#11217=VERTEX_POINT('',#49784);
#11218=VERTEX_POINT('',#49788);
#11219=VERTEX_POINT('',#49790);
#11220=VERTEX_POINT('',#49794);
#11221=VERTEX_POINT('',#49796);
#11222=VERTEX_POINT('',#49800);
#11223=VERTEX_POINT('',#49802);
#11224=VERTEX_POINT('',#49806);
#11225=VERTEX_POINT('',#49808);
#11226=VERTEX_POINT('',#49812);
#11227=VERTEX_POINT('',#49813);
#11228=VERTEX_POINT('',#49815);
#11229=VERTEX_POINT('',#49817);
#11230=VERTEX_POINT('',#49821);
#11231=VERTEX_POINT('',#49823);
#11232=VERTEX_POINT('',#49827);
#11233=VERTEX_POINT('',#49829);
#11234=VERTEX_POINT('',#49839);
#11235=VERTEX_POINT('',#49841);
#11236=VERTEX_POINT('',#49846);
#11237=VERTEX_POINT('',#49848);
#11238=VERTEX_POINT('',#49853);
#11239=VERTEX_POINT('',#49855);
#11240=VERTEX_POINT('',#49860);
#11241=VERTEX_POINT('',#49862);
#11242=VERTEX_POINT('',#49867);
#11243=VERTEX_POINT('',#49869);
#11244=VERTEX_POINT('',#49874);
#11245=VERTEX_POINT('',#49876);
#11246=VERTEX_POINT('',#49881);
#11247=VERTEX_POINT('',#49883);
#11248=VERTEX_POINT('',#49888);
#11249=VERTEX_POINT('',#49890);
#11250=VERTEX_POINT('',#49894);
#11251=VERTEX_POINT('',#49895);
#11252=VERTEX_POINT('',#49897);
#11253=VERTEX_POINT('',#49899);
#11254=VERTEX_POINT('',#49903);
#11255=VERTEX_POINT('',#49905);
#11256=VERTEX_POINT('',#49909);
#11257=VERTEX_POINT('',#49911);
#11258=VERTEX_POINT('',#49922);
#11259=VERTEX_POINT('',#49923);
#11260=VERTEX_POINT('',#49927);
#11261=VERTEX_POINT('',#49929);
#11262=VERTEX_POINT('',#49931);
#11263=VERTEX_POINT('',#49934);
#11264=VERTEX_POINT('',#49938);
#11265=VERTEX_POINT('',#49939);
#11266=VERTEX_POINT('',#49943);
#11267=VERTEX_POINT('',#49945);
#11268=VERTEX_POINT('',#49947);
#11269=VERTEX_POINT('',#49950);
#11270=VERTEX_POINT('',#49954);
#11271=VERTEX_POINT('',#49955);
#11272=VERTEX_POINT('',#49959);
#11273=VERTEX_POINT('',#49961);
#11274=VERTEX_POINT('',#49963);
#11275=VERTEX_POINT('',#49966);
#11276=VERTEX_POINT('',#49970);
#11277=VERTEX_POINT('',#49971);
#11278=VERTEX_POINT('',#49975);
#11279=VERTEX_POINT('',#49977);
#11280=VERTEX_POINT('',#49979);
#11281=VERTEX_POINT('',#49982);
#11282=VERTEX_POINT('',#49987);
#11283=VERTEX_POINT('',#49989);
#11284=VERTEX_POINT('',#49991);
#11285=VERTEX_POINT('',#49993);
#11286=VERTEX_POINT('',#49998);
#11287=VERTEX_POINT('',#50000);
#11288=VERTEX_POINT('',#50002);
#11289=VERTEX_POINT('',#50004);
#11290=VERTEX_POINT('',#50008);
#11291=VERTEX_POINT('',#50010);
#11292=VERTEX_POINT('',#50012);
#11293=VERTEX_POINT('',#50014);
#11294=VERTEX_POINT('',#50017);
#11295=VERTEX_POINT('',#50019);
#11296=VERTEX_POINT('',#50021);
#11297=VERTEX_POINT('',#50023);
#11298=VERTEX_POINT('',#50027);
#11299=VERTEX_POINT('',#50031);
#11300=VERTEX_POINT('',#50035);
#11301=VERTEX_POINT('',#50039);
#11302=VERTEX_POINT('',#50045);
#11303=VERTEX_POINT('',#50049);
#11304=VERTEX_POINT('',#50053);
#11305=VERTEX_POINT('',#50057);
#11306=VERTEX_POINT('',#50065);
#11307=VERTEX_POINT('',#50066);
#11308=VERTEX_POINT('',#50068);
#11309=VERTEX_POINT('',#50070);
#11310=VERTEX_POINT('',#50074);
#11311=VERTEX_POINT('',#50076);
#11312=VERTEX_POINT('',#50080);
#11313=VERTEX_POINT('',#50082);
#11314=VERTEX_POINT('',#50086);
#11315=VERTEX_POINT('',#50088);
#11316=VERTEX_POINT('',#50092);
#11317=VERTEX_POINT('',#50094);
#11318=VERTEX_POINT('',#50098);
#11319=VERTEX_POINT('',#50100);
#11320=VERTEX_POINT('',#50104);
#11321=VERTEX_POINT('',#50106);
#11322=VERTEX_POINT('',#50116);
#11323=VERTEX_POINT('',#50117);
#11324=VERTEX_POINT('',#50119);
#11325=VERTEX_POINT('',#50121);
#11326=VERTEX_POINT('',#50125);
#11327=VERTEX_POINT('',#50127);
#11328=VERTEX_POINT('',#50131);
#11329=VERTEX_POINT('',#50133);
#11330=VERTEX_POINT('',#50137);
#11331=VERTEX_POINT('',#50139);
#11332=VERTEX_POINT('',#50143);
#11333=VERTEX_POINT('',#50145);
#11334=VERTEX_POINT('',#50149);
#11335=VERTEX_POINT('',#50151);
#11336=VERTEX_POINT('',#50155);
#11337=VERTEX_POINT('',#50157);
#11338=VERTEX_POINT('',#50170);
#11339=VERTEX_POINT('',#50172);
#11340=VERTEX_POINT('',#50176);
#11341=VERTEX_POINT('',#50180);
#11342=VERTEX_POINT('',#50183);
#11343=VERTEX_POINT('',#50189);
#11344=VERTEX_POINT('',#50190);
#11345=VERTEX_POINT('',#50192);
#11346=VERTEX_POINT('',#50194);
#11347=VERTEX_POINT('',#50198);
#11348=VERTEX_POINT('',#50200);
#11349=VERTEX_POINT('',#50204);
#11350=VERTEX_POINT('',#50206);
#11351=VERTEX_POINT('',#50210);
#11352=VERTEX_POINT('',#50212);
#11353=VERTEX_POINT('',#50216);
#11354=VERTEX_POINT('',#50218);
#11355=VERTEX_POINT('',#50227);
#11356=VERTEX_POINT('',#50229);
#11357=VERTEX_POINT('',#50232);
#11358=VERTEX_POINT('',#50237);
#11359=VERTEX_POINT('',#50240);
#11360=VERTEX_POINT('',#50244);
#11361=VERTEX_POINT('',#50248);
#11362=VERTEX_POINT('',#50252);
#11363=VERTEX_POINT('',#50255);
#11364=VERTEX_POINT('',#50262);
#11365=VERTEX_POINT('',#50263);
#11366=VERTEX_POINT('',#50265);
#11367=VERTEX_POINT('',#50291);
#11368=VERTEX_POINT('',#50334);
#11369=VERTEX_POINT('',#50335);
#11370=VERTEX_POINT('',#50421);
#11371=VERTEX_POINT('',#50422);
#11372=VERTEX_POINT('',#50511);
#11373=VERTEX_POINT('',#50512);
#11374=VERTEX_POINT('',#50598);
#11375=VERTEX_POINT('',#50599);
#11376=VERTEX_POINT('',#50688);
#11377=VERTEX_POINT('',#50689);
#11378=VERTEX_POINT('',#50775);
#11379=VERTEX_POINT('',#50776);
#11380=VERTEX_POINT('',#50862);
#11381=VERTEX_POINT('',#50863);
#11382=VERTEX_POINT('',#50952);
#11383=VERTEX_POINT('',#50953);
#11384=VERTEX_POINT('',#50955);
#11385=VERTEX_POINT('',#50968);
#11386=VERTEX_POINT('',#50969);
#11387=VERTEX_POINT('',#50971);
#11388=VERTEX_POINT('',#50979);
#11389=VERTEX_POINT('',#50994);
#11390=VERTEX_POINT('',#50995);
#11391=VERTEX_POINT('',#51031);
#11392=VERTEX_POINT('',#51032);
#11393=VERTEX_POINT('',#51068);
#11394=VERTEX_POINT('',#51069);
#11395=VERTEX_POINT('',#51106);
#11396=VERTEX_POINT('',#51107);
#11397=VERTEX_POINT('',#51143);
#11398=VERTEX_POINT('',#51144);
#11399=VERTEX_POINT('',#51180);
#11400=VERTEX_POINT('',#51181);
#11401=VERTEX_POINT('',#51218);
#11402=VERTEX_POINT('',#51219);
#11403=VERTEX_POINT('',#51256);
#11404=VERTEX_POINT('',#51257);
#11405=VERTEX_POINT('',#51259);
#11406=VERTEX_POINT('',#51265);
#11407=VERTEX_POINT('',#52329);
#11408=VERTEX_POINT('',#52421);
#11409=VERTEX_POINT('',#52422);
#11410=VERTEX_POINT('',#52426);
#11411=VERTEX_POINT('',#52428);
#11412=VERTEX_POINT('',#52430);
#11413=VERTEX_POINT('',#52433);
#11414=VERTEX_POINT('',#52437);
#11415=VERTEX_POINT('',#52441);
#11416=VERTEX_POINT('',#52445);
#11417=VERTEX_POINT('',#52446);
#11418=VERTEX_POINT('',#52452);
#11419=VERTEX_POINT('',#52457);
#11420=VERTEX_POINT('',#52463);
#11421=VERTEX_POINT('',#52466);
#11422=VERTEX_POINT('',#52470);
#11423=VERTEX_POINT('',#52474);
#11424=VERTEX_POINT('',#52478);
#11425=VERTEX_POINT('',#52481);
#11426=VERTEX_POINT('',#52485);
#11427=VERTEX_POINT('',#52489);
#11428=VERTEX_POINT('',#52494);
#11429=VERTEX_POINT('',#52495);
#11430=VERTEX_POINT('',#52497);
#11431=VERTEX_POINT('',#52499);
#11432=VERTEX_POINT('',#52503);
#11433=VERTEX_POINT('',#52505);
#11434=VERTEX_POINT('',#52509);
#11435=VERTEX_POINT('',#52511);
#11436=VERTEX_POINT('',#52515);
#11437=VERTEX_POINT('',#52517);
#11438=VERTEX_POINT('',#52521);
#11439=VERTEX_POINT('',#52523);
#11440=VERTEX_POINT('',#52533);
#11441=VERTEX_POINT('',#52536);
#11442=VERTEX_POINT('',#52540);
#11443=VERTEX_POINT('',#52544);
#11444=VERTEX_POINT('',#52548);
#11445=VERTEX_POINT('',#52551);
#11446=VERTEX_POINT('',#52555);
#11447=VERTEX_POINT('',#52559);
#11448=VERTEX_POINT('',#52564);
#11449=VERTEX_POINT('',#52565);
#11450=VERTEX_POINT('',#52567);
#11451=VERTEX_POINT('',#52569);
#11452=VERTEX_POINT('',#52573);
#11453=VERTEX_POINT('',#52575);
#11454=VERTEX_POINT('',#52579);
#11455=VERTEX_POINT('',#52581);
#11456=VERTEX_POINT('',#52585);
#11457=VERTEX_POINT('',#52587);
#11458=VERTEX_POINT('',#52591);
#11459=VERTEX_POINT('',#52593);
#11460=VERTEX_POINT('',#52624);
#11461=VERTEX_POINT('',#52625);
#11462=VERTEX_POINT('',#52627);
#11463=VERTEX_POINT('',#52647);
#11464=VERTEX_POINT('',#52654);
#11465=VERTEX_POINT('',#52655);
#11466=VERTEX_POINT('',#52741);
#11467=VERTEX_POINT('',#52742);
#11468=VERTEX_POINT('',#52831);
#11469=VERTEX_POINT('',#52832);
#11470=VERTEX_POINT('',#52918);
#11471=VERTEX_POINT('',#52919);
#11472=VERTEX_POINT('',#53005);
#11473=VERTEX_POINT('',#53006);
#11474=VERTEX_POINT('',#53092);
#11475=VERTEX_POINT('',#53093);
#11476=VERTEX_POINT('',#53179);
#11477=VERTEX_POINT('',#53180);
#11478=VERTEX_POINT('',#53266);
#11479=VERTEX_POINT('',#53267);
#11480=VERTEX_POINT('',#53338);
#11481=VERTEX_POINT('',#53339);
#11482=VERTEX_POINT('',#53389);
#11483=VERTEX_POINT('',#53390);
#11484=VERTEX_POINT('',#53437);
#11485=VERTEX_POINT('',#53438);
#11486=VERTEX_POINT('',#53485);
#11487=VERTEX_POINT('',#53486);
#11488=VERTEX_POINT('',#53536);
#11489=VERTEX_POINT('',#53537);
#11490=VERTEX_POINT('',#53587);
#11491=VERTEX_POINT('',#53588);
#11492=VERTEX_POINT('',#53635);
#11493=VERTEX_POINT('',#53636);
#11494=VERTEX_POINT('',#53686);
#11495=VERTEX_POINT('',#53687);
#11496=VERTEX_POINT('',#53737);
#11497=VERTEX_POINT('',#53738);
#11498=VERTEX_POINT('',#53785);
#11499=VERTEX_POINT('',#53786);
#11500=VERTEX_POINT('',#53833);
#11501=VERTEX_POINT('',#53834);
#11502=VERTEX_POINT('',#53884);
#11503=VERTEX_POINT('',#53885);
#11504=VERTEX_POINT('',#53935);
#11505=VERTEX_POINT('',#53936);
#11506=VERTEX_POINT('',#53983);
#11507=VERTEX_POINT('',#53984);
#11508=VERTEX_POINT('',#54034);
#11509=VERTEX_POINT('',#54035);
#11510=VERTEX_POINT('',#54085);
#11511=VERTEX_POINT('',#54086);
#11512=VERTEX_POINT('',#54133);
#11513=VERTEX_POINT('',#54134);
#11514=VERTEX_POINT('',#54181);
#11515=VERTEX_POINT('',#54182);
#11516=VERTEX_POINT('',#54232);
#11517=VERTEX_POINT('',#54233);
#11518=VERTEX_POINT('',#54283);
#11519=VERTEX_POINT('',#54284);
#11520=VERTEX_POINT('',#54331);
#11521=VERTEX_POINT('',#54332);
#11522=VERTEX_POINT('',#54382);
#11523=VERTEX_POINT('',#54383);
#11524=VERTEX_POINT('',#54433);
#11525=VERTEX_POINT('',#54434);
#11526=VERTEX_POINT('',#54481);
#11527=VERTEX_POINT('',#54482);
#11528=VERTEX_POINT('',#54529);
#11529=VERTEX_POINT('',#54530);
#11530=VERTEX_POINT('',#54580);
#11531=VERTEX_POINT('',#54581);
#11532=VERTEX_POINT('',#54631);
#11533=VERTEX_POINT('',#54632);
#11534=VERTEX_POINT('',#54679);
#11535=VERTEX_POINT('',#54680);
#11536=VERTEX_POINT('',#54730);
#11537=VERTEX_POINT('',#54731);
#11538=VERTEX_POINT('',#54781);
#11539=VERTEX_POINT('',#54782);
#11540=VERTEX_POINT('',#54829);
#11541=VERTEX_POINT('',#54830);
#11542=VERTEX_POINT('',#54877);
#11543=VERTEX_POINT('',#54878);
#11544=VERTEX_POINT('',#54928);
#11545=VERTEX_POINT('',#54929);
#11546=VERTEX_POINT('',#54979);
#11547=VERTEX_POINT('',#54980);
#11548=VERTEX_POINT('',#55027);
#11549=VERTEX_POINT('',#55028);
#11550=VERTEX_POINT('',#55078);
#11551=VERTEX_POINT('',#55079);
#11552=VERTEX_POINT('',#55129);
#11553=VERTEX_POINT('',#55130);
#11554=VERTEX_POINT('',#55177);
#11555=VERTEX_POINT('',#55178);
#11556=VERTEX_POINT('',#55225);
#11557=VERTEX_POINT('',#55226);
#11558=VERTEX_POINT('',#55276);
#11559=VERTEX_POINT('',#55277);
#11560=VERTEX_POINT('',#55327);
#11561=VERTEX_POINT('',#55328);
#11562=VERTEX_POINT('',#55375);
#11563=VERTEX_POINT('',#55376);
#11564=VERTEX_POINT('',#55426);
#11565=VERTEX_POINT('',#55427);
#11566=VERTEX_POINT('',#55477);
#11567=VERTEX_POINT('',#55478);
#11568=VERTEX_POINT('',#55525);
#11569=VERTEX_POINT('',#55526);
#11570=VERTEX_POINT('',#55573);
#11571=VERTEX_POINT('',#55574);
#11572=VERTEX_POINT('',#55624);
#11573=VERTEX_POINT('',#55625);
#11574=VERTEX_POINT('',#55690);
#11575=VERTEX_POINT('',#55691);
#11576=VERTEX_POINT('',#55780);
#11577=VERTEX_POINT('',#55781);
#11578=VERTEX_POINT('',#55867);
#11579=VERTEX_POINT('',#55868);
#11580=VERTEX_POINT('',#55954);
#11581=VERTEX_POINT('',#55955);
#11582=VERTEX_POINT('',#56041);
#11583=VERTEX_POINT('',#56042);
#11584=VERTEX_POINT('',#56128);
#11585=VERTEX_POINT('',#56129);
#11586=VERTEX_POINT('',#56215);
#11587=VERTEX_POINT('',#56216);
#11588=VERTEX_POINT('',#56305);
#11589=VERTEX_POINT('',#56306);
#11590=VERTEX_POINT('',#56308);
#11591=VERTEX_POINT('',#56315);
#11592=VERTEX_POINT('',#56316);
#11593=VERTEX_POINT('',#56335);
#11594=VERTEX_POINT('',#56351);
#11595=VERTEX_POINT('',#56352);
#11596=VERTEX_POINT('',#56389);
#11597=VERTEX_POINT('',#56390);
#11598=VERTEX_POINT('',#56425);
#11599=VERTEX_POINT('',#56426);
#11600=VERTEX_POINT('',#56463);
#11601=VERTEX_POINT('',#56464);
#11602=VERTEX_POINT('',#56499);
#11603=VERTEX_POINT('',#56500);
#11604=VERTEX_POINT('',#56537);
#11605=VERTEX_POINT('',#56538);
#11606=VERTEX_POINT('',#56574);
#11607=VERTEX_POINT('',#56575);
#11608=VERTEX_POINT('',#56609);
#11609=VERTEX_POINT('',#56610);
#11610=VERTEX_POINT('',#56636);
#11611=VERTEX_POINT('',#56637);
#11612=VERTEX_POINT('',#56660);
#11613=VERTEX_POINT('',#56661);
#11614=VERTEX_POINT('',#56684);
#11615=VERTEX_POINT('',#56685);
#11616=VERTEX_POINT('',#56708);
#11617=VERTEX_POINT('',#56709);
#11618=VERTEX_POINT('',#56734);
#11619=VERTEX_POINT('',#56735);
#11620=VERTEX_POINT('',#56758);
#11621=VERTEX_POINT('',#56759);
#11622=VERTEX_POINT('',#56782);
#11623=VERTEX_POINT('',#56783);
#11624=VERTEX_POINT('',#56808);
#11625=VERTEX_POINT('',#56809);
#11626=VERTEX_POINT('',#56832);
#11627=VERTEX_POINT('',#56833);
#11628=VERTEX_POINT('',#56856);
#11629=VERTEX_POINT('',#56857);
#11630=VERTEX_POINT('',#56880);
#11631=VERTEX_POINT('',#56881);
#11632=VERTEX_POINT('',#56906);
#11633=VERTEX_POINT('',#56907);
#11634=VERTEX_POINT('',#56930);
#11635=VERTEX_POINT('',#56931);
#11636=VERTEX_POINT('',#56954);
#11637=VERTEX_POINT('',#56955);
#11638=VERTEX_POINT('',#56980);
#11639=VERTEX_POINT('',#56981);
#11640=VERTEX_POINT('',#57004);
#11641=VERTEX_POINT('',#57005);
#11642=VERTEX_POINT('',#57028);
#11643=VERTEX_POINT('',#57029);
#11644=VERTEX_POINT('',#57052);
#11645=VERTEX_POINT('',#57053);
#11646=VERTEX_POINT('',#57078);
#11647=VERTEX_POINT('',#57079);
#11648=VERTEX_POINT('',#57102);
#11649=VERTEX_POINT('',#57103);
#11650=VERTEX_POINT('',#57126);
#11651=VERTEX_POINT('',#57127);
#11652=VERTEX_POINT('',#57152);
#11653=VERTEX_POINT('',#57153);
#11654=VERTEX_POINT('',#57176);
#11655=VERTEX_POINT('',#57177);
#11656=VERTEX_POINT('',#57200);
#11657=VERTEX_POINT('',#57201);
#11658=VERTEX_POINT('',#57224);
#11659=VERTEX_POINT('',#57225);
#11660=VERTEX_POINT('',#57250);
#11661=VERTEX_POINT('',#57251);
#11662=VERTEX_POINT('',#57274);
#11663=VERTEX_POINT('',#57275);
#11664=VERTEX_POINT('',#57298);
#11665=VERTEX_POINT('',#57299);
#11666=VERTEX_POINT('',#57324);
#11667=VERTEX_POINT('',#57325);
#11668=VERTEX_POINT('',#57348);
#11669=VERTEX_POINT('',#57349);
#11670=VERTEX_POINT('',#57372);
#11671=VERTEX_POINT('',#57373);
#11672=VERTEX_POINT('',#57396);
#11673=VERTEX_POINT('',#57397);
#11674=VERTEX_POINT('',#57422);
#11675=VERTEX_POINT('',#57423);
#11676=VERTEX_POINT('',#57446);
#11677=VERTEX_POINT('',#57447);
#11678=VERTEX_POINT('',#57470);
#11679=VERTEX_POINT('',#57471);
#11680=VERTEX_POINT('',#57496);
#11681=VERTEX_POINT('',#57497);
#11682=VERTEX_POINT('',#57520);
#11683=VERTEX_POINT('',#57521);
#11684=VERTEX_POINT('',#57544);
#11685=VERTEX_POINT('',#57545);
#11686=VERTEX_POINT('',#57568);
#11687=VERTEX_POINT('',#57569);
#11688=VERTEX_POINT('',#57594);
#11689=VERTEX_POINT('',#57595);
#11690=VERTEX_POINT('',#57618);
#11691=VERTEX_POINT('',#57619);
#11692=VERTEX_POINT('',#57642);
#11693=VERTEX_POINT('',#57643);
#11694=VERTEX_POINT('',#57668);
#11695=VERTEX_POINT('',#57669);
#11696=VERTEX_POINT('',#57692);
#11697=VERTEX_POINT('',#57693);
#11698=VERTEX_POINT('',#57716);
#11699=VERTEX_POINT('',#57717);
#11700=VERTEX_POINT('',#57741);
#11701=VERTEX_POINT('',#57742);
#11702=VERTEX_POINT('',#57768);
#11703=VERTEX_POINT('',#57769);
#11704=VERTEX_POINT('',#57805);
#11705=VERTEX_POINT('',#57806);
#11706=VERTEX_POINT('',#57841);
#11707=VERTEX_POINT('',#57842);
#11708=VERTEX_POINT('',#57879);
#11709=VERTEX_POINT('',#57880);
#11710=VERTEX_POINT('',#57915);
#11711=VERTEX_POINT('',#57916);
#11712=VERTEX_POINT('',#57953);
#11713=VERTEX_POINT('',#57954);
#11714=VERTEX_POINT('',#57990);
#11715=VERTEX_POINT('',#57991);
#11716=VERTEX_POINT('',#58027);
#11717=VERTEX_POINT('',#58029);
#11718=VERTEX_POINT('',#58067);
#11719=VERTEX_POINT('',#58107);
#11720=VERTEX_POINT('',#60103);
#11721=VERTEX_POINT('',#62188);
#11722=VERTEX_POINT('',#62240);
#11723=VERTEX_POINT('',#62241);
#11724=VERTEX_POINT('',#62243);
#11725=VERTEX_POINT('',#62245);
#11726=VERTEX_POINT('',#62249);
#11727=VERTEX_POINT('',#62251);
#11728=VERTEX_POINT('',#62255);
#11729=VERTEX_POINT('',#62259);
#11730=VERTEX_POINT('',#62265);
#11731=VERTEX_POINT('',#62267);
#11732=VERTEX_POINT('',#62272);
#11733=VERTEX_POINT('',#62276);
#11734=VERTEX_POINT('',#62283);
#11735=VERTEX_POINT('',#62285);
#11736=VERTEX_POINT('',#62289);
#11737=VERTEX_POINT('',#62291);
#11738=VERTEX_POINT('',#62298);
#11739=VERTEX_POINT('',#62299);
#11740=VERTEX_POINT('',#62303);
#11741=VERTEX_POINT('',#62304);
#11742=VERTEX_POINT('',#62313);
#11743=VERTEX_POINT('',#62337);
#11744=VERTEX_POINT('',#62339);
#11745=VERTEX_POINT('',#62379);
#11746=VERTEX_POINT('',#62381);
#11747=VERTEX_POINT('',#62385);
#11748=VERTEX_POINT('',#62387);
#11749=VERTEX_POINT('',#62394);
#11750=VERTEX_POINT('',#62396);
#11751=VERTEX_POINT('',#62400);
#11752=VERTEX_POINT('',#62401);
#11753=VERTEX_POINT('',#62405);
#11754=VERTEX_POINT('',#62406);
#11755=VERTEX_POINT('',#62413);
#11756=VERTEX_POINT('',#62431);
#11757=VERTEX_POINT('',#62433);
#11758=VERTEX_POINT('',#62473);
#11759=VERTEX_POINT('',#62474);
#11760=VERTEX_POINT('',#62476);
#11761=VERTEX_POINT('',#62478);
#11762=VERTEX_POINT('',#62480);
#11763=VERTEX_POINT('',#62482);
#11764=VERTEX_POINT('',#62486);
#11765=VERTEX_POINT('',#62488);
#11766=VERTEX_POINT('',#62492);
#11767=VERTEX_POINT('',#62494);
#11768=VERTEX_POINT('',#62496);
#11769=VERTEX_POINT('',#62498);
#11770=VERTEX_POINT('',#62502);
#11771=VERTEX_POINT('',#62506);
#11772=VERTEX_POINT('',#62518);
#11773=VERTEX_POINT('',#62520);
#11774=VERTEX_POINT('',#62524);
#11775=VERTEX_POINT('',#62526);
#11776=VERTEX_POINT('',#62533);
#11777=VERTEX_POINT('',#62535);
#11778=VERTEX_POINT('',#62539);
#11779=VERTEX_POINT('',#62541);
#11780=VERTEX_POINT('',#62548);
#11781=VERTEX_POINT('',#62549);
#11782=VERTEX_POINT('',#62551);
#11783=VERTEX_POINT('',#62553);
#11784=VERTEX_POINT('',#62555);
#11785=VERTEX_POINT('',#62557);
#11786=VERTEX_POINT('',#62559);
#11787=VERTEX_POINT('',#62561);
#11788=VERTEX_POINT('',#62565);
#11789=VERTEX_POINT('',#62567);
#11790=VERTEX_POINT('',#62571);
#11791=VERTEX_POINT('',#62575);
#11792=VERTEX_POINT('',#62579);
#11793=VERTEX_POINT('',#62583);
#11794=VERTEX_POINT('',#62584);
#11795=VERTEX_POINT('',#62587);
#11796=VERTEX_POINT('',#62599);
#11797=VERTEX_POINT('',#62600);
#11798=VERTEX_POINT('',#62602);
#11799=VERTEX_POINT('',#62604);
#11800=VERTEX_POINT('',#62608);
#11801=VERTEX_POINT('',#62610);
#11802=VERTEX_POINT('',#62614);
#11803=VERTEX_POINT('',#62616);
#11804=VERTEX_POINT('',#62620);
#11805=VERTEX_POINT('',#62622);
#11806=VERTEX_POINT('',#62626);
#11807=VERTEX_POINT('',#62628);
#11808=VERTEX_POINT('',#62636);
#11809=VERTEX_POINT('',#62639);
#11810=VERTEX_POINT('',#62643);
#11811=VERTEX_POINT('',#62647);
#11812=VERTEX_POINT('',#62653);
#11813=VERTEX_POINT('',#62655);
#11814=VERTEX_POINT('',#62659);
#11815=VERTEX_POINT('',#62661);
#11816=VERTEX_POINT('',#62668);
#11817=VERTEX_POINT('',#62671);
#11818=VERTEX_POINT('',#62675);
#11819=VERTEX_POINT('',#62679);
#11820=VERTEX_POINT('',#62683);
#11821=VERTEX_POINT('',#62686);
#11822=VERTEX_POINT('',#62690);
#11823=VERTEX_POINT('',#62694);
#11824=VERTEX_POINT('',#62699);
#11825=VERTEX_POINT('',#62700);
#11826=VERTEX_POINT('',#62702);
#11827=VERTEX_POINT('',#62704);
#11828=VERTEX_POINT('',#62708);
#11829=VERTEX_POINT('',#62710);
#11830=VERTEX_POINT('',#62714);
#11831=VERTEX_POINT('',#62716);
#11832=VERTEX_POINT('',#62720);
#11833=VERTEX_POINT('',#62722);
#11834=VERTEX_POINT('',#62726);
#11835=VERTEX_POINT('',#62728);
#11836=EDGE_CURVE('',#9773,#9773,#8880,.T.);
#11837=EDGE_CURVE('',#9773,#9774,#5906,.T.);
#11838=EDGE_CURVE('',#9774,#9774,#8881,.T.);
#11839=EDGE_CURVE('',#9775,#9775,#8882,.T.);
#11840=EDGE_CURVE('',#9775,#9776,#5907,.T.);
#11841=EDGE_CURVE('',#9776,#9776,#8883,.T.);
#11842=EDGE_CURVE('',#9777,#9777,#8884,.T.);
#11843=EDGE_CURVE('',#9777,#9778,#5908,.T.);
#11844=EDGE_CURVE('',#9778,#9778,#8885,.T.);
#11845=EDGE_CURVE('',#9779,#9779,#8886,.T.);
#11846=EDGE_CURVE('',#9779,#9780,#5909,.T.);
#11847=EDGE_CURVE('',#9780,#9780,#8887,.T.);
#11848=EDGE_CURVE('',#9781,#9781,#8888,.T.);
#11849=EDGE_CURVE('',#9781,#9782,#5910,.T.);
#11850=EDGE_CURVE('',#9782,#9782,#8889,.T.);
#11851=EDGE_CURVE('',#9783,#9783,#8890,.T.);
#11852=EDGE_CURVE('',#9783,#9784,#5911,.T.);
#11853=EDGE_CURVE('',#9784,#9784,#8891,.T.);
#11854=EDGE_CURVE('',#9785,#9785,#8892,.T.);
#11855=EDGE_CURVE('',#9785,#9786,#5912,.T.);
#11856=EDGE_CURVE('',#9786,#9786,#8893,.T.);
#11857=EDGE_CURVE('',#9787,#9787,#8894,.T.);
#11858=EDGE_CURVE('',#9787,#9788,#5913,.T.);
#11859=EDGE_CURVE('',#9788,#9788,#8895,.T.);
#11860=EDGE_CURVE('',#9789,#9789,#8896,.T.);
#11861=EDGE_CURVE('',#9789,#9790,#5914,.T.);
#11862=EDGE_CURVE('',#9790,#9790,#8897,.T.);
#11863=EDGE_CURVE('',#9791,#9791,#8898,.T.);
#11864=EDGE_CURVE('',#9791,#9792,#5915,.T.);
#11865=EDGE_CURVE('',#9792,#9792,#8899,.T.);
#11866=EDGE_CURVE('',#9793,#9794,#5916,.T.);
#11867=EDGE_CURVE('',#9794,#9795,#5917,.T.);
#11868=EDGE_CURVE('',#9796,#9795,#5918,.T.);
#11869=EDGE_CURVE('',#9793,#9796,#5919,.T.);
#11870=EDGE_CURVE('',#9797,#9793,#5920,.T.);
#11871=EDGE_CURVE('',#9798,#9796,#5921,.T.);
#11872=EDGE_CURVE('',#9797,#9798,#5922,.T.);
#11873=EDGE_CURVE('',#9799,#9797,#5923,.T.);
#11874=EDGE_CURVE('',#9800,#9798,#5924,.T.);
#11875=EDGE_CURVE('',#9799,#9800,#5925,.T.);
#11876=EDGE_CURVE('',#9794,#9799,#5926,.T.);
#11877=EDGE_CURVE('',#9795,#9800,#5927,.T.);
#11878=EDGE_CURVE('',#9801,#9802,#5928,.T.);
#11879=EDGE_CURVE('',#9802,#9803,#5929,.T.);
#11880=EDGE_CURVE('',#9804,#9803,#5930,.T.);
#11881=EDGE_CURVE('',#9801,#9804,#5931,.T.);
#11882=EDGE_CURVE('',#9805,#9801,#5932,.T.);
#11883=EDGE_CURVE('',#9806,#9804,#5933,.T.);
#11884=EDGE_CURVE('',#9805,#9806,#5934,.T.);
#11885=EDGE_CURVE('',#9807,#9805,#5935,.T.);
#11886=EDGE_CURVE('',#9808,#9806,#5936,.T.);
#11887=EDGE_CURVE('',#9807,#9808,#5937,.T.);
#11888=EDGE_CURVE('',#9802,#9807,#5938,.T.);
#11889=EDGE_CURVE('',#9803,#9808,#5939,.T.);
#11890=EDGE_CURVE('',#9809,#9810,#5940,.T.);
#11891=EDGE_CURVE('',#9810,#9811,#5941,.T.);
#11892=EDGE_CURVE('',#9812,#9811,#5942,.T.);
#11893=EDGE_CURVE('',#9809,#9812,#5943,.T.);
#11894=EDGE_CURVE('',#9813,#9809,#5944,.T.);
#11895=EDGE_CURVE('',#9814,#9812,#5945,.T.);
#11896=EDGE_CURVE('',#9813,#9814,#5946,.T.);
#11897=EDGE_CURVE('',#9815,#9813,#5947,.T.);
#11898=EDGE_CURVE('',#9816,#9814,#5948,.T.);
#11899=EDGE_CURVE('',#9815,#9816,#5949,.T.);
#11900=EDGE_CURVE('',#9810,#9815,#5950,.T.);
#11901=EDGE_CURVE('',#9811,#9816,#5951,.T.);
#11902=EDGE_CURVE('',#9817,#9818,#5952,.T.);
#11903=EDGE_CURVE('',#9819,#9817,#8900,.T.);
#11904=EDGE_CURVE('',#9819,#9820,#5953,.T.);
#11905=EDGE_CURVE('',#9818,#9820,#8901,.T.);
#11906=EDGE_CURVE('',#9821,#9822,#5954,.T.);
#11907=EDGE_CURVE('',#9823,#9821,#8902,.T.);
#11908=EDGE_CURVE('',#9823,#9824,#5955,.T.);
#11909=EDGE_CURVE('',#9822,#9824,#8903,.T.);
#11910=EDGE_CURVE('',#9825,#9825,#8904,.T.);
#11911=EDGE_CURVE('',#9825,#9826,#5956,.T.);
#11912=EDGE_CURVE('',#9826,#9826,#8905,.T.);
#11913=EDGE_CURVE('',#9827,#9827,#8906,.T.);
#11914=EDGE_CURVE('',#9827,#9828,#5957,.T.);
#11915=EDGE_CURVE('',#9828,#9828,#8907,.T.);
#11916=EDGE_CURVE('',#9829,#9829,#8908,.T.);
#11917=EDGE_CURVE('',#9829,#9830,#5958,.T.);
#11918=EDGE_CURVE('',#9830,#9830,#8909,.T.);
#11919=EDGE_CURVE('',#9831,#9831,#8910,.T.);
#11920=EDGE_CURVE('',#9831,#9832,#5959,.T.);
#11921=EDGE_CURVE('',#9832,#9832,#8911,.T.);
#11922=EDGE_CURVE('',#9833,#9833,#8912,.T.);
#11923=EDGE_CURVE('',#9833,#9834,#5960,.T.);
#11924=EDGE_CURVE('',#9834,#9834,#8913,.T.);
#11925=EDGE_CURVE('',#9835,#9835,#8914,.T.);
#11926=EDGE_CURVE('',#9824,#9822,#8915,.T.);
#11927=EDGE_CURVE('',#9823,#9824,#5961,.T.);
#11928=EDGE_CURVE('',#9821,#9823,#8916,.T.);
#11929=EDGE_CURVE('',#9836,#9836,#8917,.T.);
#11930=EDGE_CURVE('',#9837,#9837,#8918,.T.);
#11931=EDGE_CURVE('',#9837,#9838,#5962,.T.);
#11932=EDGE_CURVE('',#9838,#9838,#8919,.T.);
#11933=EDGE_CURVE('',#9839,#9839,#8920,.T.);
#11934=EDGE_CURVE('',#9820,#9818,#8921,.T.);
#11935=EDGE_CURVE('',#9819,#9820,#5963,.T.);
#11936=EDGE_CURVE('',#9817,#9819,#8922,.T.);
#11937=EDGE_CURVE('',#9840,#9840,#8923,.T.);
#11938=EDGE_CURVE('',#9841,#9842,#5964,.T.);
#11939=EDGE_CURVE('',#9842,#9843,#5965,.T.);
#11940=EDGE_CURVE('',#9843,#9844,#5966,.T.);
#11941=EDGE_CURVE('',#9844,#9820,#5967,.T.);
#11942=EDGE_CURVE('',#9820,#9824,#5968,.T.);
#11943=EDGE_CURVE('',#9824,#9841,#5969,.T.);
#11944=EDGE_CURVE('',#9845,#9845,#8924,.T.);
#11945=EDGE_CURVE('',#9845,#9835,#5970,.T.);
#11946=EDGE_CURVE('',#9846,#9846,#8925,.T.);
#11947=EDGE_CURVE('',#9846,#9836,#5971,.T.);
#11948=EDGE_CURVE('',#9847,#9847,#8926,.T.);
#11949=EDGE_CURVE('',#9847,#9839,#5972,.T.);
#11950=EDGE_CURVE('',#9848,#9848,#8927,.T.);
#11951=EDGE_CURVE('',#9848,#9840,#5973,.T.);
#11952=EDGE_CURVE('',#9849,#9850,#5974,.T.);
#11953=EDGE_CURVE('',#9850,#9841,#5975,.T.);
#11954=EDGE_CURVE('',#9849,#9844,#5976,.T.);
#11955=EDGE_CURVE('',#9851,#9849,#5977,.T.);
#11956=EDGE_CURVE('',#9851,#9843,#5978,.T.);
#11957=EDGE_CURVE('',#9852,#9851,#5979,.T.);
#11958=EDGE_CURVE('',#9852,#9842,#5980,.T.);
#11959=EDGE_CURVE('',#9850,#9852,#5981,.T.);
#11960=EDGE_CURVE('',#9853,#9853,#8928,.T.);
#11961=EDGE_CURVE('',#9853,#9854,#5982,.T.);
#11962=EDGE_CURVE('',#9854,#9854,#8929,.T.);
#11963=EDGE_CURVE('',#9855,#9855,#8930,.T.);
#11964=EDGE_CURVE('',#9855,#9856,#5983,.T.);
#11965=EDGE_CURVE('',#9856,#9856,#8931,.T.);
#11966=EDGE_CURVE('',#9857,#9857,#8932,.T.);
#11967=EDGE_CURVE('',#9857,#9858,#5984,.T.);
#11968=EDGE_CURVE('',#9858,#9858,#8933,.T.);
#11969=EDGE_CURVE('',#9859,#9859,#8934,.T.);
#11970=EDGE_CURVE('',#9859,#9860,#5985,.T.);
#11971=EDGE_CURVE('',#9860,#9860,#8935,.T.);
#11972=EDGE_CURVE('',#9861,#9861,#8936,.T.);
#11973=EDGE_CURVE('',#9861,#9862,#5986,.T.);
#11974=EDGE_CURVE('',#9862,#9862,#8937,.T.);
#11975=EDGE_CURVE('',#9863,#9863,#8938,.T.);
#11976=EDGE_CURVE('',#9863,#9864,#5987,.T.);
#11977=EDGE_CURVE('',#9864,#9864,#8939,.T.);
#11978=EDGE_CURVE('',#9865,#9865,#8940,.T.);
#11979=EDGE_CURVE('',#9865,#9866,#5988,.T.);
#11980=EDGE_CURVE('',#9866,#9866,#8941,.T.);
#11981=EDGE_CURVE('',#9867,#9868,#5989,.T.);
#11982=EDGE_CURVE('',#9868,#9869,#5990,.T.);
#11983=EDGE_CURVE('',#9870,#9869,#5991,.T.);
#11984=EDGE_CURVE('',#9867,#9870,#5992,.T.);
#11985=EDGE_CURVE('',#9871,#9867,#5993,.T.);
#11986=EDGE_CURVE('',#9872,#9870,#5994,.T.);
#11987=EDGE_CURVE('',#9871,#9872,#5995,.T.);
#11988=EDGE_CURVE('',#9873,#9871,#5996,.T.);
#11989=EDGE_CURVE('',#9874,#9872,#5997,.T.);
#11990=EDGE_CURVE('',#9873,#9874,#5998,.T.);
#11991=EDGE_CURVE('',#9868,#9873,#5999,.T.);
#11992=EDGE_CURVE('',#9869,#9874,#6000,.T.);
#11993=EDGE_CURVE('',#9875,#9875,#8942,.T.);
#11994=EDGE_CURVE('',#9875,#9876,#6001,.T.);
#11995=EDGE_CURVE('',#9876,#9876,#8943,.T.);
#11996=EDGE_CURVE('',#9877,#9877,#8944,.T.);
#11997=EDGE_CURVE('',#9877,#9878,#6002,.T.);
#11998=EDGE_CURVE('',#9878,#9878,#8945,.T.);
#11999=EDGE_CURVE('',#9879,#9879,#8946,.T.);
#12000=EDGE_CURVE('',#9879,#9880,#6003,.T.);
#12001=EDGE_CURVE('',#9880,#9880,#8947,.T.);
#12002=EDGE_CURVE('',#9881,#9881,#8948,.T.);
#12003=EDGE_CURVE('',#9881,#9882,#6004,.T.);
#12004=EDGE_CURVE('',#9882,#9882,#8949,.T.);
#12005=EDGE_CURVE('',#9883,#9883,#8950,.T.);
#12006=EDGE_CURVE('',#9883,#9884,#6005,.T.);
#12007=EDGE_CURVE('',#9884,#9884,#8951,.T.);
#12008=EDGE_CURVE('',#9885,#9885,#8952,.T.);
#12009=EDGE_CURVE('',#9885,#9886,#6006,.T.);
#12010=EDGE_CURVE('',#9886,#9886,#8953,.T.);
#12011=EDGE_CURVE('',#9887,#9887,#8954,.T.);
#12012=EDGE_CURVE('',#9887,#9888,#6007,.T.);
#12013=EDGE_CURVE('',#9888,#9888,#8955,.T.);
#12014=EDGE_CURVE('',#9889,#9889,#8956,.T.);
#12015=EDGE_CURVE('',#9889,#9890,#6008,.T.);
#12016=EDGE_CURVE('',#9890,#9890,#8957,.T.);
#12017=EDGE_CURVE('',#9891,#9891,#8958,.T.);
#12018=EDGE_CURVE('',#9891,#9892,#6009,.T.);
#12019=EDGE_CURVE('',#9892,#9892,#8959,.T.);
#12020=EDGE_CURVE('',#9893,#9893,#8960,.T.);
#12021=EDGE_CURVE('',#9893,#9894,#6010,.T.);
#12022=EDGE_CURVE('',#9894,#9894,#8961,.T.);
#12023=EDGE_CURVE('',#9895,#9895,#8962,.T.);
#12024=EDGE_CURVE('',#9896,#9896,#8963,.T.);
#12025=EDGE_CURVE('',#9896,#9895,#6011,.T.);
#12026=EDGE_CURVE('',#9897,#9897,#8964,.T.);
#12027=EDGE_CURVE('',#9897,#9898,#6012,.T.);
#12028=EDGE_CURVE('',#9898,#9898,#8965,.T.);
#12029=EDGE_CURVE('',#9899,#9899,#8966,.T.);
#12030=EDGE_CURVE('',#9899,#9900,#6013,.T.);
#12031=EDGE_CURVE('',#9900,#9900,#8967,.T.);
#12032=EDGE_CURVE('',#9901,#9902,#6014,.T.);
#12033=EDGE_CURVE('',#9902,#9903,#6015,.T.);
#12034=EDGE_CURVE('',#9904,#9903,#6016,.T.);
#12035=EDGE_CURVE('',#9901,#9904,#6017,.T.);
#12036=EDGE_CURVE('',#9905,#9901,#6018,.T.);
#12037=EDGE_CURVE('',#9906,#9904,#6019,.T.);
#12038=EDGE_CURVE('',#9905,#9906,#6020,.T.);
#12039=EDGE_CURVE('',#9907,#9905,#6021,.T.);
#12040=EDGE_CURVE('',#9908,#9906,#6022,.T.);
#12041=EDGE_CURVE('',#9907,#9908,#6023,.T.);
#12042=EDGE_CURVE('',#9902,#9907,#6024,.T.);
#12043=EDGE_CURVE('',#9903,#9908,#6025,.T.);
#12044=EDGE_CURVE('',#9909,#9909,#8968,.T.);
#12045=EDGE_CURVE('',#9909,#9910,#6026,.T.);
#12046=EDGE_CURVE('',#9910,#9910,#8969,.T.);
#12047=EDGE_CURVE('',#9911,#9911,#8970,.T.);
#12048=EDGE_CURVE('',#9911,#9912,#6027,.T.);
#12049=EDGE_CURVE('',#9912,#9912,#8971,.T.);
#12050=EDGE_CURVE('',#9913,#9913,#8972,.T.);
#12051=EDGE_CURVE('',#9913,#9914,#6028,.T.);
#12052=EDGE_CURVE('',#9914,#9914,#8973,.T.);
#12053=EDGE_CURVE('',#9915,#9916,#6029,.T.);
#12054=EDGE_CURVE('',#9917,#9915,#6030,.T.);
#12055=EDGE_CURVE('',#9918,#9917,#6031,.T.);
#12056=EDGE_CURVE('',#9916,#9918,#6032,.T.);
#12057=EDGE_CURVE('',#9917,#9915,#8974,.T.);
#12058=EDGE_CURVE('',#9919,#9919,#8975,.T.);
#12059=EDGE_CURVE('',#9918,#9916,#8976,.T.);
#12060=EDGE_CURVE('',#9919,#9920,#6033,.T.);
#12061=EDGE_CURVE('',#9920,#9920,#8977,.T.);
#12062=EDGE_CURVE('',#9921,#9921,#8978,.T.);
#12063=EDGE_CURVE('',#9922,#9922,#8979,.T.);
#12064=EDGE_CURVE('',#9922,#9921,#6034,.T.);
#12065=EDGE_CURVE('',#9923,#9923,#8980,.T.);
#12066=EDGE_CURVE('',#9923,#9924,#6035,.T.);
#12067=EDGE_CURVE('',#9924,#9924,#8981,.T.);
#12068=EDGE_CURVE('',#9925,#9925,#8982,.T.);
#12069=EDGE_CURVE('',#9926,#9926,#8983,.T.);
#12070=EDGE_CURVE('',#9926,#9925,#6036,.T.);
#12071=EDGE_CURVE('',#9927,#9928,#6037,.T.);
#12072=EDGE_CURVE('',#9928,#9929,#6038,.T.);
#12073=EDGE_CURVE('',#9930,#9929,#6039,.T.);
#12074=EDGE_CURVE('',#9927,#9930,#6040,.T.);
#12075=EDGE_CURVE('',#9931,#9927,#6041,.T.);
#12076=EDGE_CURVE('',#9932,#9930,#6042,.T.);
#12077=EDGE_CURVE('',#9931,#9932,#6043,.T.);
#12078=EDGE_CURVE('',#9933,#9931,#6044,.T.);
#12079=EDGE_CURVE('',#9934,#9932,#6045,.T.);
#12080=EDGE_CURVE('',#9933,#9934,#6046,.T.);
#12081=EDGE_CURVE('',#9928,#9933,#6047,.T.);
#12082=EDGE_CURVE('',#9929,#9934,#6048,.T.);
#12083=EDGE_CURVE('',#9935,#9935,#8984,.T.);
#12084=EDGE_CURVE('',#9935,#9936,#6049,.T.);
#12085=EDGE_CURVE('',#9936,#9936,#8985,.T.);
#12086=EDGE_CURVE('',#9937,#9937,#8986,.T.);
#12087=EDGE_CURVE('',#9938,#9938,#8987,.T.);
#12088=EDGE_CURVE('',#9938,#9937,#6050,.T.);
#12089=EDGE_CURVE('',#9939,#9940,#6051,.T.);
#12090=EDGE_CURVE('',#9940,#9941,#6052,.T.);
#12091=EDGE_CURVE('',#9942,#9941,#6053,.T.);
#12092=EDGE_CURVE('',#9939,#9942,#6054,.T.);
#12093=EDGE_CURVE('',#9943,#9939,#6055,.T.);
#12094=EDGE_CURVE('',#9944,#9942,#6056,.T.);
#12095=EDGE_CURVE('',#9943,#9944,#6057,.T.);
#12096=EDGE_CURVE('',#9945,#9943,#6058,.T.);
#12097=EDGE_CURVE('',#9946,#9944,#6059,.T.);
#12098=EDGE_CURVE('',#9945,#9946,#6060,.T.);
#12099=EDGE_CURVE('',#9940,#9945,#6061,.T.);
#12100=EDGE_CURVE('',#9941,#9946,#6062,.T.);
#12101=EDGE_CURVE('',#9947,#9947,#8988,.T.);
#12102=EDGE_CURVE('',#9947,#9948,#6063,.T.);
#12103=EDGE_CURVE('',#9948,#9948,#8989,.T.);
#12104=EDGE_CURVE('',#9949,#9949,#8990,.T.);
#12105=EDGE_CURVE('',#9950,#9950,#8991,.T.);
#12106=EDGE_CURVE('',#9950,#9951,#6064,.T.);
#12107=EDGE_CURVE('',#9951,#9951,#8992,.T.);
#12108=EDGE_CURVE('',#9952,#9952,#8993,.T.);
#12109=EDGE_CURVE('',#9953,#9953,#8994,.T.);
#12110=EDGE_CURVE('',#9953,#9954,#6065,.T.);
#12111=EDGE_CURVE('',#9954,#9954,#8995,.T.);
#12112=EDGE_CURVE('',#9955,#9955,#8996,.T.);
#12113=EDGE_CURVE('',#9956,#9956,#8997,.T.);
#12114=EDGE_CURVE('',#9956,#9957,#6066,.T.);
#12115=EDGE_CURVE('',#9957,#9957,#8998,.T.);
#12116=EDGE_CURVE('',#9958,#9958,#8999,.T.);
#12117=EDGE_CURVE('',#9959,#9959,#9000,.T.);
#12118=EDGE_CURVE('',#9959,#9949,#6067,.T.);
#12119=EDGE_CURVE('',#9960,#9960,#9001,.T.);
#12120=EDGE_CURVE('',#9960,#9952,#6068,.T.);
#12121=EDGE_CURVE('',#9961,#9961,#9002,.T.);
#12122=EDGE_CURVE('',#9961,#9955,#6069,.T.);
#12123=EDGE_CURVE('',#9962,#9962,#9003,.T.);
#12124=EDGE_CURVE('',#9962,#9958,#6070,.T.);
#12125=EDGE_CURVE('',#9963,#9964,#6071,.T.);
#12126=EDGE_CURVE('',#9964,#9965,#6072,.T.);
#12127=EDGE_CURVE('',#9966,#9965,#6073,.T.);
#12128=EDGE_CURVE('',#9963,#9966,#6074,.T.);
#12129=EDGE_CURVE('',#9967,#9963,#6075,.T.);
#12130=EDGE_CURVE('',#9968,#9966,#6076,.T.);
#12131=EDGE_CURVE('',#9967,#9968,#6077,.T.);
#12132=EDGE_CURVE('',#9969,#9967,#6078,.T.);
#12133=EDGE_CURVE('',#9970,#9968,#6079,.T.);
#12134=EDGE_CURVE('',#9969,#9970,#6080,.T.);
#12135=EDGE_CURVE('',#9971,#9969,#6081,.T.);
#12136=EDGE_CURVE('',#9972,#9970,#6082,.T.);
#12137=EDGE_CURVE('',#9971,#9972,#6083,.T.);
#12138=EDGE_CURVE('',#9973,#9971,#6084,.T.);
#12139=EDGE_CURVE('',#9974,#9972,#6085,.T.);
#12140=EDGE_CURVE('',#9973,#9974,#6086,.T.);
#12141=EDGE_CURVE('',#9975,#9973,#6087,.T.);
#12142=EDGE_CURVE('',#9976,#9974,#6088,.T.);
#12143=EDGE_CURVE('',#9975,#9976,#6089,.T.);
#12144=EDGE_CURVE('',#9977,#9975,#6090,.T.);
#12145=EDGE_CURVE('',#9978,#9976,#6091,.T.);
#12146=EDGE_CURVE('',#9977,#9978,#6092,.T.);
#12147=EDGE_CURVE('',#9979,#9977,#6093,.T.);
#12148=EDGE_CURVE('',#9980,#9978,#6094,.T.);
#12149=EDGE_CURVE('',#9979,#9980,#6095,.T.);
#12150=EDGE_CURVE('',#9981,#9979,#6096,.T.);
#12151=EDGE_CURVE('',#9982,#9980,#6097,.T.);
#12152=EDGE_CURVE('',#9981,#9982,#6098,.T.);
#12153=EDGE_CURVE('',#9983,#9981,#6099,.T.);
#12154=EDGE_CURVE('',#9984,#9982,#6100,.T.);
#12155=EDGE_CURVE('',#9983,#9984,#6101,.T.);
#12156=EDGE_CURVE('',#9985,#9983,#6102,.T.);
#12157=EDGE_CURVE('',#9986,#9984,#6103,.T.);
#12158=EDGE_CURVE('',#9985,#9986,#6104,.T.);
#12159=EDGE_CURVE('',#9964,#9985,#6105,.T.);
#12160=EDGE_CURVE('',#9965,#9986,#6106,.T.);
#12161=EDGE_CURVE('',#9987,#9988,#9004,.T.);
#12162=EDGE_CURVE('',#9988,#9987,#9005,.T.);
#12163=EDGE_CURVE('',#9988,#9989,#9006,.T.);
#12164=EDGE_CURVE('',#9990,#9989,#9007,.T.);
#12165=EDGE_CURVE('',#9989,#9990,#9008,.T.);
#12166=EDGE_CURVE('',#9990,#9991,#6107,.T.);
#12167=EDGE_CURVE('',#9991,#9991,#9009,.T.);
#12168=EDGE_CURVE('',#9992,#9992,#9010,.T.);
#12169=EDGE_CURVE('',#9992,#9993,#6108,.T.);
#12170=EDGE_CURVE('',#9993,#9993,#9011,.T.);
#12171=EDGE_CURVE('',#9993,#9994,#6109,.T.);
#12172=EDGE_CURVE('',#9994,#9994,#9012,.T.);
#12173=EDGE_CURVE('',#9995,#9995,#9013,.T.);
#12174=EDGE_CURVE('',#9995,#9987,#6110,.T.);
#12175=EDGE_CURVE('',#9996,#9996,#9014,.T.);
#12176=EDGE_CURVE('',#9996,#9992,#6111,.T.);
#12177=EDGE_CURVE('',#9997,#9998,#9015,.T.);
#12178=EDGE_CURVE('',#9998,#9997,#9016,.T.);
#12179=EDGE_CURVE('',#9998,#9999,#9017,.T.);
#12180=EDGE_CURVE('',#10000,#9999,#9018,.T.);
#12181=EDGE_CURVE('',#9999,#10000,#9019,.T.);
#12182=EDGE_CURVE('',#10001,#10001,#9020,.T.);
#12183=EDGE_CURVE('',#10001,#10000,#6112,.T.);
#12184=EDGE_CURVE('',#10002,#10002,#9021,.T.);
#12185=EDGE_CURVE('',#10003,#10003,#9022,.T.);
#12186=EDGE_CURVE('',#10004,#10004,#9023,.T.);
#12187=EDGE_CURVE('',#10004,#10002,#6113,.T.);
#12188=EDGE_CURVE('',#10005,#10005,#9024,.T.);
#12189=EDGE_CURVE('',#10005,#10004,#6114,.T.);
#12190=EDGE_CURVE('',#10006,#10006,#9025,.T.);
#12191=EDGE_CURVE('',#10006,#10005,#6115,.T.);
#12192=EDGE_CURVE('',#9997,#10003,#6116,.T.);
#12193=EDGE_CURVE('',#10007,#10008,#9026,.T.);
#12194=EDGE_CURVE('',#10009,#10010,#9027,.T.);
#12195=EDGE_CURVE('',#10011,#10012,#9028,.T.);
#12196=EDGE_CURVE('',#10013,#10014,#9029,.T.);
#12197=EDGE_CURVE('',#10015,#10016,#9030,.T.);
#12198=EDGE_CURVE('',#10017,#10018,#9031,.T.);
#12199=EDGE_CURVE('',#10019,#10020,#9032,.T.);
#12200=EDGE_CURVE('',#10021,#10022,#693,.T.);
#12201=EDGE_CURVE('',#10023,#10021,#9033,.T.);
#12202=EDGE_CURVE('',#10024,#10023,#694,.T.);
#12203=EDGE_CURVE('',#10022,#10024,#9034,.T.);
#12204=EDGE_CURVE('',#10025,#10023,#9035,.T.);
#12205=EDGE_CURVE('',#10025,#10026,#695,.T.);
#12206=EDGE_CURVE('',#10027,#10026,#9036,.T.);
#12207=EDGE_CURVE('',#10027,#10028,#696,.T.);
#12208=EDGE_CURVE('',#10029,#10028,#9037,.T.);
#12209=EDGE_CURVE('',#10029,#10030,#6117,.T.);
#12210=EDGE_CURVE('',#10030,#10030,#9038,.T.);
#12211=EDGE_CURVE('',#10031,#10029,#9039,.T.);
#12212=EDGE_CURVE('',#10031,#10032,#697,.T.);
#12213=EDGE_CURVE('',#10033,#10032,#9040,.T.);
#12214=EDGE_CURVE('',#10033,#10034,#698,.T.);
#12215=EDGE_CURVE('',#10035,#10034,#9041,.T.);
#12216=EDGE_CURVE('',#10035,#10036,#699,.T.);
#12217=EDGE_CURVE('',#10037,#10036,#9042,.T.);
#12218=EDGE_CURVE('',#10037,#10038,#700,.T.);
#12219=EDGE_CURVE('',#10024,#10038,#9043,.T.);
#12220=EDGE_CURVE('',#10021,#10039,#9044,.T.);
#12221=EDGE_CURVE('',#10039,#10025,#9045,.T.);
#12222=EDGE_CURVE('',#10040,#10039,#701,.T.);
#12223=EDGE_CURVE('',#10026,#10040,#9046,.T.);
#12224=EDGE_CURVE('',#10040,#10041,#9047,.T.);
#12225=EDGE_CURVE('',#10041,#10027,#9048,.T.);
#12226=EDGE_CURVE('',#10042,#10041,#702,.T.);
#12227=EDGE_CURVE('',#10028,#10042,#9049,.T.);
#12228=EDGE_CURVE('',#10042,#10043,#9050,.T.);
#12229=EDGE_CURVE('',#10043,#10044,#9051,.T.);
#12230=EDGE_CURVE('',#10044,#10031,#9052,.T.);
#12231=EDGE_CURVE('',#10045,#10044,#703,.T.);
#12232=EDGE_CURVE('',#10032,#10045,#9053,.T.);
#12233=EDGE_CURVE('',#10045,#10046,#9054,.T.);
#12234=EDGE_CURVE('',#10046,#10033,#9055,.T.);
#12235=EDGE_CURVE('',#10047,#10046,#704,.T.);
#12236=EDGE_CURVE('',#10034,#10047,#9056,.T.);
#12237=EDGE_CURVE('',#10047,#10048,#9057,.T.);
#12238=EDGE_CURVE('',#10048,#10035,#9058,.T.);
#12239=EDGE_CURVE('',#10049,#10048,#705,.T.);
#12240=EDGE_CURVE('',#10036,#10049,#9059,.T.);
#12241=EDGE_CURVE('',#10050,#10050,#9060,.T.);
#12242=EDGE_CURVE('',#10050,#10043,#6118,.T.);
#12243=EDGE_CURVE('',#10051,#10022,#9061,.T.);
#12244=EDGE_CURVE('',#10051,#10052,#706,.T.);
#12245=EDGE_CURVE('',#10049,#10052,#9062,.T.);
#12246=EDGE_CURVE('',#10038,#10051,#9063,.T.);
#12247=EDGE_CURVE('',#10052,#10037,#9064,.T.);
#12248=EDGE_CURVE('',#10053,#10053,#9065,.T.);
#12249=EDGE_CURVE('',#10054,#10054,#9066,.T.);
#12250=EDGE_CURVE('',#10055,#10055,#9067,.T.);
#12251=EDGE_CURVE('',#10055,#10053,#6119,.T.);
#12252=EDGE_CURVE('',#10056,#10056,#9068,.T.);
#12253=EDGE_CURVE('',#10056,#10054,#6120,.T.);
#12254=EDGE_CURVE('',#10057,#10057,#9069,.T.);
#12255=EDGE_CURVE('',#10058,#10058,#9070,.T.);
#12256=EDGE_CURVE('',#10059,#10059,#9071,.T.);
#12257=EDGE_CURVE('',#10059,#10057,#6121,.T.);
#12258=EDGE_CURVE('',#10060,#10060,#9072,.T.);
#12259=EDGE_CURVE('',#10060,#10058,#6122,.T.);
#12260=EDGE_CURVE('',#10061,#10062,#9073,.T.);
#12261=EDGE_CURVE('',#10062,#10061,#9074,.T.);
#12262=EDGE_CURVE('',#10062,#10063,#9075,.T.);
#12263=EDGE_CURVE('',#10064,#10063,#9076,.T.);
#12264=EDGE_CURVE('',#10063,#10064,#9077,.T.);
#12265=EDGE_CURVE('',#10064,#10065,#6123,.T.);
#12266=EDGE_CURVE('',#10065,#10065,#9078,.T.);
#12267=EDGE_CURVE('',#10066,#10066,#9079,.T.);
#12268=EDGE_CURVE('',#10066,#10067,#6124,.T.);
#12269=EDGE_CURVE('',#10067,#10067,#9080,.T.);
#12270=EDGE_CURVE('',#10067,#10068,#6125,.T.);
#12271=EDGE_CURVE('',#10068,#10068,#9081,.T.);
#12272=EDGE_CURVE('',#10069,#10069,#9082,.T.);
#12273=EDGE_CURVE('',#10069,#10061,#6126,.T.);
#12274=EDGE_CURVE('',#10070,#10070,#9083,.T.);
#12275=EDGE_CURVE('',#10070,#10066,#6127,.T.);
#12276=EDGE_CURVE('',#10071,#10072,#9084,.T.);
#12277=EDGE_CURVE('',#10072,#10071,#9085,.T.);
#12278=EDGE_CURVE('',#10072,#10073,#9086,.T.);
#12279=EDGE_CURVE('',#10074,#10073,#9087,.T.);
#12280=EDGE_CURVE('',#10073,#10074,#9088,.T.);
#12281=EDGE_CURVE('',#10075,#10075,#9089,.T.);
#12282=EDGE_CURVE('',#10075,#10074,#6128,.T.);
#12283=EDGE_CURVE('',#10076,#10076,#9090,.T.);
#12284=EDGE_CURVE('',#10077,#10077,#9091,.T.);
#12285=EDGE_CURVE('',#10078,#10078,#9092,.T.);
#12286=EDGE_CURVE('',#10078,#10076,#6129,.T.);
#12287=EDGE_CURVE('',#10079,#10079,#9093,.T.);
#12288=EDGE_CURVE('',#10079,#10078,#6130,.T.);
#12289=EDGE_CURVE('',#10080,#10080,#9094,.T.);
#12290=EDGE_CURVE('',#10080,#10079,#6131,.T.);
#12291=EDGE_CURVE('',#10071,#10077,#6132,.T.);
#12292=EDGE_CURVE('',#10081,#10082,#9095,.T.);
#12293=EDGE_CURVE('',#10083,#10084,#9096,.T.);
#12294=EDGE_CURVE('',#10085,#10086,#9097,.T.);
#12295=EDGE_CURVE('',#10087,#10088,#9098,.T.);
#12296=EDGE_CURVE('',#10089,#10090,#9099,.T.);
#12297=EDGE_CURVE('',#10091,#10092,#9100,.T.);
#12298=EDGE_CURVE('',#10093,#10094,#9101,.T.);
#12299=EDGE_CURVE('',#10095,#10096,#9102,.T.);
#12300=EDGE_CURVE('',#10097,#10098,#707,.T.);
#12301=EDGE_CURVE('',#10099,#10097,#9103,.T.);
#12302=EDGE_CURVE('',#10100,#10099,#708,.T.);
#12303=EDGE_CURVE('',#10098,#10100,#9104,.T.);
#12304=EDGE_CURVE('',#10101,#10099,#9105,.T.);
#12305=EDGE_CURVE('',#10101,#10102,#709,.T.);
#12306=EDGE_CURVE('',#10103,#10102,#9106,.T.);
#12307=EDGE_CURVE('',#10103,#10104,#710,.T.);
#12308=EDGE_CURVE('',#10105,#10104,#9107,.T.);
#12309=EDGE_CURVE('',#10105,#10106,#711,.T.);
#12310=EDGE_CURVE('',#10106,#10107,#6133,.T.);
#12311=EDGE_CURVE('',#10107,#10107,#9108,.T.);
#12312=EDGE_CURVE('',#10106,#10108,#712,.T.);
#12313=EDGE_CURVE('',#10109,#10108,#9109,.T.);
#12314=EDGE_CURVE('',#10109,#10110,#713,.T.);
#12315=EDGE_CURVE('',#10111,#10110,#9110,.T.);
#12316=EDGE_CURVE('',#10111,#10112,#714,.T.);
#12317=EDGE_CURVE('',#10113,#10112,#9111,.T.);
#12318=EDGE_CURVE('',#10113,#10114,#715,.T.);
#12319=EDGE_CURVE('',#10115,#10114,#9112,.T.);
#12320=EDGE_CURVE('',#10115,#10116,#716,.T.);
#12321=EDGE_CURVE('',#10100,#10116,#9113,.T.);
#12322=EDGE_CURVE('',#10097,#10117,#9114,.T.);
#12323=EDGE_CURVE('',#10117,#10101,#9115,.T.);
#12324=EDGE_CURVE('',#10118,#10117,#717,.T.);
#12325=EDGE_CURVE('',#10102,#10118,#9116,.T.);
#12326=EDGE_CURVE('',#10118,#10119,#9117,.T.);
#12327=EDGE_CURVE('',#10119,#10103,#9118,.T.);
#12328=EDGE_CURVE('',#10120,#10119,#718,.T.);
#12329=EDGE_CURVE('',#10104,#10120,#9119,.T.);
#12330=EDGE_CURVE('',#10120,#10121,#9120,.T.);
#12331=EDGE_CURVE('',#10121,#10105,#9121,.T.);
#12332=EDGE_CURVE('',#10122,#10123,#719,.T.);
#12333=EDGE_CURVE('',#10108,#10122,#9122,.T.);
#12334=EDGE_CURVE('',#10123,#10121,#720,.T.);
#12335=EDGE_CURVE('',#10122,#10124,#9123,.T.);
#12336=EDGE_CURVE('',#10124,#10109,#9124,.T.);
#12337=EDGE_CURVE('',#10125,#10124,#721,.T.);
#12338=EDGE_CURVE('',#10110,#10125,#9125,.T.);
#12339=EDGE_CURVE('',#10125,#10126,#9126,.T.);
#12340=EDGE_CURVE('',#10126,#10111,#9127,.T.);
#12341=EDGE_CURVE('',#10127,#10126,#722,.T.);
#12342=EDGE_CURVE('',#10112,#10127,#9128,.T.);
#12343=EDGE_CURVE('',#10127,#10128,#9129,.T.);
#12344=EDGE_CURVE('',#10128,#10113,#9130,.T.);
#12345=EDGE_CURVE('',#10129,#10128,#723,.T.);
#12346=EDGE_CURVE('',#10114,#10129,#9131,.T.);
#12347=EDGE_CURVE('',#10130,#10130,#9132,.T.);
#12348=EDGE_CURVE('',#10130,#10123,#6134,.T.);
#12349=EDGE_CURVE('',#10131,#10098,#9133,.T.);
#12350=EDGE_CURVE('',#10131,#10132,#724,.T.);
#12351=EDGE_CURVE('',#10129,#10132,#9134,.T.);
#12352=EDGE_CURVE('',#10116,#10131,#9135,.T.);
#12353=EDGE_CURVE('',#10132,#10115,#9136,.T.);
#12354=EDGE_CURVE('',#10133,#10133,#9137,.T.);
#12355=EDGE_CURVE('',#10134,#10134,#9138,.T.);
#12356=EDGE_CURVE('',#10135,#10135,#9139,.T.);
#12357=EDGE_CURVE('',#10135,#10133,#6135,.T.);
#12358=EDGE_CURVE('',#10136,#10136,#9140,.T.);
#12359=EDGE_CURVE('',#10136,#10134,#6136,.T.);
#12360=EDGE_CURVE('',#10137,#10137,#9141,.T.);
#12361=EDGE_CURVE('',#10138,#10138,#9142,.T.);
#12362=EDGE_CURVE('',#10139,#10139,#9143,.T.);
#12363=EDGE_CURVE('',#10139,#10137,#6137,.T.);
#12364=EDGE_CURVE('',#10140,#10140,#9144,.T.);
#12365=EDGE_CURVE('',#10140,#10138,#6138,.T.);
#12366=EDGE_CURVE('',#10141,#10141,#9145,.T.);
#12367=EDGE_CURVE('',#10141,#10142,#6139,.T.);
#12368=EDGE_CURVE('',#10142,#10142,#9146,.T.);
#12369=EDGE_CURVE('',#10143,#10143,#9147,.T.);
#12370=EDGE_CURVE('',#10143,#10144,#6140,.T.);
#12371=EDGE_CURVE('',#10144,#10144,#9148,.T.);
#12372=EDGE_CURVE('',#10145,#10145,#9149,.T.);
#12373=EDGE_CURVE('',#10145,#10146,#6141,.T.);
#12374=EDGE_CURVE('',#10146,#10146,#9150,.T.);
#12375=EDGE_CURVE('',#10147,#10147,#9151,.T.);
#12376=EDGE_CURVE('',#10147,#10148,#6142,.T.);
#12377=EDGE_CURVE('',#10148,#10148,#9152,.T.);
#12378=EDGE_CURVE('',#10149,#10150,#6143,.T.);
#12379=EDGE_CURVE('',#10150,#10151,#6144,.T.);
#12380=EDGE_CURVE('',#10152,#10151,#6145,.T.);
#12381=EDGE_CURVE('',#10149,#10152,#6146,.T.);
#12382=EDGE_CURVE('',#10153,#10149,#6147,.T.);
#12383=EDGE_CURVE('',#10154,#10152,#6148,.T.);
#12384=EDGE_CURVE('',#10153,#10154,#6149,.T.);
#12385=EDGE_CURVE('',#10155,#10153,#6150,.T.);
#12386=EDGE_CURVE('',#10156,#10154,#6151,.T.);
#12387=EDGE_CURVE('',#10155,#10156,#6152,.T.);
#12388=EDGE_CURVE('',#10150,#10155,#6153,.T.);
#12389=EDGE_CURVE('',#10151,#10156,#6154,.T.);
#12390=EDGE_CURVE('',#10157,#10157,#9153,.T.);
#12391=EDGE_CURVE('',#10157,#10158,#6155,.T.);
#12392=EDGE_CURVE('',#10158,#10158,#9154,.T.);
#12393=EDGE_CURVE('',#10159,#10159,#9155,.T.);
#12394=EDGE_CURVE('',#10159,#10160,#6156,.T.);
#12395=EDGE_CURVE('',#10160,#10160,#9156,.T.);
#12396=EDGE_CURVE('',#10161,#10161,#9157,.T.);
#12397=EDGE_CURVE('',#10161,#10162,#6157,.T.);
#12398=EDGE_CURVE('',#10162,#10162,#9158,.T.);
#12399=EDGE_CURVE('',#10163,#10163,#9159,.T.);
#12400=EDGE_CURVE('',#10163,#10164,#6158,.T.);
#12401=EDGE_CURVE('',#10164,#10164,#9160,.T.);
#12402=EDGE_CURVE('',#10165,#10165,#9161,.T.);
#12403=EDGE_CURVE('',#10165,#10166,#6159,.T.);
#12404=EDGE_CURVE('',#10166,#10166,#9162,.T.);
#12405=EDGE_CURVE('',#10167,#10167,#9163,.T.);
#12406=EDGE_CURVE('',#10167,#10168,#6160,.T.);
#12407=EDGE_CURVE('',#10168,#10168,#9164,.T.);
#12408=EDGE_CURVE('',#10169,#10169,#9165,.T.);
#12409=EDGE_CURVE('',#10169,#10170,#6161,.T.);
#12410=EDGE_CURVE('',#10170,#10170,#9166,.T.);
#12411=EDGE_CURVE('',#10171,#10171,#9167,.T.);
#12412=EDGE_CURVE('',#10171,#10172,#6162,.T.);
#12413=EDGE_CURVE('',#10172,#10172,#9168,.T.);
#12414=EDGE_CURVE('',#10173,#10173,#9169,.T.);
#12415=EDGE_CURVE('',#10173,#10174,#6163,.T.);
#12416=EDGE_CURVE('',#10174,#10174,#9170,.T.);
#12417=EDGE_CURVE('',#10175,#10175,#9171,.T.);
#12418=EDGE_CURVE('',#10175,#10176,#6164,.T.);
#12419=EDGE_CURVE('',#10176,#10176,#9172,.T.);
#12420=EDGE_CURVE('',#10177,#10177,#9173,.T.);
#12421=EDGE_CURVE('',#10177,#10178,#6165,.T.);
#12422=EDGE_CURVE('',#10178,#10178,#9174,.T.);
#12423=EDGE_CURVE('',#10179,#10179,#9175,.T.);
#12424=EDGE_CURVE('',#10179,#10180,#6166,.T.);
#12425=EDGE_CURVE('',#10180,#10180,#9176,.T.);
#12426=EDGE_CURVE('',#10181,#10182,#6167,.T.);
#12427=EDGE_CURVE('',#10182,#10183,#6168,.T.);
#12428=EDGE_CURVE('',#10184,#10183,#6169,.T.);
#12429=EDGE_CURVE('',#10181,#10184,#6170,.T.);
#12430=EDGE_CURVE('',#10185,#10181,#6171,.T.);
#12431=EDGE_CURVE('',#10186,#10184,#6172,.T.);
#12432=EDGE_CURVE('',#10185,#10186,#6173,.T.);
#12433=EDGE_CURVE('',#10187,#10185,#6174,.T.);
#12434=EDGE_CURVE('',#10188,#10186,#6175,.T.);
#12435=EDGE_CURVE('',#10187,#10188,#6176,.T.);
#12436=EDGE_CURVE('',#10182,#10187,#6177,.T.);
#12437=EDGE_CURVE('',#10183,#10188,#6178,.T.);
#12438=EDGE_CURVE('',#10189,#10189,#9177,.T.);
#12439=EDGE_CURVE('',#10189,#10190,#6179,.T.);
#12440=EDGE_CURVE('',#10190,#10190,#9178,.T.);
#12441=EDGE_CURVE('',#10191,#10191,#9179,.T.);
#12442=EDGE_CURVE('',#10191,#10192,#6180,.T.);
#12443=EDGE_CURVE('',#10192,#10192,#9180,.T.);
#12444=EDGE_CURVE('',#10193,#10193,#9181,.T.);
#12445=EDGE_CURVE('',#10193,#10194,#6181,.T.);
#12446=EDGE_CURVE('',#10194,#10194,#9182,.T.);
#12447=EDGE_CURVE('',#10195,#10195,#9183,.T.);
#12448=EDGE_CURVE('',#10195,#10196,#6182,.T.);
#12449=EDGE_CURVE('',#10196,#10196,#9184,.T.);
#12450=EDGE_CURVE('',#10197,#10197,#9185,.T.);
#12451=EDGE_CURVE('',#10197,#10198,#6183,.T.);
#12452=EDGE_CURVE('',#10198,#10198,#9186,.T.);
#12453=EDGE_CURVE('',#10199,#10199,#9187,.T.);
#12454=EDGE_CURVE('',#10199,#10200,#6184,.T.);
#12455=EDGE_CURVE('',#10200,#10200,#9188,.T.);
#12456=EDGE_CURVE('',#10201,#10201,#9189,.T.);
#12457=EDGE_CURVE('',#10201,#10202,#6185,.T.);
#12458=EDGE_CURVE('',#10202,#10202,#9190,.T.);
#12459=EDGE_CURVE('',#10203,#10203,#9191,.T.);
#12460=EDGE_CURVE('',#10203,#10204,#6186,.T.);
#12461=EDGE_CURVE('',#10204,#10204,#9192,.T.);
#12462=EDGE_CURVE('',#10205,#10206,#6187,.T.);
#12463=EDGE_CURVE('',#10206,#10207,#6188,.T.);
#12464=EDGE_CURVE('',#10208,#10207,#6189,.T.);
#12465=EDGE_CURVE('',#10205,#10208,#6190,.T.);
#12466=EDGE_CURVE('',#10209,#10205,#6191,.T.);
#12467=EDGE_CURVE('',#10210,#10208,#6192,.T.);
#12468=EDGE_CURVE('',#10209,#10210,#6193,.T.);
#12469=EDGE_CURVE('',#10211,#10209,#6194,.T.);
#12470=EDGE_CURVE('',#10212,#10210,#6195,.T.);
#12471=EDGE_CURVE('',#10211,#10212,#6196,.T.);
#12472=EDGE_CURVE('',#10206,#10211,#6197,.T.);
#12473=EDGE_CURVE('',#10207,#10212,#6198,.T.);
#12474=EDGE_CURVE('',#10213,#10214,#6199,.T.);
#12475=EDGE_CURVE('',#10213,#10214,#9193,.T.);
#12476=EDGE_CURVE('',#10215,#10213,#6200,.T.);
#12477=EDGE_CURVE('',#10216,#10215,#9194,.T.);
#12478=EDGE_CURVE('',#10216,#10217,#6201,.T.);
#12479=EDGE_CURVE('',#10217,#10217,#9195,.T.);
#12480=EDGE_CURVE('',#10218,#10216,#9196,.T.);
#12481=EDGE_CURVE('',#10214,#10218,#6202,.T.);
#12482=EDGE_CURVE('',#10219,#10220,#6203,.T.);
#12483=EDGE_CURVE('',#10219,#10220,#9197,.T.);
#12484=EDGE_CURVE('',#10221,#10219,#6204,.T.);
#12485=EDGE_CURVE('',#10222,#10221,#9198,.T.);
#12486=EDGE_CURVE('',#10222,#10223,#6205,.T.);
#12487=EDGE_CURVE('',#10223,#10223,#9199,.T.);
#12488=EDGE_CURVE('',#10224,#10222,#9200,.T.);
#12489=EDGE_CURVE('',#10220,#10224,#6206,.T.);
#12490=EDGE_CURVE('',#10225,#10226,#6207,.T.);
#12491=EDGE_CURVE('',#10225,#10226,#9201,.T.);
#12492=EDGE_CURVE('',#10227,#10225,#6208,.T.);
#12493=EDGE_CURVE('',#10228,#10227,#9202,.T.);
#12494=EDGE_CURVE('',#10228,#10229,#6209,.T.);
#12495=EDGE_CURVE('',#10229,#10229,#9203,.T.);
#12496=EDGE_CURVE('',#10230,#10228,#9204,.T.);
#12497=EDGE_CURVE('',#10226,#10230,#6210,.T.);
#12498=EDGE_CURVE('',#10231,#10232,#6211,.T.);
#12499=EDGE_CURVE('',#10231,#10232,#9205,.T.);
#12500=EDGE_CURVE('',#10233,#10231,#6212,.T.);
#12501=EDGE_CURVE('',#10234,#10233,#9206,.T.);
#12502=EDGE_CURVE('',#10234,#10235,#6213,.T.);
#12503=EDGE_CURVE('',#10235,#10235,#9207,.T.);
#12504=EDGE_CURVE('',#10236,#10234,#9208,.T.);
#12505=EDGE_CURVE('',#10232,#10236,#6214,.T.);
#12506=EDGE_CURVE('',#10218,#10227,#6215,.T.);
#12507=EDGE_CURVE('',#10230,#10237,#6216,.T.);
#12508=EDGE_CURVE('',#10238,#10237,#6217,.T.);
#12509=EDGE_CURVE('',#10238,#10239,#6218,.T.);
#12510=EDGE_CURVE('',#10240,#10239,#6219,.T.);
#12511=EDGE_CURVE('',#10240,#10215,#6220,.T.);
#12512=EDGE_CURVE('',#10224,#10233,#6221,.T.);
#12513=EDGE_CURVE('',#10236,#10241,#6222,.T.);
#12514=EDGE_CURVE('',#10242,#10241,#6223,.T.);
#12515=EDGE_CURVE('',#10243,#10242,#6224,.T.);
#12516=EDGE_CURVE('',#10244,#10243,#6225,.T.);
#12517=EDGE_CURVE('',#10244,#10221,#6226,.T.);
#12518=EDGE_CURVE('',#10237,#10245,#6227,.T.);
#12519=EDGE_CURVE('',#10245,#10246,#6228,.T.);
#12520=EDGE_CURVE('',#10246,#10247,#6229,.T.);
#12521=EDGE_CURVE('',#10247,#10248,#6230,.T.);
#12522=EDGE_CURVE('',#10248,#10244,#6231,.T.);
#12523=EDGE_CURVE('',#10243,#10249,#6232,.T.);
#12524=EDGE_CURVE('',#10249,#10250,#6233,.T.);
#12525=EDGE_CURVE('',#10250,#10251,#6234,.T.);
#12526=EDGE_CURVE('',#10251,#10252,#6235,.T.);
#12527=EDGE_CURVE('',#10252,#10238,#6236,.T.);
#12528=EDGE_CURVE('',#10253,#10240,#6237,.T.);
#12529=EDGE_CURVE('',#10245,#10253,#6238,.T.);
#12530=EDGE_CURVE('',#10254,#10253,#6239,.T.);
#12531=EDGE_CURVE('',#10246,#10254,#6240,.T.);
#12532=EDGE_CURVE('',#10255,#10254,#6241,.T.);
#12533=EDGE_CURVE('',#10247,#10255,#6242,.T.);
#12534=EDGE_CURVE('',#10256,#10255,#6243,.T.);
#12535=EDGE_CURVE('',#10248,#10256,#6244,.T.);
#12536=EDGE_CURVE('',#10241,#10256,#6245,.T.);
#12537=EDGE_CURVE('',#10257,#10242,#6246,.T.);
#12538=EDGE_CURVE('',#10249,#10257,#6247,.T.);
#12539=EDGE_CURVE('',#10258,#10257,#6248,.T.);
#12540=EDGE_CURVE('',#10250,#10258,#6249,.T.);
#12541=EDGE_CURVE('',#10259,#10258,#6250,.T.);
#12542=EDGE_CURVE('',#10251,#10259,#6251,.T.);
#12543=EDGE_CURVE('',#10260,#10259,#6252,.T.);
#12544=EDGE_CURVE('',#10252,#10260,#6253,.T.);
#12545=EDGE_CURVE('',#10239,#10260,#6254,.T.);
#12546=EDGE_CURVE('',#10261,#10262,#6255,.T.);
#12547=EDGE_CURVE('',#10262,#10263,#6256,.T.);
#12548=EDGE_CURVE('',#10264,#10263,#6257,.T.);
#12549=EDGE_CURVE('',#10261,#10264,#6258,.T.);
#12550=EDGE_CURVE('',#10265,#10261,#6259,.T.);
#12551=EDGE_CURVE('',#10266,#10264,#6260,.T.);
#12552=EDGE_CURVE('',#10265,#10266,#6261,.T.);
#12553=EDGE_CURVE('',#10267,#10265,#6262,.T.);
#12554=EDGE_CURVE('',#10268,#10266,#6263,.T.);
#12555=EDGE_CURVE('',#10267,#10268,#6264,.T.);
#12556=EDGE_CURVE('',#10269,#10267,#6265,.T.);
#12557=EDGE_CURVE('',#10270,#10268,#6266,.T.);
#12558=EDGE_CURVE('',#10269,#10270,#6267,.T.);
#12559=EDGE_CURVE('',#10271,#10269,#6268,.T.);
#12560=EDGE_CURVE('',#10272,#10270,#6269,.T.);
#12561=EDGE_CURVE('',#10271,#10272,#6270,.T.);
#12562=EDGE_CURVE('',#10273,#10271,#6271,.T.);
#12563=EDGE_CURVE('',#10274,#10272,#6272,.T.);
#12564=EDGE_CURVE('',#10273,#10274,#6273,.T.);
#12565=EDGE_CURVE('',#10275,#10273,#6274,.T.);
#12566=EDGE_CURVE('',#10276,#10274,#6275,.T.);
#12567=EDGE_CURVE('',#10275,#10276,#6276,.T.);
#12568=EDGE_CURVE('',#10262,#10275,#6277,.T.);
#12569=EDGE_CURVE('',#10263,#10276,#6278,.T.);
#12570=EDGE_CURVE('',#10277,#10278,#6279,.T.);
#12571=EDGE_CURVE('',#10277,#10279,#6280,.T.);
#12572=EDGE_CURVE('',#10280,#10279,#6281,.T.);
#12573=EDGE_CURVE('',#10278,#10280,#6282,.T.);
#12574=EDGE_CURVE('',#10278,#10281,#6283,.T.);
#12575=EDGE_CURVE('',#10282,#10280,#6284,.T.);
#12576=EDGE_CURVE('',#10281,#10282,#6285,.T.);
#12577=EDGE_CURVE('',#10281,#10283,#6286,.T.);
#12578=EDGE_CURVE('',#10284,#10282,#6287,.T.);
#12579=EDGE_CURVE('',#10283,#10284,#6288,.T.);
#12580=EDGE_CURVE('',#10283,#10285,#6289,.T.);
#12581=EDGE_CURVE('',#10286,#10284,#6290,.T.);
#12582=EDGE_CURVE('',#10285,#10286,#6291,.T.);
#12583=EDGE_CURVE('',#10285,#10287,#6292,.T.);
#12584=EDGE_CURVE('',#10288,#10286,#6293,.T.);
#12585=EDGE_CURVE('',#10287,#10288,#6294,.T.);
#12586=EDGE_CURVE('',#10287,#10289,#6295,.T.);
#12587=EDGE_CURVE('',#10290,#10288,#6296,.T.);
#12588=EDGE_CURVE('',#10289,#10290,#6297,.T.);
#12589=EDGE_CURVE('',#10289,#10291,#6298,.T.);
#12590=EDGE_CURVE('',#10292,#10290,#6299,.T.);
#12591=EDGE_CURVE('',#10291,#10292,#6300,.T.);
#12592=EDGE_CURVE('',#10291,#10277,#6301,.T.);
#12593=EDGE_CURVE('',#10279,#10292,#6302,.T.);
#12594=EDGE_CURVE('',#10293,#10293,#9209,.T.);
#12595=EDGE_CURVE('',#10293,#10294,#6303,.T.);
#12596=EDGE_CURVE('',#10294,#10294,#9210,.T.);
#12597=EDGE_CURVE('',#10294,#10295,#6304,.T.);
#12598=EDGE_CURVE('',#10295,#10295,#9211,.T.);
#12599=EDGE_CURVE('',#10296,#10296,#9212,.T.);
#12600=EDGE_CURVE('',#10296,#10297,#6305,.T.);
#12601=EDGE_CURVE('',#10297,#10297,#9213,.T.);
#12602=EDGE_CURVE('',#10298,#10299,#6306,.T.);
#12603=EDGE_CURVE('',#10299,#10300,#6307,.T.);
#12604=EDGE_CURVE('',#10300,#10301,#6308,.T.);
#12605=EDGE_CURVE('',#10298,#10301,#6309,.T.);
#12606=EDGE_CURVE('',#10299,#10302,#6310,.T.);
#12607=EDGE_CURVE('',#10302,#10303,#6311,.T.);
#12608=EDGE_CURVE('',#10303,#10300,#6312,.T.);
#12609=EDGE_CURVE('',#10302,#10304,#6313,.T.);
#12610=EDGE_CURVE('',#10304,#10305,#6314,.T.);
#12611=EDGE_CURVE('',#10305,#10303,#6315,.T.);
#12612=EDGE_CURVE('',#10304,#10306,#6316,.T.);
#12613=EDGE_CURVE('',#10306,#10307,#6317,.T.);
#12614=EDGE_CURVE('',#10307,#10305,#6318,.T.);
#12615=EDGE_CURVE('',#10306,#10308,#6319,.T.);
#12616=EDGE_CURVE('',#10308,#10309,#6320,.T.);
#12617=EDGE_CURVE('',#10309,#10307,#6321,.T.);
#12618=EDGE_CURVE('',#10308,#10298,#6322,.T.);
#12619=EDGE_CURVE('',#10301,#10309,#6323,.T.);
#12620=EDGE_CURVE('',#10310,#10310,#9214,.T.);
#12621=EDGE_CURVE('',#10311,#10311,#9215,.T.);
#12622=EDGE_CURVE('',#10310,#10312,#6324,.T.);
#12623=EDGE_CURVE('',#10312,#10312,#9216,.T.);
#12624=EDGE_CURVE('',#10313,#10313,#9217,.T.);
#12625=EDGE_CURVE('',#10314,#10314,#9218,.T.);
#12626=EDGE_CURVE('',#10314,#10313,#6325,.T.);
#12627=EDGE_CURVE('',#10315,#10315,#9219,.T.);
#12628=EDGE_CURVE('',#10315,#10314,#6326,.T.);
#12629=EDGE_CURVE('',#10316,#10316,#9220,.T.);
#12630=EDGE_CURVE('',#10316,#10315,#6327,.T.);
#12631=EDGE_CURVE('',#10317,#10317,#9221,.T.);
#12632=EDGE_CURVE('',#10318,#10318,#9222,.F.);
#12633=EDGE_CURVE('',#10318,#10317,#6328,.T.);
#12634=EDGE_CURVE('',#10311,#10318,#6329,.T.);
#12635=EDGE_CURVE('',#10319,#10320,#6330,.T.);
#12636=EDGE_CURVE('',#10320,#10321,#725,.T.);
#12637=EDGE_CURVE('',#10321,#10322,#9223,.F.);
#12638=EDGE_CURVE('',#10322,#10319,#726,.T.);
#12639=EDGE_CURVE('',#10323,#10324,#6331,.T.);
#12640=EDGE_CURVE('',#10324,#10320,#727,.T.);
#12641=EDGE_CURVE('',#10319,#10323,#728,.T.);
#12642=EDGE_CURVE('',#10325,#10326,#6332,.T.);
#12643=EDGE_CURVE('',#10326,#10324,#729,.T.);
#12644=EDGE_CURVE('',#10323,#10325,#730,.T.);
#12645=EDGE_CURVE('',#10327,#10328,#6333,.T.);
#12646=EDGE_CURVE('',#10328,#10326,#731,.T.);
#12647=EDGE_CURVE('',#10325,#10327,#732,.T.);
#12648=EDGE_CURVE('',#10329,#10330,#6334,.T.);
#12649=EDGE_CURVE('',#10330,#10328,#733,.T.);
#12650=EDGE_CURVE('',#10327,#10329,#734,.T.);
#12651=EDGE_CURVE('',#10331,#10332,#6335,.T.);
#12652=EDGE_CURVE('',#10332,#10330,#735,.T.);
#12653=EDGE_CURVE('',#10329,#10331,#736,.T.);
#12654=EDGE_CURVE('',#10333,#10334,#6336,.T.);
#12655=EDGE_CURVE('',#10334,#10332,#737,.T.);
#12656=EDGE_CURVE('',#10331,#10333,#738,.T.);
#12657=EDGE_CURVE('',#10335,#10336,#6337,.T.);
#12658=EDGE_CURVE('',#10336,#10334,#739,.T.);
#12659=EDGE_CURVE('',#10333,#10335,#740,.T.);
#12660=EDGE_CURVE('',#10337,#10338,#6338,.T.);
#12661=EDGE_CURVE('',#10339,#10337,#9224,.F.);
#12662=EDGE_CURVE('',#10339,#10338,#741,.T.);
#12663=EDGE_CURVE('',#10340,#10341,#6339,.T.);
#12664=EDGE_CURVE('',#10341,#10342,#742,.T.);
#12665=EDGE_CURVE('',#10343,#10342,#9225,.T.);
#12666=EDGE_CURVE('',#10340,#10343,#743,.T.);
#12667=EDGE_CURVE('',#10344,#10345,#6340,.T.);
#12668=EDGE_CURVE('',#10345,#10341,#744,.T.);
#12669=EDGE_CURVE('',#10344,#10340,#745,.T.);
#12670=EDGE_CURVE('',#10346,#10347,#6341,.T.);
#12671=EDGE_CURVE('',#10347,#10345,#746,.T.);
#12672=EDGE_CURVE('',#10346,#10344,#747,.T.);
#12673=EDGE_CURVE('',#10348,#10349,#6342,.T.);
#12674=EDGE_CURVE('',#10349,#10347,#748,.T.);
#12675=EDGE_CURVE('',#10348,#10346,#749,.T.);
#12676=EDGE_CURVE('',#10350,#10351,#6343,.T.);
#12677=EDGE_CURVE('',#10351,#10349,#750,.T.);
#12678=EDGE_CURVE('',#10350,#10348,#751,.T.);
#12679=EDGE_CURVE('',#10352,#10353,#6344,.T.);
#12680=EDGE_CURVE('',#10353,#10351,#752,.T.);
#12681=EDGE_CURVE('',#10352,#10350,#753,.T.);
#12682=EDGE_CURVE('',#10354,#10355,#6345,.T.);
#12683=EDGE_CURVE('',#10355,#10353,#754,.T.);
#12684=EDGE_CURVE('',#10354,#10352,#755,.T.);
#12685=EDGE_CURVE('',#10356,#10357,#6346,.T.);
#12686=EDGE_CURVE('',#10357,#10355,#756,.T.);
#12687=EDGE_CURVE('',#10356,#10354,#757,.T.);
#12688=EDGE_CURVE('',#10358,#10359,#6347,.T.);
#12689=EDGE_CURVE('',#10360,#10358,#758,.T.);
#12690=EDGE_CURVE('',#10361,#10360,#9226,.T.);
#12691=EDGE_CURVE('',#10361,#10359,#759,.T.);
#12692=EDGE_CURVE('',#10359,#10357,#760,.T.);
#12693=EDGE_CURVE('',#10358,#10356,#761,.T.);
#12694=EDGE_CURVE('',#10342,#10339,#762,.T.);
#12695=EDGE_CURVE('',#10321,#10361,#763,.T.);
#12696=EDGE_CURVE('',#10338,#10336,#764,.T.);
#12697=EDGE_CURVE('',#10362,#10343,#765,.T.);
#12698=EDGE_CURVE('',#10335,#10362,#766,.T.);
#12699=EDGE_CURVE('',#10360,#10322,#767,.T.);
#12700=EDGE_CURVE('',#10363,#10364,#6348,.T.);
#12701=EDGE_CURVE('',#10364,#10363,#9227,.T.);
#12702=EDGE_CURVE('',#10337,#10362,#9228,.F.);
#12703=EDGE_CURVE('',#10365,#10365,#9229,.T.);
#12704=EDGE_CURVE('',#10366,#10366,#9230,.T.);
#12705=EDGE_CURVE('',#10367,#10367,#9231,.T.);
#12706=EDGE_CURVE('',#10368,#10368,#9232,.T.);
#12707=EDGE_CURVE('',#10368,#10367,#6349,.T.);
#12708=EDGE_CURVE('',#10369,#10369,#9233,.T.);
#12709=EDGE_CURVE('',#10369,#10366,#6350,.T.);
#12710=EDGE_CURVE('',#10370,#10370,#9234,.T.);
#12711=EDGE_CURVE('',#10370,#10365,#6351,.T.);
#12712=EDGE_CURVE('',#10371,#10372,#6352,.T.);
#12713=EDGE_CURVE('',#10364,#10371,#6353,.T.);
#12714=EDGE_CURVE('',#10372,#10363,#6354,.T.);
#12715=EDGE_CURVE('',#10371,#10372,#9235,.T.);
#12716=EDGE_CURVE('',#10373,#10373,#9236,.T.);
#12717=EDGE_CURVE('',#10373,#10374,#6355,.T.);
#12718=EDGE_CURVE('',#10374,#10374,#9237,.T.);
#12719=EDGE_CURVE('',#10375,#10375,#9238,.T.);
#12720=EDGE_CURVE('',#10376,#10376,#9239,.T.);
#12721=EDGE_CURVE('',#10376,#10375,#6356,.T.);
#12722=EDGE_CURVE('',#10377,#10377,#9240,.T.);
#12723=EDGE_CURVE('',#10377,#10376,#6357,.T.);
#12724=EDGE_CURVE('',#10378,#10378,#9241,.T.);
#12725=EDGE_CURVE('',#10378,#10377,#6358,.T.);
#12726=EDGE_CURVE('',#10379,#10379,#9242,.T.);
#12727=EDGE_CURVE('',#10380,#10380,#9243,.F.);
#12728=EDGE_CURVE('',#10380,#10379,#6359,.T.);
#12729=EDGE_CURVE('',#10381,#10381,#9244,.F.);
#12730=EDGE_CURVE('',#10381,#10380,#6360,.T.);
#12731=EDGE_CURVE('',#10382,#10382,#9245,.T.);
#12732=EDGE_CURVE('',#10382,#10381,#6361,.T.);
#12733=EDGE_CURVE('',#10383,#10384,#6362,.T.);
#12734=EDGE_CURVE('',#10384,#10385,#6363,.T.);
#12735=EDGE_CURVE('',#10385,#10386,#6364,.T.);
#12736=EDGE_CURVE('',#10383,#10386,#6365,.T.);
#12737=EDGE_CURVE('',#10384,#10387,#6366,.T.);
#12738=EDGE_CURVE('',#10387,#10388,#6367,.T.);
#12739=EDGE_CURVE('',#10388,#10385,#6368,.T.);
#12740=EDGE_CURVE('',#10387,#10389,#6369,.T.);
#12741=EDGE_CURVE('',#10389,#10390,#6370,.T.);
#12742=EDGE_CURVE('',#10390,#10388,#6371,.T.);
#12743=EDGE_CURVE('',#10389,#10391,#6372,.T.);
#12744=EDGE_CURVE('',#10391,#10392,#6373,.T.);
#12745=EDGE_CURVE('',#10392,#10390,#6374,.T.);
#12746=EDGE_CURVE('',#10391,#10393,#6375,.T.);
#12747=EDGE_CURVE('',#10393,#10394,#6376,.T.);
#12748=EDGE_CURVE('',#10394,#10392,#6377,.T.);
#12749=EDGE_CURVE('',#10393,#10383,#6378,.T.);
#12750=EDGE_CURVE('',#10386,#10394,#6379,.T.);
#12751=EDGE_CURVE('',#10395,#10395,#9246,.T.);
#12752=EDGE_CURVE('',#10396,#10396,#9247,.T.);
#12753=EDGE_CURVE('',#10396,#10395,#6380,.T.);
#12754=EDGE_CURVE('',#10397,#10397,#9248,.T.);
#12755=EDGE_CURVE('',#10397,#10396,#6381,.T.);
#12756=EDGE_CURVE('',#10398,#10398,#9249,.T.);
#12757=EDGE_CURVE('',#10398,#10397,#6382,.T.);
#12758=EDGE_CURVE('',#10399,#10399,#9250,.T.);
#12759=EDGE_CURVE('',#10400,#10400,#9251,.F.);
#12760=EDGE_CURVE('',#10400,#10399,#6383,.T.);
#12761=EDGE_CURVE('',#10401,#10401,#9252,.F.);
#12762=EDGE_CURVE('',#10401,#10400,#6384,.T.);
#12763=EDGE_CURVE('',#10402,#10402,#9253,.T.);
#12764=EDGE_CURVE('',#10402,#10401,#6385,.T.);
#12765=EDGE_CURVE('',#10403,#10404,#6386,.T.);
#12766=EDGE_CURVE('',#10404,#10405,#6387,.T.);
#12767=EDGE_CURVE('',#10405,#10406,#6388,.T.);
#12768=EDGE_CURVE('',#10403,#10406,#6389,.T.);
#12769=EDGE_CURVE('',#10404,#10407,#6390,.T.);
#12770=EDGE_CURVE('',#10407,#10408,#6391,.T.);
#12771=EDGE_CURVE('',#10408,#10405,#6392,.T.);
#12772=EDGE_CURVE('',#10407,#10409,#6393,.T.);
#12773=EDGE_CURVE('',#10409,#10410,#6394,.T.);
#12774=EDGE_CURVE('',#10410,#10408,#6395,.T.);
#12775=EDGE_CURVE('',#10409,#10411,#6396,.T.);
#12776=EDGE_CURVE('',#10411,#10412,#6397,.T.);
#12777=EDGE_CURVE('',#10412,#10410,#6398,.T.);
#12778=EDGE_CURVE('',#10411,#10413,#6399,.T.);
#12779=EDGE_CURVE('',#10413,#10414,#6400,.T.);
#12780=EDGE_CURVE('',#10414,#10412,#6401,.T.);
#12781=EDGE_CURVE('',#10413,#10403,#6402,.T.);
#12782=EDGE_CURVE('',#10406,#10414,#6403,.T.);
#12783=EDGE_CURVE('',#10415,#10416,#6404,.T.);
#12784=EDGE_CURVE('',#10415,#10417,#768,.T.);
#12785=EDGE_CURVE('',#10417,#10418,#9254,.F.);
#12786=EDGE_CURVE('',#10418,#10416,#769,.T.);
#12787=EDGE_CURVE('',#10419,#10420,#6405,.T.);
#12788=EDGE_CURVE('',#10419,#10415,#770,.T.);
#12789=EDGE_CURVE('',#10416,#10420,#771,.T.);
#12790=EDGE_CURVE('',#10421,#10422,#6406,.T.);
#12791=EDGE_CURVE('',#10421,#10419,#772,.T.);
#12792=EDGE_CURVE('',#10420,#10422,#773,.T.);
#12793=EDGE_CURVE('',#10423,#10424,#6407,.T.);
#12794=EDGE_CURVE('',#10423,#10421,#774,.T.);
#12795=EDGE_CURVE('',#10422,#10424,#775,.T.);
#12796=EDGE_CURVE('',#10425,#10426,#6408,.T.);
#12797=EDGE_CURVE('',#10425,#10423,#776,.T.);
#12798=EDGE_CURVE('',#10424,#10426,#777,.T.);
#12799=EDGE_CURVE('',#10427,#10428,#6409,.T.);
#12800=EDGE_CURVE('',#10427,#10425,#778,.T.);
#12801=EDGE_CURVE('',#10426,#10428,#779,.T.);
#12802=EDGE_CURVE('',#10429,#10430,#6410,.T.);
#12803=EDGE_CURVE('',#10429,#10427,#780,.T.);
#12804=EDGE_CURVE('',#10428,#10430,#781,.T.);
#12805=EDGE_CURVE('',#10431,#10432,#6411,.T.);
#12806=EDGE_CURVE('',#10431,#10429,#782,.T.);
#12807=EDGE_CURVE('',#10430,#10432,#783,.T.);
#12808=EDGE_CURVE('',#10433,#10434,#6412,.T.);
#12809=EDGE_CURVE('',#10433,#10431,#784,.T.);
#12810=EDGE_CURVE('',#10432,#10434,#785,.T.);
#12811=EDGE_CURVE('',#10435,#10436,#6413,.T.);
#12812=EDGE_CURVE('',#10435,#10433,#786,.T.);
#12813=EDGE_CURVE('',#10434,#10436,#787,.T.);
#12814=EDGE_CURVE('',#10437,#10438,#6414,.T.);
#12815=EDGE_CURVE('',#10437,#10435,#788,.T.);
#12816=EDGE_CURVE('',#10436,#10438,#789,.T.);
#12817=EDGE_CURVE('',#10439,#10440,#6415,.T.);
#12818=EDGE_CURVE('',#10439,#10437,#790,.T.);
#12819=EDGE_CURVE('',#10438,#10440,#791,.T.);
#12820=EDGE_CURVE('',#10441,#10442,#6416,.T.);
#12821=EDGE_CURVE('',#10441,#10439,#792,.T.);
#12822=EDGE_CURVE('',#10440,#10442,#793,.T.);
#12823=EDGE_CURVE('',#10443,#10444,#6417,.T.);
#12824=EDGE_CURVE('',#10443,#10441,#794,.T.);
#12825=EDGE_CURVE('',#10442,#10444,#795,.T.);
#12826=EDGE_CURVE('',#10445,#10446,#6418,.T.);
#12827=EDGE_CURVE('',#10445,#10443,#796,.T.);
#12828=EDGE_CURVE('',#10444,#10446,#797,.T.);
#12829=EDGE_CURVE('',#10447,#10448,#6419,.T.);
#12830=EDGE_CURVE('',#10447,#10445,#798,.T.);
#12831=EDGE_CURVE('',#10446,#10448,#799,.T.);
#12832=EDGE_CURVE('',#10449,#10450,#6420,.T.);
#12833=EDGE_CURVE('',#10449,#10447,#800,.T.);
#12834=EDGE_CURVE('',#10448,#10450,#801,.T.);
#12835=EDGE_CURVE('',#10451,#10452,#6421,.T.);
#12836=EDGE_CURVE('',#10451,#10449,#802,.T.);
#12837=EDGE_CURVE('',#10450,#10452,#803,.T.);
#12838=EDGE_CURVE('',#10453,#10454,#6422,.T.);
#12839=EDGE_CURVE('',#10453,#10451,#804,.T.);
#12840=EDGE_CURVE('',#10452,#10454,#805,.T.);
#12841=EDGE_CURVE('',#10455,#10456,#6423,.T.);
#12842=EDGE_CURVE('',#10455,#10453,#806,.T.);
#12843=EDGE_CURVE('',#10454,#10456,#807,.T.);
#12844=EDGE_CURVE('',#10457,#10458,#6424,.T.);
#12845=EDGE_CURVE('',#10457,#10455,#808,.T.);
#12846=EDGE_CURVE('',#10456,#10458,#809,.T.);
#12847=EDGE_CURVE('',#10459,#10460,#6425,.T.);
#12848=EDGE_CURVE('',#10459,#10457,#810,.T.);
#12849=EDGE_CURVE('',#10458,#10460,#811,.T.);
#12850=EDGE_CURVE('',#10461,#10462,#6426,.T.);
#12851=EDGE_CURVE('',#10461,#10459,#812,.T.);
#12852=EDGE_CURVE('',#10460,#10462,#813,.T.);
#12853=EDGE_CURVE('',#10463,#10464,#6427,.T.);
#12854=EDGE_CURVE('',#10463,#10461,#814,.T.);
#12855=EDGE_CURVE('',#10462,#10464,#815,.T.);
#12856=EDGE_CURVE('',#10465,#10466,#6428,.T.);
#12857=EDGE_CURVE('',#10465,#10463,#816,.T.);
#12858=EDGE_CURVE('',#10464,#10466,#817,.T.);
#12859=EDGE_CURVE('',#10467,#10468,#6429,.T.);
#12860=EDGE_CURVE('',#10467,#10465,#818,.T.);
#12861=EDGE_CURVE('',#10466,#10468,#819,.T.);
#12862=EDGE_CURVE('',#10469,#10470,#6430,.T.);
#12863=EDGE_CURVE('',#10469,#10467,#820,.T.);
#12864=EDGE_CURVE('',#10468,#10470,#821,.T.);
#12865=EDGE_CURVE('',#10471,#10472,#6431,.T.);
#12866=EDGE_CURVE('',#10471,#10469,#822,.T.);
#12867=EDGE_CURVE('',#10470,#10472,#823,.T.);
#12868=EDGE_CURVE('',#10473,#10474,#6432,.T.);
#12869=EDGE_CURVE('',#10473,#10471,#824,.T.);
#12870=EDGE_CURVE('',#10472,#10474,#825,.T.);
#12871=EDGE_CURVE('',#10475,#10476,#6433,.T.);
#12872=EDGE_CURVE('',#10475,#10473,#826,.T.);
#12873=EDGE_CURVE('',#10474,#10476,#827,.T.);
#12874=EDGE_CURVE('',#10477,#10478,#6434,.T.);
#12875=EDGE_CURVE('',#10477,#10475,#828,.T.);
#12876=EDGE_CURVE('',#10476,#10478,#829,.T.);
#12877=EDGE_CURVE('',#10479,#10480,#6435,.T.);
#12878=EDGE_CURVE('',#10479,#10477,#830,.T.);
#12879=EDGE_CURVE('',#10478,#10480,#831,.T.);
#12880=EDGE_CURVE('',#10481,#10482,#6436,.T.);
#12881=EDGE_CURVE('',#10481,#10479,#832,.T.);
#12882=EDGE_CURVE('',#10480,#10482,#833,.T.);
#12883=EDGE_CURVE('',#10483,#10484,#6437,.T.);
#12884=EDGE_CURVE('',#10483,#10481,#834,.T.);
#12885=EDGE_CURVE('',#10482,#10484,#835,.T.);
#12886=EDGE_CURVE('',#10485,#10486,#6438,.T.);
#12887=EDGE_CURVE('',#10485,#10483,#836,.T.);
#12888=EDGE_CURVE('',#10484,#10486,#837,.T.);
#12889=EDGE_CURVE('',#10487,#10488,#6439,.T.);
#12890=EDGE_CURVE('',#10487,#10485,#838,.T.);
#12891=EDGE_CURVE('',#10486,#10488,#839,.T.);
#12892=EDGE_CURVE('',#10489,#10490,#6440,.T.);
#12893=EDGE_CURVE('',#10489,#10487,#840,.T.);
#12894=EDGE_CURVE('',#10488,#10490,#841,.T.);
#12895=EDGE_CURVE('',#10491,#10492,#6441,.T.);
#12896=EDGE_CURVE('',#10491,#10489,#842,.T.);
#12897=EDGE_CURVE('',#10490,#10492,#843,.T.);
#12898=EDGE_CURVE('',#10493,#10494,#6442,.T.);
#12899=EDGE_CURVE('',#10493,#10491,#844,.T.);
#12900=EDGE_CURVE('',#10492,#10494,#845,.T.);
#12901=EDGE_CURVE('',#10495,#10496,#6443,.T.);
#12902=EDGE_CURVE('',#10495,#10493,#846,.T.);
#12903=EDGE_CURVE('',#10494,#10496,#847,.T.);
#12904=EDGE_CURVE('',#10497,#10498,#6444,.T.);
#12905=EDGE_CURVE('',#10497,#10495,#848,.T.);
#12906=EDGE_CURVE('',#10496,#10498,#849,.T.);
#12907=EDGE_CURVE('',#10499,#10500,#6445,.T.);
#12908=EDGE_CURVE('',#10499,#10497,#850,.T.);
#12909=EDGE_CURVE('',#10498,#10500,#851,.T.);
#12910=EDGE_CURVE('',#10501,#10502,#6446,.T.);
#12911=EDGE_CURVE('',#10501,#10499,#852,.T.);
#12912=EDGE_CURVE('',#10500,#10502,#853,.T.);
#12913=EDGE_CURVE('',#10503,#10504,#6447,.T.);
#12914=EDGE_CURVE('',#10503,#10501,#854,.T.);
#12915=EDGE_CURVE('',#10502,#10504,#855,.T.);
#12916=EDGE_CURVE('',#10505,#10506,#6448,.T.);
#12917=EDGE_CURVE('',#10505,#10503,#856,.T.);
#12918=EDGE_CURVE('',#10504,#10506,#857,.T.);
#12919=EDGE_CURVE('',#10507,#10508,#6449,.T.);
#12920=EDGE_CURVE('',#10507,#10505,#858,.T.);
#12921=EDGE_CURVE('',#10506,#10508,#859,.T.);
#12922=EDGE_CURVE('',#10509,#10510,#6450,.T.);
#12923=EDGE_CURVE('',#10509,#10507,#860,.T.);
#12924=EDGE_CURVE('',#10508,#10510,#861,.T.);
#12925=EDGE_CURVE('',#10511,#10512,#6451,.T.);
#12926=EDGE_CURVE('',#10511,#10509,#862,.T.);
#12927=EDGE_CURVE('',#10510,#10512,#863,.T.);
#12928=EDGE_CURVE('',#10513,#10514,#6452,.T.);
#12929=EDGE_CURVE('',#10513,#10511,#864,.T.);
#12930=EDGE_CURVE('',#10512,#10514,#865,.T.);
#12931=EDGE_CURVE('',#10515,#10516,#6453,.T.);
#12932=EDGE_CURVE('',#10515,#10513,#866,.T.);
#12933=EDGE_CURVE('',#10514,#10516,#867,.T.);
#12934=EDGE_CURVE('',#10517,#10518,#6454,.T.);
#12935=EDGE_CURVE('',#10517,#10515,#868,.T.);
#12936=EDGE_CURVE('',#10516,#10518,#869,.T.);
#12937=EDGE_CURVE('',#10519,#10520,#6455,.T.);
#12938=EDGE_CURVE('',#10519,#10517,#870,.T.);
#12939=EDGE_CURVE('',#10518,#10520,#871,.T.);
#12940=EDGE_CURVE('',#10521,#10522,#6456,.T.);
#12941=EDGE_CURVE('',#10521,#10519,#872,.T.);
#12942=EDGE_CURVE('',#10520,#10522,#873,.T.);
#12943=EDGE_CURVE('',#10523,#10524,#6457,.T.);
#12944=EDGE_CURVE('',#10523,#10521,#874,.T.);
#12945=EDGE_CURVE('',#10522,#10524,#875,.T.);
#12946=EDGE_CURVE('',#10525,#10526,#6458,.T.);
#12947=EDGE_CURVE('',#10525,#10523,#876,.T.);
#12948=EDGE_CURVE('',#10524,#10526,#877,.T.);
#12949=EDGE_CURVE('',#10527,#10528,#6459,.T.);
#12950=EDGE_CURVE('',#10527,#10525,#878,.T.);
#12951=EDGE_CURVE('',#10526,#10528,#879,.T.);
#12952=EDGE_CURVE('',#10529,#10530,#6460,.T.);
#12953=EDGE_CURVE('',#10529,#10527,#880,.T.);
#12954=EDGE_CURVE('',#10528,#10530,#881,.T.);
#12955=EDGE_CURVE('',#10531,#10532,#6461,.T.);
#12956=EDGE_CURVE('',#10531,#10529,#882,.T.);
#12957=EDGE_CURVE('',#10530,#10532,#883,.T.);
#12958=EDGE_CURVE('',#10533,#10534,#6462,.T.);
#12959=EDGE_CURVE('',#10533,#10531,#884,.T.);
#12960=EDGE_CURVE('',#10532,#10534,#885,.T.);
#12961=EDGE_CURVE('',#10535,#10536,#6463,.T.);
#12962=EDGE_CURVE('',#10535,#10533,#886,.T.);
#12963=EDGE_CURVE('',#10534,#10536,#887,.T.);
#12964=EDGE_CURVE('',#10537,#10538,#6464,.T.);
#12965=EDGE_CURVE('',#10537,#10535,#888,.T.);
#12966=EDGE_CURVE('',#10536,#10538,#889,.T.);
#12967=EDGE_CURVE('',#10539,#10540,#6465,.T.);
#12968=EDGE_CURVE('',#10539,#10537,#890,.T.);
#12969=EDGE_CURVE('',#10538,#10540,#891,.T.);
#12970=EDGE_CURVE('',#10541,#10542,#6466,.T.);
#12971=EDGE_CURVE('',#10541,#10539,#892,.T.);
#12972=EDGE_CURVE('',#10540,#10542,#893,.T.);
#12973=EDGE_CURVE('',#10543,#10544,#6467,.T.);
#12974=EDGE_CURVE('',#10543,#10545,#894,.T.);
#12975=EDGE_CURVE('',#10544,#10545,#9255,.T.);
#12976=EDGE_CURVE('',#10546,#10547,#6468,.T.);
#12977=EDGE_CURVE('',#10546,#10543,#895,.T.);
#12978=EDGE_CURVE('',#10548,#10544,#9256,.T.);
#12979=EDGE_CURVE('',#10547,#10548,#896,.T.);
#12980=EDGE_CURVE('',#10549,#10550,#6469,.T.);
#12981=EDGE_CURVE('',#10549,#10546,#897,.T.);
#12982=EDGE_CURVE('',#10550,#10547,#898,.T.);
#12983=EDGE_CURVE('',#10551,#10552,#6470,.T.);
#12984=EDGE_CURVE('',#10551,#10549,#899,.T.);
#12985=EDGE_CURVE('',#10552,#10550,#900,.T.);
#12986=EDGE_CURVE('',#10553,#10554,#6471,.T.);
#12987=EDGE_CURVE('',#10553,#10551,#901,.T.);
#12988=EDGE_CURVE('',#10554,#10552,#902,.T.);
#12989=EDGE_CURVE('',#10555,#10556,#6472,.T.);
#12990=EDGE_CURVE('',#10555,#10553,#903,.T.);
#12991=EDGE_CURVE('',#10556,#10554,#904,.T.);
#12992=EDGE_CURVE('',#10557,#10558,#6473,.T.);
#12993=EDGE_CURVE('',#10557,#10555,#905,.T.);
#12994=EDGE_CURVE('',#10558,#10556,#906,.T.);
#12995=EDGE_CURVE('',#10559,#10560,#6474,.T.);
#12996=EDGE_CURVE('',#10559,#10557,#907,.T.);
#12997=EDGE_CURVE('',#10560,#10558,#908,.T.);
#12998=EDGE_CURVE('',#10561,#10562,#6475,.T.);
#12999=EDGE_CURVE('',#10561,#10559,#909,.T.);
#13000=EDGE_CURVE('',#10562,#10560,#910,.T.);
#13001=EDGE_CURVE('',#10563,#10564,#6476,.T.);
#13002=EDGE_CURVE('',#10563,#10561,#911,.T.);
#13003=EDGE_CURVE('',#10564,#10562,#912,.T.);
#13004=EDGE_CURVE('',#10565,#10566,#6477,.T.);
#13005=EDGE_CURVE('',#10565,#10563,#913,.T.);
#13006=EDGE_CURVE('',#10566,#10564,#914,.T.);
#13007=EDGE_CURVE('',#10567,#10568,#6478,.T.);
#13008=EDGE_CURVE('',#10567,#10565,#915,.T.);
#13009=EDGE_CURVE('',#10568,#10566,#916,.T.);
#13010=EDGE_CURVE('',#10569,#10570,#6479,.T.);
#13011=EDGE_CURVE('',#10569,#10567,#917,.T.);
#13012=EDGE_CURVE('',#10570,#10568,#918,.T.);
#13013=EDGE_CURVE('',#10571,#10572,#6480,.T.);
#13014=EDGE_CURVE('',#10571,#10569,#919,.T.);
#13015=EDGE_CURVE('',#10572,#10570,#920,.T.);
#13016=EDGE_CURVE('',#10573,#10574,#6481,.T.);
#13017=EDGE_CURVE('',#10573,#10571,#921,.T.);
#13018=EDGE_CURVE('',#10574,#10572,#922,.T.);
#13019=EDGE_CURVE('',#10575,#10576,#6482,.T.);
#13020=EDGE_CURVE('',#10575,#10573,#923,.T.);
#13021=EDGE_CURVE('',#10576,#10574,#924,.T.);
#13022=EDGE_CURVE('',#10577,#10578,#6483,.T.);
#13023=EDGE_CURVE('',#10577,#10575,#925,.T.);
#13024=EDGE_CURVE('',#10578,#10576,#926,.T.);
#13025=EDGE_CURVE('',#10579,#10580,#6484,.T.);
#13026=EDGE_CURVE('',#10579,#10577,#927,.T.);
#13027=EDGE_CURVE('',#10580,#10578,#928,.T.);
#13028=EDGE_CURVE('',#10581,#10582,#6485,.T.);
#13029=EDGE_CURVE('',#10581,#10579,#929,.T.);
#13030=EDGE_CURVE('',#10582,#10580,#930,.T.);
#13031=EDGE_CURVE('',#10583,#10584,#6486,.T.);
#13032=EDGE_CURVE('',#10583,#10581,#931,.T.);
#13033=EDGE_CURVE('',#10584,#10582,#932,.T.);
#13034=EDGE_CURVE('',#10585,#10586,#6487,.T.);
#13035=EDGE_CURVE('',#10585,#10583,#933,.T.);
#13036=EDGE_CURVE('',#10586,#10584,#934,.T.);
#13037=EDGE_CURVE('',#10587,#10588,#6488,.T.);
#13038=EDGE_CURVE('',#10587,#10585,#935,.T.);
#13039=EDGE_CURVE('',#10588,#10586,#936,.T.);
#13040=EDGE_CURVE('',#10589,#10590,#6489,.T.);
#13041=EDGE_CURVE('',#10589,#10587,#937,.T.);
#13042=EDGE_CURVE('',#10590,#10588,#938,.T.);
#13043=EDGE_CURVE('',#10591,#10592,#6490,.T.);
#13044=EDGE_CURVE('',#10591,#10589,#939,.T.);
#13045=EDGE_CURVE('',#10592,#10590,#940,.T.);
#13046=EDGE_CURVE('',#10593,#10594,#6491,.T.);
#13047=EDGE_CURVE('',#10593,#10591,#941,.T.);
#13048=EDGE_CURVE('',#10594,#10592,#942,.T.);
#13049=EDGE_CURVE('',#10595,#10596,#6492,.T.);
#13050=EDGE_CURVE('',#10595,#10593,#943,.T.);
#13051=EDGE_CURVE('',#10596,#10594,#944,.T.);
#13052=EDGE_CURVE('',#10597,#10598,#6493,.T.);
#13053=EDGE_CURVE('',#10597,#10595,#945,.T.);
#13054=EDGE_CURVE('',#10598,#10596,#946,.T.);
#13055=EDGE_CURVE('',#10599,#10600,#6494,.T.);
#13056=EDGE_CURVE('',#10599,#10597,#947,.T.);
#13057=EDGE_CURVE('',#10600,#10598,#948,.T.);
#13058=EDGE_CURVE('',#10601,#10602,#6495,.T.);
#13059=EDGE_CURVE('',#10601,#10599,#949,.T.);
#13060=EDGE_CURVE('',#10602,#10600,#950,.T.);
#13061=EDGE_CURVE('',#10603,#10604,#6496,.T.);
#13062=EDGE_CURVE('',#10603,#10601,#951,.T.);
#13063=EDGE_CURVE('',#10604,#10602,#952,.T.);
#13064=EDGE_CURVE('',#10605,#10606,#6497,.T.);
#13065=EDGE_CURVE('',#10605,#10603,#953,.T.);
#13066=EDGE_CURVE('',#10606,#10604,#954,.T.);
#13067=EDGE_CURVE('',#10607,#10608,#6498,.T.);
#13068=EDGE_CURVE('',#10607,#10605,#955,.T.);
#13069=EDGE_CURVE('',#10608,#10606,#956,.T.);
#13070=EDGE_CURVE('',#10609,#10610,#6499,.T.);
#13071=EDGE_CURVE('',#10609,#10607,#957,.T.);
#13072=EDGE_CURVE('',#10610,#10608,#958,.T.);
#13073=EDGE_CURVE('',#10611,#10612,#6500,.T.);
#13074=EDGE_CURVE('',#10611,#10609,#959,.T.);
#13075=EDGE_CURVE('',#10612,#10610,#960,.T.);
#13076=EDGE_CURVE('',#10613,#10614,#6501,.T.);
#13077=EDGE_CURVE('',#10613,#10611,#961,.T.);
#13078=EDGE_CURVE('',#10614,#10612,#962,.T.);
#13079=EDGE_CURVE('',#10615,#10616,#6502,.T.);
#13080=EDGE_CURVE('',#10615,#10613,#963,.T.);
#13081=EDGE_CURVE('',#10616,#10614,#964,.T.);
#13082=EDGE_CURVE('',#10617,#10618,#6503,.T.);
#13083=EDGE_CURVE('',#10617,#10615,#965,.T.);
#13084=EDGE_CURVE('',#10618,#10616,#966,.T.);
#13085=EDGE_CURVE('',#10619,#10620,#6504,.T.);
#13086=EDGE_CURVE('',#10619,#10617,#967,.T.);
#13087=EDGE_CURVE('',#10620,#10618,#968,.T.);
#13088=EDGE_CURVE('',#10621,#10622,#6505,.T.);
#13089=EDGE_CURVE('',#10621,#10619,#969,.T.);
#13090=EDGE_CURVE('',#10622,#10620,#970,.T.);
#13091=EDGE_CURVE('',#10623,#10624,#6506,.T.);
#13092=EDGE_CURVE('',#10623,#10621,#971,.T.);
#13093=EDGE_CURVE('',#10624,#10622,#972,.T.);
#13094=EDGE_CURVE('',#10625,#10626,#6507,.T.);
#13095=EDGE_CURVE('',#10625,#10623,#973,.T.);
#13096=EDGE_CURVE('',#10626,#10624,#974,.T.);
#13097=EDGE_CURVE('',#10627,#10628,#6508,.T.);
#13098=EDGE_CURVE('',#10627,#10625,#975,.T.);
#13099=EDGE_CURVE('',#10628,#10626,#976,.T.);
#13100=EDGE_CURVE('',#10629,#10630,#6509,.T.);
#13101=EDGE_CURVE('',#10629,#10627,#977,.T.);
#13102=EDGE_CURVE('',#10630,#10628,#978,.T.);
#13103=EDGE_CURVE('',#10631,#10632,#6510,.T.);
#13104=EDGE_CURVE('',#10631,#10629,#979,.T.);
#13105=EDGE_CURVE('',#10632,#10630,#980,.T.);
#13106=EDGE_CURVE('',#10633,#10634,#6511,.T.);
#13107=EDGE_CURVE('',#10633,#10631,#981,.T.);
#13108=EDGE_CURVE('',#10634,#10632,#982,.T.);
#13109=EDGE_CURVE('',#10635,#10636,#6512,.T.);
#13110=EDGE_CURVE('',#10635,#10633,#983,.T.);
#13111=EDGE_CURVE('',#10636,#10634,#984,.T.);
#13112=EDGE_CURVE('',#10637,#10638,#6513,.T.);
#13113=EDGE_CURVE('',#10637,#10635,#985,.T.);
#13114=EDGE_CURVE('',#10638,#10636,#986,.T.);
#13115=EDGE_CURVE('',#10639,#10640,#6514,.T.);
#13116=EDGE_CURVE('',#10639,#10637,#987,.T.);
#13117=EDGE_CURVE('',#10640,#10638,#988,.T.);
#13118=EDGE_CURVE('',#10641,#10642,#6515,.T.);
#13119=EDGE_CURVE('',#10641,#10639,#989,.T.);
#13120=EDGE_CURVE('',#10642,#10640,#990,.T.);
#13121=EDGE_CURVE('',#10643,#10644,#6516,.T.);
#13122=EDGE_CURVE('',#10643,#10641,#991,.T.);
#13123=EDGE_CURVE('',#10644,#10642,#992,.T.);
#13124=EDGE_CURVE('',#10645,#10646,#6517,.T.);
#13125=EDGE_CURVE('',#10645,#10643,#993,.T.);
#13126=EDGE_CURVE('',#10646,#10644,#994,.T.);
#13127=EDGE_CURVE('',#10647,#10648,#6518,.T.);
#13128=EDGE_CURVE('',#10647,#10645,#995,.T.);
#13129=EDGE_CURVE('',#10648,#10646,#996,.T.);
#13130=EDGE_CURVE('',#10649,#10650,#6519,.T.);
#13131=EDGE_CURVE('',#10649,#10647,#997,.T.);
#13132=EDGE_CURVE('',#10650,#10648,#998,.T.);
#13133=EDGE_CURVE('',#10651,#10652,#6520,.T.);
#13134=EDGE_CURVE('',#10651,#10649,#999,.T.);
#13135=EDGE_CURVE('',#10652,#10650,#1000,.T.);
#13136=EDGE_CURVE('',#10653,#10654,#6521,.T.);
#13137=EDGE_CURVE('',#10653,#10651,#1001,.T.);
#13138=EDGE_CURVE('',#10654,#10652,#1002,.T.);
#13139=EDGE_CURVE('',#10655,#10656,#6522,.T.);
#13140=EDGE_CURVE('',#10655,#10653,#1003,.T.);
#13141=EDGE_CURVE('',#10656,#10654,#1004,.T.);
#13142=EDGE_CURVE('',#10657,#10658,#6523,.T.);
#13143=EDGE_CURVE('',#10657,#10655,#1005,.T.);
#13144=EDGE_CURVE('',#10658,#10656,#1006,.T.);
#13145=EDGE_CURVE('',#10659,#10660,#6524,.T.);
#13146=EDGE_CURVE('',#10659,#10657,#1007,.T.);
#13147=EDGE_CURVE('',#10660,#10658,#1008,.T.);
#13148=EDGE_CURVE('',#10661,#10662,#6525,.T.);
#13149=EDGE_CURVE('',#10661,#10659,#1009,.T.);
#13150=EDGE_CURVE('',#10662,#10660,#1010,.T.);
#13151=EDGE_CURVE('',#10663,#10664,#6526,.T.);
#13152=EDGE_CURVE('',#10663,#10661,#1011,.T.);
#13153=EDGE_CURVE('',#10664,#10662,#1012,.T.);
#13154=EDGE_CURVE('',#10665,#10666,#6527,.T.);
#13155=EDGE_CURVE('',#10665,#10663,#1013,.T.);
#13156=EDGE_CURVE('',#10666,#10664,#1014,.T.);
#13157=EDGE_CURVE('',#10667,#10668,#6528,.T.);
#13158=EDGE_CURVE('',#10667,#10665,#1015,.T.);
#13159=EDGE_CURVE('',#10668,#10666,#1016,.T.);
#13160=EDGE_CURVE('',#10669,#10670,#6529,.T.);
#13161=EDGE_CURVE('',#10669,#10667,#1017,.T.);
#13162=EDGE_CURVE('',#10670,#10668,#1018,.T.);
#13163=EDGE_CURVE('',#10671,#10671,#9257,.T.);
#13164=EDGE_CURVE('',#10672,#10418,#1019,.T.);
#13165=EDGE_CURVE('',#10417,#10673,#1020,.T.);
#13166=EDGE_CURVE('',#10673,#10672,#9258,.T.);
#13167=EDGE_CURVE('',#10671,#10674,#6530,.T.);
#13168=EDGE_CURVE('',#10674,#10674,#9259,.T.);
#13169=EDGE_CURVE('',#10675,#10548,#1021,.T.);
#13170=EDGE_CURVE('',#10542,#10675,#1022,.T.);
#13171=EDGE_CURVE('',#10672,#10670,#1023,.T.);
#13172=EDGE_CURVE('',#10673,#10669,#1024,.T.);
#13173=EDGE_CURVE('',#10545,#10676,#1025,.T.);
#13174=EDGE_CURVE('',#10676,#10541,#1026,.T.);
#13175=EDGE_CURVE('',#10677,#10678,#6531,.T.);
#13176=EDGE_CURVE('',#10677,#10679,#6532,.T.);
#13177=EDGE_CURVE('',#10680,#10679,#6533,.T.);
#13178=EDGE_CURVE('',#10678,#10680,#6534,.T.);
#13179=EDGE_CURVE('',#10678,#10681,#9260,.T.);
#13180=EDGE_CURVE('',#10680,#10682,#6535,.T.);
#13181=EDGE_CURVE('',#10682,#10681,#6536,.T.);
#13182=EDGE_CURVE('',#10679,#10683,#6537,.T.);
#13183=EDGE_CURVE('',#10682,#10683,#6538,.T.);
#13184=EDGE_CURVE('',#10681,#10684,#6539,.T.);
#13185=EDGE_CURVE('',#10683,#10684,#6540,.T.);
#13186=EDGE_CURVE('',#10684,#10677,#9261,.T.);
#13187=EDGE_CURVE('',#10685,#10685,#9262,.T.);
#13188=EDGE_CURVE('',#10685,#10686,#6541,.T.);
#13189=EDGE_CURVE('',#10686,#10686,#9263,.T.);
#13190=EDGE_CURVE('',#10687,#10687,#9264,.T.);
#13191=EDGE_CURVE('',#10676,#10675,#9265,.F.);
#13192=EDGE_CURVE('',#10688,#10688,#9266,.T.);
#13193=EDGE_CURVE('',#10688,#10687,#6542,.T.);
#13194=EDGE_CURVE('',#10689,#10689,#9267,.T.);
#13195=EDGE_CURVE('',#10689,#10690,#6543,.T.);
#13196=EDGE_CURVE('',#10690,#10690,#9268,.T.);
#13197=EDGE_CURVE('',#10691,#10691,#9269,.T.);
#13198=EDGE_CURVE('',#10691,#10692,#6544,.T.);
#13199=EDGE_CURVE('',#10692,#10692,#9270,.T.);
#13200=EDGE_CURVE('',#10693,#10694,#6545,.T.);
#13201=EDGE_CURVE('',#10693,#10694,#9271,.T.);
#13202=EDGE_CURVE('',#10695,#10696,#1027,.T.);
#13203=EDGE_CURVE('',#10697,#10695,#9272,.T.);
#13204=EDGE_CURVE('',#10694,#10697,#1028,.T.);
#13205=EDGE_CURVE('',#10696,#10693,#1029,.T.);
#13206=EDGE_CURVE('',#10696,#10698,#6546,.T.);
#13207=EDGE_CURVE('',#10699,#10698,#1030,.T.);
#13208=EDGE_CURVE('',#10698,#10699,#1031,.T.);
#13209=EDGE_CURVE('',#10697,#10695,#6547,.T.);
#13210=EDGE_CURVE('',#10700,#10700,#9273,.T.);
#13211=EDGE_CURVE('',#10700,#10701,#6548,.T.);
#13212=EDGE_CURVE('',#10701,#10701,#9274,.T.);
#13213=EDGE_CURVE('',#10702,#10702,#9275,.T.);
#13214=EDGE_CURVE('',#10702,#10703,#6549,.T.);
#13215=EDGE_CURVE('',#10703,#10703,#9276,.T.);
#13216=EDGE_CURVE('',#10704,#10704,#9277,.T.);
#13217=EDGE_CURVE('',#10704,#10705,#6550,.T.);
#13218=EDGE_CURVE('',#10705,#10705,#9278,.T.);
#13219=EDGE_CURVE('',#10706,#10707,#6551,.T.);
#13220=EDGE_CURVE('',#10706,#10707,#9279,.T.);
#13221=EDGE_CURVE('',#10708,#10709,#1032,.T.);
#13222=EDGE_CURVE('',#10710,#10708,#9280,.T.);
#13223=EDGE_CURVE('',#10707,#10710,#1033,.T.);
#13224=EDGE_CURVE('',#10709,#10706,#1034,.T.);
#13225=EDGE_CURVE('',#10709,#10711,#6552,.T.);
#13226=EDGE_CURVE('',#10712,#10711,#1035,.T.);
#13227=EDGE_CURVE('',#10711,#10712,#1036,.T.);
#13228=EDGE_CURVE('',#10710,#10708,#6553,.T.);
#13229=EDGE_CURVE('',#10713,#10714,#6554,.T.);
#13230=EDGE_CURVE('',#10715,#10713,#6555,.T.);
#13231=EDGE_CURVE('',#10716,#10715,#6556,.T.);
#13232=EDGE_CURVE('',#10717,#10716,#6557,.T.);
#13233=EDGE_CURVE('',#10718,#10717,#6558,.T.);
#13234=EDGE_CURVE('',#10714,#10718,#6559,.T.);
#13235=EDGE_CURVE('',#10719,#10713,#6560,.T.);
#13236=EDGE_CURVE('',#10720,#10719,#6561,.T.);
#13237=EDGE_CURVE('',#10715,#10720,#6562,.T.);
#13238=EDGE_CURVE('',#10721,#10719,#6563,.T.);
#13239=EDGE_CURVE('',#10722,#10721,#6564,.T.);
#13240=EDGE_CURVE('',#10723,#10722,#6565,.T.);
#13241=EDGE_CURVE('',#10724,#10723,#6566,.T.);
#13242=EDGE_CURVE('',#10720,#10724,#6567,.T.);
#13243=EDGE_CURVE('',#10725,#10725,#9281,.T.);
#13244=EDGE_CURVE('',#10714,#10721,#9282,.T.);
#13245=EDGE_CURVE('',#10726,#10726,#9283,.T.);
#13246=EDGE_CURVE('',#10724,#10716,#9284,.T.);
#13247=EDGE_CURVE('',#10725,#10726,#6568,.T.);
#13248=EDGE_CURVE('',#10718,#10722,#9285,.T.);
#13249=EDGE_CURVE('',#10723,#10717,#9286,.T.);
#13250=EDGE_CURVE('',#10727,#10727,#9287,.T.);
#13251=EDGE_CURVE('',#10727,#10728,#6569,.T.);
#13252=EDGE_CURVE('',#10728,#10728,#9288,.T.);
#13253=EDGE_CURVE('',#10729,#10729,#9289,.T.);
#13254=EDGE_CURVE('',#10729,#10730,#6570,.T.);
#13255=EDGE_CURVE('',#10730,#10730,#9290,.T.);
#13256=EDGE_CURVE('',#10731,#10731,#9291,.T.);
#13257=EDGE_CURVE('',#10731,#10732,#6571,.T.);
#13258=EDGE_CURVE('',#10732,#10732,#9292,.T.);
#13259=EDGE_CURVE('',#10733,#10733,#9293,.T.);
#13260=EDGE_CURVE('',#10733,#10734,#6572,.T.);
#13261=EDGE_CURVE('',#10734,#10734,#9294,.T.);
#13262=EDGE_CURVE('',#10735,#10736,#6573,.T.);
#13263=EDGE_CURVE('',#10737,#10735,#6574,.T.);
#13264=EDGE_CURVE('',#10738,#10737,#6575,.T.);
#13265=EDGE_CURVE('',#10739,#10738,#6576,.T.);
#13266=EDGE_CURVE('',#10740,#10739,#6577,.T.);
#13267=EDGE_CURVE('',#10741,#10740,#6578,.T.);
#13268=EDGE_CURVE('',#10742,#10741,#6579,.T.);
#13269=EDGE_CURVE('',#10736,#10742,#6580,.T.);
#13270=EDGE_CURVE('',#10739,#10743,#6581,.T.);
#13271=EDGE_CURVE('',#10743,#10744,#6582,.T.);
#13272=EDGE_CURVE('',#10744,#10740,#6583,.T.);
#13273=EDGE_CURVE('',#10745,#10738,#6584,.T.);
#13274=EDGE_CURVE('',#10745,#10743,#6585,.T.);
#13275=EDGE_CURVE('',#10737,#10746,#6586,.T.);
#13276=EDGE_CURVE('',#10746,#10745,#6587,.T.);
#13277=EDGE_CURVE('',#10747,#10735,#6588,.T.);
#13278=EDGE_CURVE('',#10747,#10746,#6589,.T.);
#13279=EDGE_CURVE('',#10748,#10749,#6590,.T.);
#13280=EDGE_CURVE('',#10744,#10748,#6591,.T.);
#13281=EDGE_CURVE('',#10750,#10747,#6592,.T.);
#13282=EDGE_CURVE('',#10749,#10750,#6593,.T.);
#13283=EDGE_CURVE('',#10741,#10748,#6594,.T.);
#13284=EDGE_CURVE('',#10736,#10750,#6595,.T.);
#13285=EDGE_CURVE('',#10749,#10742,#6596,.T.);
#13286=EDGE_CURVE('',#10751,#10752,#6597,.T.);
#13287=EDGE_CURVE('',#10751,#10753,#6598,.T.);
#13288=EDGE_CURVE('',#10753,#10754,#6599,.T.);
#13289=EDGE_CURVE('',#10752,#10754,#6600,.T.);
#13290=EDGE_CURVE('',#10755,#10751,#6601,.T.);
#13291=EDGE_CURVE('',#10755,#10756,#6602,.T.);
#13292=EDGE_CURVE('',#10756,#10753,#6603,.T.);
#13293=EDGE_CURVE('',#10757,#10755,#6604,.T.);
#13294=EDGE_CURVE('',#10757,#10758,#6605,.T.);
#13295=EDGE_CURVE('',#10758,#10756,#6606,.T.);
#13296=EDGE_CURVE('',#10759,#10757,#6607,.T.);
#13297=EDGE_CURVE('',#10759,#10760,#6608,.T.);
#13298=EDGE_CURVE('',#10760,#10758,#6609,.T.);
#13299=EDGE_CURVE('',#10761,#10759,#6610,.T.);
#13300=EDGE_CURVE('',#10761,#10762,#6611,.T.);
#13301=EDGE_CURVE('',#10762,#10760,#6612,.T.);
#13302=EDGE_CURVE('',#10752,#10761,#6613,.T.);
#13303=EDGE_CURVE('',#10754,#10762,#6614,.T.);
#13304=EDGE_CURVE('',#10763,#10763,#9295,.T.);
#13305=EDGE_CURVE('',#10764,#10764,#9296,.T.);
#13306=EDGE_CURVE('',#10764,#10763,#6615,.T.);
#13307=EDGE_CURVE('',#10765,#10765,#9297,.F.);
#13308=EDGE_CURVE('',#10765,#10764,#6616,.T.);
#13309=EDGE_CURVE('',#10766,#10766,#9298,.T.);
#13310=EDGE_CURVE('',#10766,#10765,#6617,.T.);
#13311=EDGE_CURVE('',#10767,#10767,#9299,.T.);
#13312=EDGE_CURVE('',#10767,#10768,#6618,.T.);
#13313=EDGE_CURVE('',#10768,#10768,#9300,.T.);
#13314=EDGE_CURVE('',#10769,#10769,#9301,.T.);
#13315=EDGE_CURVE('',#10769,#10770,#6619,.T.);
#13316=EDGE_CURVE('',#10770,#10770,#9302,.T.);
#13317=EDGE_CURVE('',#10771,#10771,#9303,.T.);
#13318=EDGE_CURVE('',#10772,#10772,#9304,.T.);
#13319=EDGE_CURVE('',#10772,#10771,#6620,.T.);
#13320=EDGE_CURVE('',#10773,#10773,#9305,.T.);
#13321=EDGE_CURVE('',#10773,#10772,#6621,.T.);
#13322=EDGE_CURVE('',#10774,#10774,#9306,.T.);
#13323=EDGE_CURVE('',#10774,#10773,#6622,.T.);
#13324=EDGE_CURVE('',#10775,#10775,#9307,.T.);
#13325=EDGE_CURVE('',#10776,#10776,#9308,.F.);
#13326=EDGE_CURVE('',#10776,#10775,#6623,.T.);
#13327=EDGE_CURVE('',#10777,#10777,#9309,.F.);
#13328=EDGE_CURVE('',#10777,#10776,#6624,.T.);
#13329=EDGE_CURVE('',#10778,#10778,#9310,.T.);
#13330=EDGE_CURVE('',#10778,#10777,#6625,.T.);
#13331=EDGE_CURVE('',#10779,#10780,#6626,.T.);
#13332=EDGE_CURVE('',#10780,#10781,#6627,.T.);
#13333=EDGE_CURVE('',#10781,#10782,#6628,.T.);
#13334=EDGE_CURVE('',#10779,#10782,#6629,.T.);
#13335=EDGE_CURVE('',#10780,#10783,#6630,.T.);
#13336=EDGE_CURVE('',#10783,#10784,#6631,.T.);
#13337=EDGE_CURVE('',#10784,#10781,#6632,.T.);
#13338=EDGE_CURVE('',#10783,#10785,#6633,.T.);
#13339=EDGE_CURVE('',#10785,#10786,#6634,.T.);
#13340=EDGE_CURVE('',#10786,#10784,#6635,.T.);
#13341=EDGE_CURVE('',#10785,#10787,#6636,.T.);
#13342=EDGE_CURVE('',#10787,#10788,#6637,.T.);
#13343=EDGE_CURVE('',#10788,#10786,#6638,.T.);
#13344=EDGE_CURVE('',#10787,#10789,#6639,.T.);
#13345=EDGE_CURVE('',#10789,#10790,#6640,.T.);
#13346=EDGE_CURVE('',#10790,#10788,#6641,.T.);
#13347=EDGE_CURVE('',#10789,#10779,#6642,.T.);
#13348=EDGE_CURVE('',#10782,#10790,#6643,.T.);
#13349=EDGE_CURVE('',#10791,#10791,#9311,.T.);
#13350=EDGE_CURVE('',#10791,#10792,#6644,.T.);
#13351=EDGE_CURVE('',#10792,#10792,#9312,.T.);
#13352=EDGE_CURVE('',#10793,#10793,#9313,.T.);
#13353=EDGE_CURVE('',#10793,#10794,#6645,.T.);
#13354=EDGE_CURVE('',#10794,#10794,#9314,.T.);
#13355=EDGE_CURVE('',#10795,#10795,#9315,.T.);
#13356=EDGE_CURVE('',#10795,#10796,#6646,.T.);
#13357=EDGE_CURVE('',#10796,#10796,#9316,.T.);
#13358=EDGE_CURVE('',#10797,#10797,#9317,.T.);
#13359=EDGE_CURVE('',#10797,#10798,#6647,.T.);
#13360=EDGE_CURVE('',#10798,#10798,#9318,.T.);
#13361=EDGE_CURVE('',#10799,#10799,#9319,.T.);
#13362=EDGE_CURVE('',#10799,#10800,#6648,.T.);
#13363=EDGE_CURVE('',#10800,#10800,#9320,.T.);
#13364=EDGE_CURVE('',#10801,#10801,#9321,.T.);
#13365=EDGE_CURVE('',#10801,#10802,#6649,.T.);
#13366=EDGE_CURVE('',#10802,#10802,#9322,.T.);
#13367=EDGE_CURVE('',#10803,#10803,#9323,.T.);
#13368=EDGE_CURVE('',#10803,#10804,#6650,.T.);
#13369=EDGE_CURVE('',#10804,#10804,#9324,.T.);
#13370=EDGE_CURVE('',#10805,#10805,#9325,.T.);
#13371=EDGE_CURVE('',#10805,#10806,#6651,.T.);
#13372=EDGE_CURVE('',#10806,#10806,#9326,.T.);
#13373=EDGE_CURVE('',#10807,#10807,#9327,.T.);
#13374=EDGE_CURVE('',#10807,#10808,#6652,.T.);
#13375=EDGE_CURVE('',#10808,#10808,#9328,.T.);
#13376=EDGE_CURVE('',#10809,#10809,#9329,.T.);
#13377=EDGE_CURVE('',#10810,#10810,#9330,.T.);
#13378=EDGE_CURVE('',#10810,#10811,#6653,.T.);
#13379=EDGE_CURVE('',#10811,#10811,#9331,.T.);
#13380=EDGE_CURVE('',#10812,#10812,#9332,.T.);
#13381=EDGE_CURVE('',#10813,#10813,#9333,.T.);
#13382=EDGE_CURVE('',#10813,#10814,#6654,.T.);
#13383=EDGE_CURVE('',#10814,#10814,#9334,.T.);
#13384=EDGE_CURVE('',#10815,#10815,#9335,.T.);
#13385=EDGE_CURVE('',#10816,#10816,#9336,.T.);
#13386=EDGE_CURVE('',#10816,#10817,#6655,.T.);
#13387=EDGE_CURVE('',#10817,#10817,#9337,.T.);
#13388=EDGE_CURVE('',#10818,#10818,#9338,.T.);
#13389=EDGE_CURVE('',#10819,#10819,#9339,.T.);
#13390=EDGE_CURVE('',#10819,#10809,#6656,.T.);
#13391=EDGE_CURVE('',#10820,#10820,#9340,.T.);
#13392=EDGE_CURVE('',#10820,#10812,#6657,.T.);
#13393=EDGE_CURVE('',#10821,#10821,#9341,.T.);
#13394=EDGE_CURVE('',#10821,#10815,#6658,.T.);
#13395=EDGE_CURVE('',#10822,#10822,#9342,.T.);
#13396=EDGE_CURVE('',#10822,#10818,#6659,.T.);
#13397=EDGE_CURVE('',#10823,#10823,#9343,.T.);
#13398=EDGE_CURVE('',#10823,#10824,#6660,.T.);
#13399=EDGE_CURVE('',#10824,#10824,#9344,.T.);
#13400=EDGE_CURVE('',#10825,#10825,#9345,.T.);
#13401=EDGE_CURVE('',#10825,#10826,#6661,.T.);
#13402=EDGE_CURVE('',#10826,#10826,#9346,.T.);
#13403=EDGE_CURVE('',#10827,#10827,#9347,.T.);
#13404=EDGE_CURVE('',#10827,#10828,#6662,.T.);
#13405=EDGE_CURVE('',#10828,#10828,#9348,.T.);
#13406=EDGE_CURVE('',#10829,#10829,#9349,.T.);
#13407=EDGE_CURVE('',#10829,#10830,#6663,.T.);
#13408=EDGE_CURVE('',#10830,#10830,#9350,.T.);
#13409=EDGE_CURVE('',#10831,#10831,#9351,.T.);
#13410=EDGE_CURVE('',#10831,#10832,#6664,.T.);
#13411=EDGE_CURVE('',#10832,#10832,#9352,.T.);
#13412=EDGE_CURVE('',#10833,#10833,#9353,.T.);
#13413=EDGE_CURVE('',#10833,#10834,#6665,.T.);
#13414=EDGE_CURVE('',#10834,#10834,#9354,.T.);
#13415=EDGE_CURVE('',#10835,#10835,#9355,.T.);
#13416=EDGE_CURVE('',#10835,#10836,#6666,.T.);
#13417=EDGE_CURVE('',#10836,#10836,#9356,.T.);
#13418=EDGE_CURVE('',#10837,#10837,#9357,.T.);
#13419=EDGE_CURVE('',#10837,#10838,#6667,.T.);
#13420=EDGE_CURVE('',#10838,#10838,#9358,.T.);
#13421=EDGE_CURVE('',#10839,#10839,#9359,.T.);
#13422=EDGE_CURVE('',#10839,#10840,#6668,.T.);
#13423=EDGE_CURVE('',#10840,#10840,#9360,.T.);
#13424=EDGE_CURVE('',#10841,#10841,#9361,.T.);
#13425=EDGE_CURVE('',#10841,#10842,#6669,.T.);
#13426=EDGE_CURVE('',#10842,#10842,#9362,.T.);
#13427=EDGE_CURVE('',#10843,#10844,#6670,.T.);
#13428=EDGE_CURVE('',#10844,#10845,#6671,.T.);
#13429=EDGE_CURVE('',#10846,#10845,#6672,.T.);
#13430=EDGE_CURVE('',#10843,#10846,#6673,.T.);
#13431=EDGE_CURVE('',#10847,#10843,#6674,.T.);
#13432=EDGE_CURVE('',#10848,#10846,#6675,.T.);
#13433=EDGE_CURVE('',#10847,#10848,#6676,.T.);
#13434=EDGE_CURVE('',#10849,#10847,#6677,.T.);
#13435=EDGE_CURVE('',#10850,#10848,#6678,.T.);
#13436=EDGE_CURVE('',#10849,#10850,#6679,.T.);
#13437=EDGE_CURVE('',#10844,#10849,#6680,.T.);
#13438=EDGE_CURVE('',#10845,#10850,#6681,.T.);
#13439=EDGE_CURVE('',#10851,#10852,#6682,.T.);
#13440=EDGE_CURVE('',#10853,#10851,#9363,.T.);
#13441=EDGE_CURVE('',#10853,#10854,#6683,.T.);
#13442=EDGE_CURVE('',#10852,#10854,#9364,.T.);
#13443=EDGE_CURVE('',#10855,#10856,#6684,.T.);
#13444=EDGE_CURVE('',#10857,#10855,#9365,.T.);
#13445=EDGE_CURVE('',#10857,#10858,#6685,.T.);
#13446=EDGE_CURVE('',#10856,#10858,#9366,.T.);
#13447=EDGE_CURVE('',#10859,#10859,#9367,.T.);
#13448=EDGE_CURVE('',#10859,#10860,#6686,.T.);
#13449=EDGE_CURVE('',#10860,#10860,#9368,.T.);
#13450=EDGE_CURVE('',#10861,#10861,#9369,.T.);
#13451=EDGE_CURVE('',#10861,#10862,#6687,.T.);
#13452=EDGE_CURVE('',#10862,#10862,#9370,.T.);
#13453=EDGE_CURVE('',#10863,#10863,#9371,.T.);
#13454=EDGE_CURVE('',#10863,#10864,#6688,.T.);
#13455=EDGE_CURVE('',#10864,#10864,#9372,.T.);
#13456=EDGE_CURVE('',#10865,#10865,#9373,.T.);
#13457=EDGE_CURVE('',#10865,#10866,#6689,.T.);
#13458=EDGE_CURVE('',#10866,#10866,#9374,.T.);
#13459=EDGE_CURVE('',#10867,#10867,#9375,.T.);
#13460=EDGE_CURVE('',#10867,#10868,#6690,.T.);
#13461=EDGE_CURVE('',#10868,#10868,#9376,.T.);
#13462=EDGE_CURVE('',#10869,#10869,#9377,.T.);
#13463=EDGE_CURVE('',#10858,#10856,#9378,.T.);
#13464=EDGE_CURVE('',#10857,#10858,#6691,.T.);
#13465=EDGE_CURVE('',#10855,#10857,#9379,.T.);
#13466=EDGE_CURVE('',#10870,#10870,#9380,.T.);
#13467=EDGE_CURVE('',#10871,#10871,#9381,.T.);
#13468=EDGE_CURVE('',#10871,#10872,#6692,.T.);
#13469=EDGE_CURVE('',#10872,#10872,#9382,.T.);
#13470=EDGE_CURVE('',#10873,#10873,#9383,.T.);
#13471=EDGE_CURVE('',#10854,#10852,#9384,.T.);
#13472=EDGE_CURVE('',#10853,#10854,#6693,.T.);
#13473=EDGE_CURVE('',#10851,#10853,#9385,.T.);
#13474=EDGE_CURVE('',#10874,#10874,#9386,.T.);
#13475=EDGE_CURVE('',#10875,#10876,#6694,.T.);
#13476=EDGE_CURVE('',#10876,#10877,#6695,.T.);
#13477=EDGE_CURVE('',#10877,#10878,#6696,.T.);
#13478=EDGE_CURVE('',#10878,#10854,#6697,.T.);
#13479=EDGE_CURVE('',#10854,#10858,#6698,.T.);
#13480=EDGE_CURVE('',#10858,#10875,#6699,.T.);
#13481=EDGE_CURVE('',#10879,#10879,#9387,.T.);
#13482=EDGE_CURVE('',#10879,#10869,#6700,.T.);
#13483=EDGE_CURVE('',#10880,#10880,#9388,.T.);
#13484=EDGE_CURVE('',#10880,#10870,#6701,.T.);
#13485=EDGE_CURVE('',#10881,#10881,#9389,.T.);
#13486=EDGE_CURVE('',#10881,#10873,#6702,.T.);
#13487=EDGE_CURVE('',#10882,#10882,#9390,.T.);
#13488=EDGE_CURVE('',#10882,#10874,#6703,.T.);
#13489=EDGE_CURVE('',#10883,#10884,#6704,.T.);
#13490=EDGE_CURVE('',#10884,#10875,#6705,.T.);
#13491=EDGE_CURVE('',#10883,#10878,#6706,.T.);
#13492=EDGE_CURVE('',#10885,#10883,#6707,.T.);
#13493=EDGE_CURVE('',#10885,#10877,#6708,.T.);
#13494=EDGE_CURVE('',#10886,#10885,#6709,.T.);
#13495=EDGE_CURVE('',#10886,#10876,#6710,.T.);
#13496=EDGE_CURVE('',#10884,#10886,#6711,.T.);
#13497=EDGE_CURVE('',#10887,#10887,#9391,.T.);
#13498=EDGE_CURVE('',#10887,#10888,#6712,.T.);
#13499=EDGE_CURVE('',#10888,#10888,#9392,.T.);
#13500=EDGE_CURVE('',#10889,#10889,#9393,.T.);
#13501=EDGE_CURVE('',#10889,#10890,#6713,.T.);
#13502=EDGE_CURVE('',#10890,#10890,#9394,.T.);
#13503=EDGE_CURVE('',#10891,#10891,#9395,.T.);
#13504=EDGE_CURVE('',#10891,#10892,#6714,.T.);
#13505=EDGE_CURVE('',#10892,#10892,#9396,.T.);
#13506=EDGE_CURVE('',#10893,#10893,#9397,.T.);
#13507=EDGE_CURVE('',#10893,#10894,#6715,.T.);
#13508=EDGE_CURVE('',#10894,#10894,#9398,.T.);
#13509=EDGE_CURVE('',#10895,#10895,#9399,.T.);
#13510=EDGE_CURVE('',#10895,#10896,#6716,.T.);
#13511=EDGE_CURVE('',#10896,#10896,#9400,.T.);
#13512=EDGE_CURVE('',#10897,#10897,#9401,.T.);
#13513=EDGE_CURVE('',#10897,#10898,#6717,.T.);
#13514=EDGE_CURVE('',#10898,#10898,#9402,.T.);
#13515=EDGE_CURVE('',#10899,#10899,#9403,.T.);
#13516=EDGE_CURVE('',#10899,#10900,#6718,.T.);
#13517=EDGE_CURVE('',#10900,#10900,#9404,.T.);
#13518=EDGE_CURVE('',#10901,#10902,#6719,.T.);
#13519=EDGE_CURVE('',#10902,#10903,#6720,.T.);
#13520=EDGE_CURVE('',#10904,#10903,#6721,.T.);
#13521=EDGE_CURVE('',#10901,#10904,#6722,.T.);
#13522=EDGE_CURVE('',#10905,#10901,#6723,.T.);
#13523=EDGE_CURVE('',#10906,#10904,#6724,.T.);
#13524=EDGE_CURVE('',#10905,#10906,#6725,.T.);
#13525=EDGE_CURVE('',#10907,#10905,#6726,.T.);
#13526=EDGE_CURVE('',#10908,#10906,#6727,.T.);
#13527=EDGE_CURVE('',#10907,#10908,#6728,.T.);
#13528=EDGE_CURVE('',#10902,#10907,#6729,.T.);
#13529=EDGE_CURVE('',#10903,#10908,#6730,.T.);
#13530=EDGE_CURVE('',#10909,#10909,#9405,.T.);
#13531=EDGE_CURVE('',#10909,#10910,#6731,.T.);
#13532=EDGE_CURVE('',#10910,#10910,#9406,.T.);
#13533=EDGE_CURVE('',#10911,#10911,#9407,.T.);
#13534=EDGE_CURVE('',#10911,#10912,#6732,.T.);
#13535=EDGE_CURVE('',#10912,#10912,#9408,.T.);
#13536=EDGE_CURVE('',#10913,#10913,#9409,.T.);
#13537=EDGE_CURVE('',#10913,#10914,#6733,.T.);
#13538=EDGE_CURVE('',#10914,#10914,#9410,.T.);
#13539=EDGE_CURVE('',#10915,#10915,#9411,.T.);
#13540=EDGE_CURVE('',#10915,#10916,#6734,.T.);
#13541=EDGE_CURVE('',#10916,#10916,#9412,.T.);
#13542=EDGE_CURVE('',#10917,#10917,#9413,.T.);
#13543=EDGE_CURVE('',#10917,#10918,#6735,.T.);
#13544=EDGE_CURVE('',#10918,#10918,#9414,.T.);
#13545=EDGE_CURVE('',#10919,#10919,#9415,.T.);
#13546=EDGE_CURVE('',#10919,#10920,#6736,.T.);
#13547=EDGE_CURVE('',#10920,#10920,#9416,.T.);
#13548=EDGE_CURVE('',#10921,#10921,#9417,.T.);
#13549=EDGE_CURVE('',#10921,#10922,#6737,.T.);
#13550=EDGE_CURVE('',#10922,#10922,#9418,.T.);
#13551=EDGE_CURVE('',#10923,#10923,#9419,.T.);
#13552=EDGE_CURVE('',#10923,#10924,#6738,.T.);
#13553=EDGE_CURVE('',#10924,#10924,#9420,.T.);
#13554=EDGE_CURVE('',#10925,#10925,#9421,.T.);
#13555=EDGE_CURVE('',#10925,#10926,#6739,.T.);
#13556=EDGE_CURVE('',#10926,#10926,#9422,.T.);
#13557=EDGE_CURVE('',#10927,#10927,#9423,.T.);
#13558=EDGE_CURVE('',#10927,#10928,#6740,.T.);
#13559=EDGE_CURVE('',#10928,#10928,#9424,.T.);
#13560=EDGE_CURVE('',#10929,#10929,#9425,.T.);
#13561=EDGE_CURVE('',#10930,#10930,#9426,.T.);
#13562=EDGE_CURVE('',#10930,#10929,#6741,.T.);
#13563=EDGE_CURVE('',#10931,#10931,#9427,.T.);
#13564=EDGE_CURVE('',#10931,#10932,#6742,.T.);
#13565=EDGE_CURVE('',#10932,#10932,#9428,.T.);
#13566=EDGE_CURVE('',#10933,#10933,#9429,.T.);
#13567=EDGE_CURVE('',#10933,#10934,#6743,.T.);
#13568=EDGE_CURVE('',#10934,#10934,#9430,.T.);
#13569=EDGE_CURVE('',#10935,#10936,#6744,.T.);
#13570=EDGE_CURVE('',#10936,#10937,#6745,.T.);
#13571=EDGE_CURVE('',#10938,#10937,#6746,.T.);
#13572=EDGE_CURVE('',#10935,#10938,#6747,.T.);
#13573=EDGE_CURVE('',#10939,#10935,#6748,.T.);
#13574=EDGE_CURVE('',#10940,#10938,#6749,.T.);
#13575=EDGE_CURVE('',#10939,#10940,#6750,.T.);
#13576=EDGE_CURVE('',#10941,#10939,#6751,.T.);
#13577=EDGE_CURVE('',#10942,#10940,#6752,.T.);
#13578=EDGE_CURVE('',#10941,#10942,#6753,.T.);
#13579=EDGE_CURVE('',#10936,#10941,#6754,.T.);
#13580=EDGE_CURVE('',#10937,#10942,#6755,.T.);
#13581=EDGE_CURVE('',#10943,#10943,#9431,.T.);
#13582=EDGE_CURVE('',#10943,#10944,#6756,.T.);
#13583=EDGE_CURVE('',#10944,#10944,#9432,.T.);
#13584=EDGE_CURVE('',#10945,#10945,#9433,.T.);
#13585=EDGE_CURVE('',#10945,#10946,#6757,.T.);
#13586=EDGE_CURVE('',#10946,#10946,#9434,.T.);
#13587=EDGE_CURVE('',#10947,#10947,#9435,.T.);
#13588=EDGE_CURVE('',#10947,#10948,#6758,.T.);
#13589=EDGE_CURVE('',#10948,#10948,#9436,.T.);
#13590=EDGE_CURVE('',#10949,#10950,#6759,.T.);
#13591=EDGE_CURVE('',#10951,#10949,#6760,.T.);
#13592=EDGE_CURVE('',#10952,#10951,#6761,.T.);
#13593=EDGE_CURVE('',#10950,#10952,#6762,.T.);
#13594=EDGE_CURVE('',#10951,#10949,#9437,.T.);
#13595=EDGE_CURVE('',#10953,#10953,#9438,.T.);
#13596=EDGE_CURVE('',#10952,#10950,#9439,.T.);
#13597=EDGE_CURVE('',#10953,#10954,#6763,.T.);
#13598=EDGE_CURVE('',#10954,#10954,#9440,.T.);
#13599=EDGE_CURVE('',#10955,#10955,#9441,.T.);
#13600=EDGE_CURVE('',#10956,#10956,#9442,.T.);
#13601=EDGE_CURVE('',#10956,#10955,#6764,.T.);
#13602=EDGE_CURVE('',#10957,#10957,#9443,.T.);
#13603=EDGE_CURVE('',#10957,#10958,#6765,.T.);
#13604=EDGE_CURVE('',#10958,#10958,#9444,.T.);
#13605=EDGE_CURVE('',#10959,#10959,#9445,.T.);
#13606=EDGE_CURVE('',#10960,#10960,#9446,.T.);
#13607=EDGE_CURVE('',#10960,#10959,#6766,.T.);
#13608=EDGE_CURVE('',#10961,#10962,#6767,.T.);
#13609=EDGE_CURVE('',#10962,#10963,#6768,.T.);
#13610=EDGE_CURVE('',#10964,#10963,#6769,.T.);
#13611=EDGE_CURVE('',#10961,#10964,#6770,.T.);
#13612=EDGE_CURVE('',#10965,#10961,#6771,.T.);
#13613=EDGE_CURVE('',#10966,#10964,#6772,.T.);
#13614=EDGE_CURVE('',#10965,#10966,#6773,.T.);
#13615=EDGE_CURVE('',#10967,#10965,#6774,.T.);
#13616=EDGE_CURVE('',#10968,#10966,#6775,.T.);
#13617=EDGE_CURVE('',#10967,#10968,#6776,.T.);
#13618=EDGE_CURVE('',#10962,#10967,#6777,.T.);
#13619=EDGE_CURVE('',#10963,#10968,#6778,.T.);
#13620=EDGE_CURVE('',#10969,#10969,#9447,.T.);
#13621=EDGE_CURVE('',#10969,#10970,#6779,.T.);
#13622=EDGE_CURVE('',#10970,#10970,#9448,.T.);
#13623=EDGE_CURVE('',#10971,#10971,#9449,.T.);
#13624=EDGE_CURVE('',#10972,#10972,#9450,.T.);
#13625=EDGE_CURVE('',#10972,#10971,#6780,.T.);
#13626=EDGE_CURVE('',#10973,#10974,#6781,.T.);
#13627=EDGE_CURVE('',#10974,#10975,#6782,.T.);
#13628=EDGE_CURVE('',#10976,#10975,#6783,.T.);
#13629=EDGE_CURVE('',#10973,#10976,#6784,.T.);
#13630=EDGE_CURVE('',#10977,#10973,#6785,.T.);
#13631=EDGE_CURVE('',#10978,#10976,#6786,.T.);
#13632=EDGE_CURVE('',#10977,#10978,#6787,.T.);
#13633=EDGE_CURVE('',#10979,#10977,#6788,.T.);
#13634=EDGE_CURVE('',#10980,#10978,#6789,.T.);
#13635=EDGE_CURVE('',#10979,#10980,#6790,.T.);
#13636=EDGE_CURVE('',#10974,#10979,#6791,.T.);
#13637=EDGE_CURVE('',#10975,#10980,#6792,.T.);
#13638=EDGE_CURVE('',#10981,#10981,#9451,.T.);
#13639=EDGE_CURVE('',#10981,#10982,#6793,.T.);
#13640=EDGE_CURVE('',#10982,#10982,#9452,.T.);
#13641=EDGE_CURVE('',#10983,#10983,#9453,.T.);
#13642=EDGE_CURVE('',#10984,#10984,#9454,.T.);
#13643=EDGE_CURVE('',#10984,#10985,#6794,.T.);
#13644=EDGE_CURVE('',#10985,#10985,#9455,.T.);
#13645=EDGE_CURVE('',#10986,#10986,#9456,.T.);
#13646=EDGE_CURVE('',#10987,#10987,#9457,.T.);
#13647=EDGE_CURVE('',#10987,#10988,#6795,.T.);
#13648=EDGE_CURVE('',#10988,#10988,#9458,.T.);
#13649=EDGE_CURVE('',#10989,#10989,#9459,.T.);
#13650=EDGE_CURVE('',#10990,#10990,#9460,.T.);
#13651=EDGE_CURVE('',#10990,#10991,#6796,.T.);
#13652=EDGE_CURVE('',#10991,#10991,#9461,.T.);
#13653=EDGE_CURVE('',#10992,#10992,#9462,.T.);
#13654=EDGE_CURVE('',#10993,#10993,#9463,.T.);
#13655=EDGE_CURVE('',#10993,#10983,#6797,.T.);
#13656=EDGE_CURVE('',#10994,#10994,#9464,.T.);
#13657=EDGE_CURVE('',#10994,#10986,#6798,.T.);
#13658=EDGE_CURVE('',#10995,#10995,#9465,.T.);
#13659=EDGE_CURVE('',#10995,#10989,#6799,.T.);
#13660=EDGE_CURVE('',#10996,#10996,#9466,.T.);
#13661=EDGE_CURVE('',#10996,#10992,#6800,.T.);
#13662=EDGE_CURVE('',#10997,#10998,#6801,.T.);
#13663=EDGE_CURVE('',#10998,#10999,#6802,.T.);
#13664=EDGE_CURVE('',#11000,#10999,#6803,.T.);
#13665=EDGE_CURVE('',#10997,#11000,#6804,.T.);
#13666=EDGE_CURVE('',#11001,#10997,#6805,.T.);
#13667=EDGE_CURVE('',#11002,#11000,#6806,.T.);
#13668=EDGE_CURVE('',#11001,#11002,#6807,.T.);
#13669=EDGE_CURVE('',#11003,#11001,#6808,.T.);
#13670=EDGE_CURVE('',#11004,#11002,#6809,.T.);
#13671=EDGE_CURVE('',#11003,#11004,#6810,.T.);
#13672=EDGE_CURVE('',#11005,#11003,#6811,.T.);
#13673=EDGE_CURVE('',#11006,#11004,#6812,.T.);
#13674=EDGE_CURVE('',#11005,#11006,#6813,.T.);
#13675=EDGE_CURVE('',#11007,#11005,#6814,.T.);
#13676=EDGE_CURVE('',#11008,#11006,#6815,.T.);
#13677=EDGE_CURVE('',#11007,#11008,#6816,.T.);
#13678=EDGE_CURVE('',#11009,#11007,#6817,.T.);
#13679=EDGE_CURVE('',#11010,#11008,#6818,.T.);
#13680=EDGE_CURVE('',#11009,#11010,#6819,.T.);
#13681=EDGE_CURVE('',#11011,#11009,#6820,.T.);
#13682=EDGE_CURVE('',#11012,#11010,#6821,.T.);
#13683=EDGE_CURVE('',#11011,#11012,#6822,.T.);
#13684=EDGE_CURVE('',#11013,#11011,#6823,.T.);
#13685=EDGE_CURVE('',#11014,#11012,#6824,.T.);
#13686=EDGE_CURVE('',#11013,#11014,#6825,.T.);
#13687=EDGE_CURVE('',#11015,#11013,#6826,.T.);
#13688=EDGE_CURVE('',#11016,#11014,#6827,.T.);
#13689=EDGE_CURVE('',#11015,#11016,#6828,.T.);
#13690=EDGE_CURVE('',#11017,#11015,#6829,.T.);
#13691=EDGE_CURVE('',#11018,#11016,#6830,.T.);
#13692=EDGE_CURVE('',#11017,#11018,#6831,.T.);
#13693=EDGE_CURVE('',#11019,#11017,#6832,.T.);
#13694=EDGE_CURVE('',#11020,#11018,#6833,.T.);
#13695=EDGE_CURVE('',#11019,#11020,#6834,.T.);
#13696=EDGE_CURVE('',#10998,#11019,#6835,.T.);
#13697=EDGE_CURVE('',#10999,#11020,#6836,.T.);
#13698=EDGE_CURVE('',#11021,#11022,#9467,.T.);
#13699=EDGE_CURVE('',#11022,#11021,#9468,.T.);
#13700=EDGE_CURVE('',#11022,#11023,#9469,.T.);
#13701=EDGE_CURVE('',#11024,#11023,#9470,.T.);
#13702=EDGE_CURVE('',#11023,#11024,#9471,.T.);
#13703=EDGE_CURVE('',#11024,#11025,#6837,.T.);
#13704=EDGE_CURVE('',#11025,#11025,#9472,.T.);
#13705=EDGE_CURVE('',#11026,#11026,#9473,.T.);
#13706=EDGE_CURVE('',#11026,#11027,#6838,.T.);
#13707=EDGE_CURVE('',#11027,#11027,#9474,.T.);
#13708=EDGE_CURVE('',#11027,#11028,#6839,.T.);
#13709=EDGE_CURVE('',#11028,#11028,#9475,.T.);
#13710=EDGE_CURVE('',#11029,#11029,#9476,.T.);
#13711=EDGE_CURVE('',#11029,#11021,#6840,.T.);
#13712=EDGE_CURVE('',#11030,#11030,#9477,.T.);
#13713=EDGE_CURVE('',#11030,#11026,#6841,.T.);
#13714=EDGE_CURVE('',#11031,#11032,#9478,.T.);
#13715=EDGE_CURVE('',#11032,#11031,#9479,.T.);
#13716=EDGE_CURVE('',#11032,#11033,#9480,.T.);
#13717=EDGE_CURVE('',#11034,#11033,#9481,.T.);
#13718=EDGE_CURVE('',#11033,#11034,#9482,.T.);
#13719=EDGE_CURVE('',#11035,#11035,#9483,.T.);
#13720=EDGE_CURVE('',#11035,#11034,#6842,.T.);
#13721=EDGE_CURVE('',#11036,#11036,#9484,.T.);
#13722=EDGE_CURVE('',#11037,#11037,#9485,.T.);
#13723=EDGE_CURVE('',#11038,#11038,#9486,.T.);
#13724=EDGE_CURVE('',#11038,#11036,#6843,.T.);
#13725=EDGE_CURVE('',#11039,#11039,#9487,.T.);
#13726=EDGE_CURVE('',#11039,#11038,#6844,.T.);
#13727=EDGE_CURVE('',#11040,#11040,#9488,.T.);
#13728=EDGE_CURVE('',#11040,#11039,#6845,.T.);
#13729=EDGE_CURVE('',#11031,#11037,#6846,.T.);
#13730=EDGE_CURVE('',#11041,#11042,#9489,.T.);
#13731=EDGE_CURVE('',#11043,#11044,#9490,.T.);
#13732=EDGE_CURVE('',#11045,#11046,#9491,.T.);
#13733=EDGE_CURVE('',#11047,#11048,#9492,.T.);
#13734=EDGE_CURVE('',#11049,#11050,#9493,.T.);
#13735=EDGE_CURVE('',#11051,#11052,#9494,.T.);
#13736=EDGE_CURVE('',#11053,#11054,#9495,.T.);
#13737=EDGE_CURVE('',#11055,#11056,#1037,.T.);
#13738=EDGE_CURVE('',#11057,#11055,#9496,.T.);
#13739=EDGE_CURVE('',#11058,#11057,#1038,.T.);
#13740=EDGE_CURVE('',#11056,#11058,#9497,.T.);
#13741=EDGE_CURVE('',#11059,#11057,#9498,.T.);
#13742=EDGE_CURVE('',#11059,#11060,#1039,.T.);
#13743=EDGE_CURVE('',#11061,#11060,#9499,.T.);
#13744=EDGE_CURVE('',#11061,#11062,#1040,.T.);
#13745=EDGE_CURVE('',#11063,#11062,#9500,.T.);
#13746=EDGE_CURVE('',#11063,#11064,#6847,.T.);
#13747=EDGE_CURVE('',#11064,#11064,#9501,.T.);
#13748=EDGE_CURVE('',#11065,#11063,#9502,.T.);
#13749=EDGE_CURVE('',#11065,#11066,#1041,.T.);
#13750=EDGE_CURVE('',#11067,#11066,#9503,.T.);
#13751=EDGE_CURVE('',#11067,#11068,#1042,.T.);
#13752=EDGE_CURVE('',#11069,#11068,#9504,.T.);
#13753=EDGE_CURVE('',#11069,#11070,#1043,.T.);
#13754=EDGE_CURVE('',#11071,#11070,#9505,.T.);
#13755=EDGE_CURVE('',#11071,#11072,#1044,.T.);
#13756=EDGE_CURVE('',#11058,#11072,#9506,.T.);
#13757=EDGE_CURVE('',#11055,#11073,#9507,.T.);
#13758=EDGE_CURVE('',#11073,#11059,#9508,.T.);
#13759=EDGE_CURVE('',#11074,#11073,#1045,.T.);
#13760=EDGE_CURVE('',#11060,#11074,#9509,.T.);
#13761=EDGE_CURVE('',#11074,#11075,#9510,.T.);
#13762=EDGE_CURVE('',#11075,#11061,#9511,.T.);
#13763=EDGE_CURVE('',#11076,#11075,#1046,.T.);
#13764=EDGE_CURVE('',#11062,#11076,#9512,.T.);
#13765=EDGE_CURVE('',#11076,#11077,#9513,.T.);
#13766=EDGE_CURVE('',#11077,#11078,#9514,.T.);
#13767=EDGE_CURVE('',#11078,#11065,#9515,.T.);
#13768=EDGE_CURVE('',#11079,#11078,#1047,.T.);
#13769=EDGE_CURVE('',#11066,#11079,#9516,.T.);
#13770=EDGE_CURVE('',#11079,#11080,#9517,.T.);
#13771=EDGE_CURVE('',#11080,#11067,#9518,.T.);
#13772=EDGE_CURVE('',#11081,#11080,#1048,.T.);
#13773=EDGE_CURVE('',#11068,#11081,#9519,.T.);
#13774=EDGE_CURVE('',#11081,#11082,#9520,.T.);
#13775=EDGE_CURVE('',#11082,#11069,#9521,.T.);
#13776=EDGE_CURVE('',#11083,#11082,#1049,.T.);
#13777=EDGE_CURVE('',#11070,#11083,#9522,.T.);
#13778=EDGE_CURVE('',#11084,#11084,#9523,.T.);
#13779=EDGE_CURVE('',#11084,#11077,#6848,.T.);
#13780=EDGE_CURVE('',#11085,#11056,#9524,.T.);
#13781=EDGE_CURVE('',#11085,#11086,#1050,.T.);
#13782=EDGE_CURVE('',#11083,#11086,#9525,.T.);
#13783=EDGE_CURVE('',#11072,#11085,#9526,.T.);
#13784=EDGE_CURVE('',#11086,#11071,#9527,.T.);
#13785=EDGE_CURVE('',#11087,#11087,#9528,.T.);
#13786=EDGE_CURVE('',#11088,#11088,#9529,.T.);
#13787=EDGE_CURVE('',#11089,#11089,#9530,.T.);
#13788=EDGE_CURVE('',#11089,#11087,#6849,.T.);
#13789=EDGE_CURVE('',#11090,#11090,#9531,.T.);
#13790=EDGE_CURVE('',#11090,#11088,#6850,.T.);
#13791=EDGE_CURVE('',#11091,#11091,#9532,.T.);
#13792=EDGE_CURVE('',#11092,#11092,#9533,.T.);
#13793=EDGE_CURVE('',#11093,#11093,#9534,.T.);
#13794=EDGE_CURVE('',#11093,#11091,#6851,.T.);
#13795=EDGE_CURVE('',#11094,#11094,#9535,.T.);
#13796=EDGE_CURVE('',#11094,#11092,#6852,.T.);
#13797=EDGE_CURVE('',#11095,#11096,#9536,.T.);
#13798=EDGE_CURVE('',#11096,#11095,#9537,.T.);
#13799=EDGE_CURVE('',#11096,#11097,#9538,.T.);
#13800=EDGE_CURVE('',#11098,#11097,#9539,.T.);
#13801=EDGE_CURVE('',#11097,#11098,#9540,.T.);
#13802=EDGE_CURVE('',#11098,#11099,#6853,.T.);
#13803=EDGE_CURVE('',#11099,#11099,#9541,.T.);
#13804=EDGE_CURVE('',#11100,#11100,#9542,.T.);
#13805=EDGE_CURVE('',#11100,#11101,#6854,.T.);
#13806=EDGE_CURVE('',#11101,#11101,#9543,.T.);
#13807=EDGE_CURVE('',#11101,#11102,#6855,.T.);
#13808=EDGE_CURVE('',#11102,#11102,#9544,.T.);
#13809=EDGE_CURVE('',#11103,#11103,#9545,.T.);
#13810=EDGE_CURVE('',#11103,#11095,#6856,.T.);
#13811=EDGE_CURVE('',#11104,#11104,#9546,.T.);
#13812=EDGE_CURVE('',#11104,#11100,#6857,.T.);
#13813=EDGE_CURVE('',#11105,#11106,#9547,.T.);
#13814=EDGE_CURVE('',#11106,#11105,#9548,.T.);
#13815=EDGE_CURVE('',#11106,#11107,#9549,.T.);
#13816=EDGE_CURVE('',#11108,#11107,#9550,.T.);
#13817=EDGE_CURVE('',#11107,#11108,#9551,.T.);
#13818=EDGE_CURVE('',#11109,#11109,#9552,.T.);
#13819=EDGE_CURVE('',#11109,#11108,#6858,.T.);
#13820=EDGE_CURVE('',#11110,#11110,#9553,.T.);
#13821=EDGE_CURVE('',#11111,#11111,#9554,.T.);
#13822=EDGE_CURVE('',#11112,#11112,#9555,.T.);
#13823=EDGE_CURVE('',#11112,#11110,#6859,.T.);
#13824=EDGE_CURVE('',#11113,#11113,#9556,.T.);
#13825=EDGE_CURVE('',#11113,#11112,#6860,.T.);
#13826=EDGE_CURVE('',#11114,#11114,#9557,.T.);
#13827=EDGE_CURVE('',#11114,#11113,#6861,.T.);
#13828=EDGE_CURVE('',#11105,#11111,#6862,.T.);
#13829=EDGE_CURVE('',#11115,#11116,#9558,.T.);
#13830=EDGE_CURVE('',#11117,#11118,#9559,.T.);
#13831=EDGE_CURVE('',#11119,#11120,#9560,.T.);
#13832=EDGE_CURVE('',#11121,#11122,#9561,.T.);
#13833=EDGE_CURVE('',#11123,#11124,#9562,.T.);
#13834=EDGE_CURVE('',#11125,#11126,#9563,.T.);
#13835=EDGE_CURVE('',#11127,#11128,#9564,.T.);
#13836=EDGE_CURVE('',#11129,#11130,#9565,.T.);
#13837=EDGE_CURVE('',#11131,#11132,#1051,.T.);
#13838=EDGE_CURVE('',#11133,#11131,#9566,.T.);
#13839=EDGE_CURVE('',#11134,#11133,#1052,.T.);
#13840=EDGE_CURVE('',#11132,#11134,#9567,.T.);
#13841=EDGE_CURVE('',#11135,#11133,#9568,.T.);
#13842=EDGE_CURVE('',#11135,#11136,#1053,.T.);
#13843=EDGE_CURVE('',#11137,#11136,#9569,.T.);
#13844=EDGE_CURVE('',#11137,#11138,#1054,.T.);
#13845=EDGE_CURVE('',#11139,#11138,#9570,.T.);
#13846=EDGE_CURVE('',#11139,#11140,#1055,.T.);
#13847=EDGE_CURVE('',#11140,#11141,#6863,.T.);
#13848=EDGE_CURVE('',#11141,#11141,#9571,.T.);
#13849=EDGE_CURVE('',#11140,#11142,#1056,.T.);
#13850=EDGE_CURVE('',#11143,#11142,#9572,.T.);
#13851=EDGE_CURVE('',#11143,#11144,#1057,.T.);
#13852=EDGE_CURVE('',#11145,#11144,#9573,.T.);
#13853=EDGE_CURVE('',#11145,#11146,#1058,.T.);
#13854=EDGE_CURVE('',#11147,#11146,#9574,.T.);
#13855=EDGE_CURVE('',#11147,#11148,#1059,.T.);
#13856=EDGE_CURVE('',#11149,#11148,#9575,.T.);
#13857=EDGE_CURVE('',#11149,#11150,#1060,.T.);
#13858=EDGE_CURVE('',#11134,#11150,#9576,.T.);
#13859=EDGE_CURVE('',#11131,#11151,#9577,.T.);
#13860=EDGE_CURVE('',#11151,#11135,#9578,.T.);
#13861=EDGE_CURVE('',#11152,#11151,#1061,.T.);
#13862=EDGE_CURVE('',#11136,#11152,#9579,.T.);
#13863=EDGE_CURVE('',#11152,#11153,#9580,.T.);
#13864=EDGE_CURVE('',#11153,#11137,#9581,.T.);
#13865=EDGE_CURVE('',#11154,#11153,#1062,.T.);
#13866=EDGE_CURVE('',#11138,#11154,#9582,.T.);
#13867=EDGE_CURVE('',#11154,#11155,#9583,.T.);
#13868=EDGE_CURVE('',#11155,#11139,#9584,.T.);
#13869=EDGE_CURVE('',#11156,#11157,#1063,.T.);
#13870=EDGE_CURVE('',#11142,#11156,#9585,.T.);
#13871=EDGE_CURVE('',#11157,#11155,#1064,.T.);
#13872=EDGE_CURVE('',#11156,#11158,#9586,.T.);
#13873=EDGE_CURVE('',#11158,#11143,#9587,.T.);
#13874=EDGE_CURVE('',#11159,#11158,#1065,.T.);
#13875=EDGE_CURVE('',#11144,#11159,#9588,.T.);
#13876=EDGE_CURVE('',#11159,#11160,#9589,.T.);
#13877=EDGE_CURVE('',#11160,#11145,#9590,.T.);
#13878=EDGE_CURVE('',#11161,#11160,#1066,.T.);
#13879=EDGE_CURVE('',#11146,#11161,#9591,.T.);
#13880=EDGE_CURVE('',#11161,#11162,#9592,.T.);
#13881=EDGE_CURVE('',#11162,#11147,#9593,.T.);
#13882=EDGE_CURVE('',#11163,#11162,#1067,.T.);
#13883=EDGE_CURVE('',#11148,#11163,#9594,.T.);
#13884=EDGE_CURVE('',#11164,#11164,#9595,.T.);
#13885=EDGE_CURVE('',#11164,#11157,#6864,.T.);
#13886=EDGE_CURVE('',#11165,#11132,#9596,.T.);
#13887=EDGE_CURVE('',#11165,#11166,#1068,.T.);
#13888=EDGE_CURVE('',#11163,#11166,#9597,.T.);
#13889=EDGE_CURVE('',#11150,#11165,#9598,.T.);
#13890=EDGE_CURVE('',#11166,#11149,#9599,.T.);
#13891=EDGE_CURVE('',#11167,#11167,#9600,.T.);
#13892=EDGE_CURVE('',#11168,#11168,#9601,.T.);
#13893=EDGE_CURVE('',#11169,#11169,#9602,.T.);
#13894=EDGE_CURVE('',#11169,#11167,#6865,.T.);
#13895=EDGE_CURVE('',#11170,#11170,#9603,.T.);
#13896=EDGE_CURVE('',#11170,#11168,#6866,.T.);
#13897=EDGE_CURVE('',#11171,#11171,#9604,.T.);
#13898=EDGE_CURVE('',#11172,#11172,#9605,.T.);
#13899=EDGE_CURVE('',#11173,#11173,#9606,.T.);
#13900=EDGE_CURVE('',#11173,#11171,#6867,.T.);
#13901=EDGE_CURVE('',#11174,#11174,#9607,.T.);
#13902=EDGE_CURVE('',#11174,#11172,#6868,.T.);
#13903=EDGE_CURVE('',#11175,#11176,#6869,.T.);
#13904=EDGE_CURVE('',#11176,#11177,#6870,.T.);
#13905=EDGE_CURVE('',#11177,#11178,#6871,.T.);
#13906=EDGE_CURVE('',#11175,#11178,#6872,.T.);
#13907=EDGE_CURVE('',#11176,#11179,#6873,.T.);
#13908=EDGE_CURVE('',#11179,#11180,#6874,.T.);
#13909=EDGE_CURVE('',#11180,#11177,#6875,.T.);
#13910=EDGE_CURVE('',#11179,#11181,#6876,.T.);
#13911=EDGE_CURVE('',#11181,#11182,#6877,.T.);
#13912=EDGE_CURVE('',#11182,#11180,#6878,.T.);
#13913=EDGE_CURVE('',#11181,#11183,#6879,.T.);
#13914=EDGE_CURVE('',#11183,#11184,#6880,.T.);
#13915=EDGE_CURVE('',#11184,#11182,#6881,.T.);
#13916=EDGE_CURVE('',#11183,#11185,#6882,.T.);
#13917=EDGE_CURVE('',#11185,#11186,#6883,.T.);
#13918=EDGE_CURVE('',#11186,#11184,#6884,.T.);
#13919=EDGE_CURVE('',#11185,#11175,#6885,.T.);
#13920=EDGE_CURVE('',#11178,#11186,#6886,.T.);
#13921=EDGE_CURVE('',#11187,#11187,#9608,.T.);
#13922=EDGE_CURVE('',#11188,#11188,#9609,.T.);
#13923=EDGE_CURVE('',#11189,#11189,#9610,.T.);
#13924=EDGE_CURVE('',#11189,#11188,#6887,.T.);
#13925=EDGE_CURVE('',#11190,#11190,#9611,.T.);
#13926=EDGE_CURVE('',#11190,#11189,#6888,.T.);
#13927=EDGE_CURVE('',#11191,#11191,#9612,.T.);
#13928=EDGE_CURVE('',#11191,#11190,#6889,.T.);
#13929=EDGE_CURVE('',#11192,#11192,#9613,.T.);
#13930=EDGE_CURVE('',#11193,#11193,#9614,.F.);
#13931=EDGE_CURVE('',#11193,#11192,#6890,.T.);
#13932=EDGE_CURVE('',#11187,#11193,#6891,.T.);
#13933=EDGE_CURVE('',#11194,#11194,#9615,.T.);
#13934=EDGE_CURVE('',#11194,#11195,#6892,.T.);
#13935=EDGE_CURVE('',#11195,#11195,#9616,.T.);
#13936=EDGE_CURVE('',#11196,#11196,#9617,.T.);
#13937=EDGE_CURVE('',#11196,#11197,#6893,.T.);
#13938=EDGE_CURVE('',#11197,#11197,#9618,.T.);
#13939=EDGE_CURVE('',#11198,#11198,#9619,.T.);
#13940=EDGE_CURVE('',#11198,#11199,#6894,.T.);
#13941=EDGE_CURVE('',#11199,#11199,#9620,.T.);
#13942=EDGE_CURVE('',#11200,#11200,#9621,.T.);
#13943=EDGE_CURVE('',#11200,#11201,#6895,.T.);
#13944=EDGE_CURVE('',#11201,#11201,#9622,.T.);
#13945=EDGE_CURVE('',#11202,#11203,#6896,.T.);
#13946=EDGE_CURVE('',#11203,#11204,#6897,.T.);
#13947=EDGE_CURVE('',#11205,#11204,#6898,.T.);
#13948=EDGE_CURVE('',#11202,#11205,#6899,.T.);
#13949=EDGE_CURVE('',#11206,#11202,#6900,.T.);
#13950=EDGE_CURVE('',#11207,#11205,#6901,.T.);
#13951=EDGE_CURVE('',#11206,#11207,#6902,.T.);
#13952=EDGE_CURVE('',#11208,#11206,#6903,.T.);
#13953=EDGE_CURVE('',#11209,#11207,#6904,.T.);
#13954=EDGE_CURVE('',#11208,#11209,#6905,.T.);
#13955=EDGE_CURVE('',#11203,#11208,#6906,.T.);
#13956=EDGE_CURVE('',#11204,#11209,#6907,.T.);
#13957=EDGE_CURVE('',#11210,#11210,#9623,.T.);
#13958=EDGE_CURVE('',#11210,#11211,#6908,.T.);
#13959=EDGE_CURVE('',#11211,#11211,#9624,.T.);
#13960=EDGE_CURVE('',#11212,#11212,#9625,.T.);
#13961=EDGE_CURVE('',#11212,#11213,#6909,.T.);
#13962=EDGE_CURVE('',#11213,#11213,#9626,.T.);
#13963=EDGE_CURVE('',#11214,#11214,#9627,.T.);
#13964=EDGE_CURVE('',#11214,#11215,#6910,.T.);
#13965=EDGE_CURVE('',#11215,#11215,#9628,.T.);
#13966=EDGE_CURVE('',#11216,#11216,#9629,.T.);
#13967=EDGE_CURVE('',#11216,#11217,#6911,.T.);
#13968=EDGE_CURVE('',#11217,#11217,#9630,.T.);
#13969=EDGE_CURVE('',#11218,#11218,#9631,.T.);
#13970=EDGE_CURVE('',#11218,#11219,#6912,.T.);
#13971=EDGE_CURVE('',#11219,#11219,#9632,.T.);
#13972=EDGE_CURVE('',#11220,#11220,#9633,.T.);
#13973=EDGE_CURVE('',#11220,#11221,#6913,.T.);
#13974=EDGE_CURVE('',#11221,#11221,#9634,.T.);
#13975=EDGE_CURVE('',#11222,#11222,#9635,.T.);
#13976=EDGE_CURVE('',#11222,#11223,#6914,.T.);
#13977=EDGE_CURVE('',#11223,#11223,#9636,.T.);
#13978=EDGE_CURVE('',#11224,#11224,#9637,.T.);
#13979=EDGE_CURVE('',#11224,#11225,#6915,.T.);
#13980=EDGE_CURVE('',#11225,#11225,#9638,.T.);
#13981=EDGE_CURVE('',#11226,#11227,#6916,.T.);
#13982=EDGE_CURVE('',#11227,#11228,#6917,.T.);
#13983=EDGE_CURVE('',#11229,#11228,#6918,.T.);
#13984=EDGE_CURVE('',#11226,#11229,#6919,.T.);
#13985=EDGE_CURVE('',#11230,#11226,#6920,.T.);
#13986=EDGE_CURVE('',#11231,#11229,#6921,.T.);
#13987=EDGE_CURVE('',#11230,#11231,#6922,.T.);
#13988=EDGE_CURVE('',#11232,#11230,#6923,.T.);
#13989=EDGE_CURVE('',#11233,#11231,#6924,.T.);
#13990=EDGE_CURVE('',#11232,#11233,#6925,.T.);
#13991=EDGE_CURVE('',#11227,#11232,#6926,.T.);
#13992=EDGE_CURVE('',#11228,#11233,#6927,.T.);
#13993=EDGE_CURVE('',#11234,#11234,#9639,.T.);
#13994=EDGE_CURVE('',#11234,#11235,#6928,.T.);
#13995=EDGE_CURVE('',#11235,#11235,#9640,.T.);
#13996=EDGE_CURVE('',#11236,#11236,#9641,.T.);
#13997=EDGE_CURVE('',#11236,#11237,#6929,.T.);
#13998=EDGE_CURVE('',#11237,#11237,#9642,.T.);
#13999=EDGE_CURVE('',#11238,#11238,#9643,.T.);
#14000=EDGE_CURVE('',#11238,#11239,#6930,.T.);
#14001=EDGE_CURVE('',#11239,#11239,#9644,.T.);
#14002=EDGE_CURVE('',#11240,#11240,#9645,.T.);
#14003=EDGE_CURVE('',#11240,#11241,#6931,.T.);
#14004=EDGE_CURVE('',#11241,#11241,#9646,.T.);
#14005=EDGE_CURVE('',#11242,#11242,#9647,.T.);
#14006=EDGE_CURVE('',#11242,#11243,#6932,.T.);
#14007=EDGE_CURVE('',#11243,#11243,#9648,.T.);
#14008=EDGE_CURVE('',#11244,#11244,#9649,.T.);
#14009=EDGE_CURVE('',#11244,#11245,#6933,.T.);
#14010=EDGE_CURVE('',#11245,#11245,#9650,.T.);
#14011=EDGE_CURVE('',#11246,#11246,#9651,.T.);
#14012=EDGE_CURVE('',#11246,#11247,#6934,.T.);
#14013=EDGE_CURVE('',#11247,#11247,#9652,.T.);
#14014=EDGE_CURVE('',#11248,#11248,#9653,.T.);
#14015=EDGE_CURVE('',#11248,#11249,#6935,.T.);
#14016=EDGE_CURVE('',#11249,#11249,#9654,.T.);
#14017=EDGE_CURVE('',#11250,#11251,#6936,.T.);
#14018=EDGE_CURVE('',#11251,#11252,#6937,.T.);
#14019=EDGE_CURVE('',#11253,#11252,#6938,.T.);
#14020=EDGE_CURVE('',#11250,#11253,#6939,.T.);
#14021=EDGE_CURVE('',#11254,#11250,#6940,.T.);
#14022=EDGE_CURVE('',#11255,#11253,#6941,.T.);
#14023=EDGE_CURVE('',#11254,#11255,#6942,.T.);
#14024=EDGE_CURVE('',#11256,#11254,#6943,.T.);
#14025=EDGE_CURVE('',#11257,#11255,#6944,.T.);
#14026=EDGE_CURVE('',#11256,#11257,#6945,.T.);
#14027=EDGE_CURVE('',#11251,#11256,#6946,.T.);
#14028=EDGE_CURVE('',#11252,#11257,#6947,.T.);
#14029=EDGE_CURVE('',#11258,#11259,#6948,.T.);
#14030=EDGE_CURVE('',#11258,#11259,#9655,.T.);
#14031=EDGE_CURVE('',#11260,#11258,#6949,.T.);
#14032=EDGE_CURVE('',#11261,#11260,#9656,.T.);
#14033=EDGE_CURVE('',#11261,#11262,#6950,.T.);
#14034=EDGE_CURVE('',#11262,#11262,#9657,.T.);
#14035=EDGE_CURVE('',#11263,#11261,#9658,.T.);
#14036=EDGE_CURVE('',#11259,#11263,#6951,.T.);
#14037=EDGE_CURVE('',#11264,#11265,#6952,.T.);
#14038=EDGE_CURVE('',#11264,#11265,#9659,.T.);
#14039=EDGE_CURVE('',#11266,#11264,#6953,.T.);
#14040=EDGE_CURVE('',#11267,#11266,#9660,.T.);
#14041=EDGE_CURVE('',#11267,#11268,#6954,.T.);
#14042=EDGE_CURVE('',#11268,#11268,#9661,.T.);
#14043=EDGE_CURVE('',#11269,#11267,#9662,.T.);
#14044=EDGE_CURVE('',#11265,#11269,#6955,.T.);
#14045=EDGE_CURVE('',#11270,#11271,#6956,.T.);
#14046=EDGE_CURVE('',#11270,#11271,#9663,.T.);
#14047=EDGE_CURVE('',#11272,#11270,#6957,.T.);
#14048=EDGE_CURVE('',#11273,#11272,#9664,.T.);
#14049=EDGE_CURVE('',#11273,#11274,#6958,.T.);
#14050=EDGE_CURVE('',#11274,#11274,#9665,.T.);
#14051=EDGE_CURVE('',#11275,#11273,#9666,.T.);
#14052=EDGE_CURVE('',#11271,#11275,#6959,.T.);
#14053=EDGE_CURVE('',#11276,#11277,#6960,.T.);
#14054=EDGE_CURVE('',#11276,#11277,#9667,.T.);
#14055=EDGE_CURVE('',#11278,#11276,#6961,.T.);
#14056=EDGE_CURVE('',#11279,#11278,#9668,.T.);
#14057=EDGE_CURVE('',#11279,#11280,#6962,.T.);
#14058=EDGE_CURVE('',#11280,#11280,#9669,.T.);
#14059=EDGE_CURVE('',#11281,#11279,#9670,.T.);
#14060=EDGE_CURVE('',#11277,#11281,#6963,.T.);
#14061=EDGE_CURVE('',#11263,#11272,#6964,.T.);
#14062=EDGE_CURVE('',#11275,#11282,#6965,.T.);
#14063=EDGE_CURVE('',#11283,#11282,#6966,.T.);
#14064=EDGE_CURVE('',#11283,#11284,#6967,.T.);
#14065=EDGE_CURVE('',#11285,#11284,#6968,.T.);
#14066=EDGE_CURVE('',#11285,#11260,#6969,.T.);
#14067=EDGE_CURVE('',#11269,#11278,#6970,.T.);
#14068=EDGE_CURVE('',#11281,#11286,#6971,.T.);
#14069=EDGE_CURVE('',#11287,#11286,#6972,.T.);
#14070=EDGE_CURVE('',#11288,#11287,#6973,.T.);
#14071=EDGE_CURVE('',#11289,#11288,#6974,.T.);
#14072=EDGE_CURVE('',#11289,#11266,#6975,.T.);
#14073=EDGE_CURVE('',#11282,#11290,#6976,.T.);
#14074=EDGE_CURVE('',#11290,#11291,#6977,.T.);
#14075=EDGE_CURVE('',#11291,#11292,#6978,.T.);
#14076=EDGE_CURVE('',#11292,#11293,#6979,.T.);
#14077=EDGE_CURVE('',#11293,#11289,#6980,.T.);
#14078=EDGE_CURVE('',#11288,#11294,#6981,.T.);
#14079=EDGE_CURVE('',#11294,#11295,#6982,.T.);
#14080=EDGE_CURVE('',#11295,#11296,#6983,.T.);
#14081=EDGE_CURVE('',#11296,#11297,#6984,.T.);
#14082=EDGE_CURVE('',#11297,#11283,#6985,.T.);
#14083=EDGE_CURVE('',#11298,#11285,#6986,.T.);
#14084=EDGE_CURVE('',#11290,#11298,#6987,.T.);
#14085=EDGE_CURVE('',#11299,#11298,#6988,.T.);
#14086=EDGE_CURVE('',#11291,#11299,#6989,.T.);
#14087=EDGE_CURVE('',#11300,#11299,#6990,.T.);
#14088=EDGE_CURVE('',#11292,#11300,#6991,.T.);
#14089=EDGE_CURVE('',#11301,#11300,#6992,.T.);
#14090=EDGE_CURVE('',#11293,#11301,#6993,.T.);
#14091=EDGE_CURVE('',#11286,#11301,#6994,.T.);
#14092=EDGE_CURVE('',#11302,#11287,#6995,.T.);
#14093=EDGE_CURVE('',#11294,#11302,#6996,.T.);
#14094=EDGE_CURVE('',#11303,#11302,#6997,.T.);
#14095=EDGE_CURVE('',#11295,#11303,#6998,.T.);
#14096=EDGE_CURVE('',#11304,#11303,#6999,.T.);
#14097=EDGE_CURVE('',#11296,#11304,#7000,.T.);
#14098=EDGE_CURVE('',#11305,#11304,#7001,.T.);
#14099=EDGE_CURVE('',#11297,#11305,#7002,.T.);
#14100=EDGE_CURVE('',#11284,#11305,#7003,.T.);
#14101=EDGE_CURVE('',#11306,#11307,#7004,.T.);
#14102=EDGE_CURVE('',#11307,#11308,#7005,.T.);
#14103=EDGE_CURVE('',#11309,#11308,#7006,.T.);
#14104=EDGE_CURVE('',#11306,#11309,#7007,.T.);
#14105=EDGE_CURVE('',#11310,#11306,#7008,.T.);
#14106=EDGE_CURVE('',#11311,#11309,#7009,.T.);
#14107=EDGE_CURVE('',#11310,#11311,#7010,.T.);
#14108=EDGE_CURVE('',#11312,#11310,#7011,.T.);
#14109=EDGE_CURVE('',#11313,#11311,#7012,.T.);
#14110=EDGE_CURVE('',#11312,#11313,#7013,.T.);
#14111=EDGE_CURVE('',#11314,#11312,#7014,.T.);
#14112=EDGE_CURVE('',#11315,#11313,#7015,.T.);
#14113=EDGE_CURVE('',#11314,#11315,#7016,.T.);
#14114=EDGE_CURVE('',#11316,#11314,#7017,.T.);
#14115=EDGE_CURVE('',#11317,#11315,#7018,.T.);
#14116=EDGE_CURVE('',#11316,#11317,#7019,.T.);
#14117=EDGE_CURVE('',#11318,#11316,#7020,.T.);
#14118=EDGE_CURVE('',#11319,#11317,#7021,.T.);
#14119=EDGE_CURVE('',#11318,#11319,#7022,.T.);
#14120=EDGE_CURVE('',#11320,#11318,#7023,.T.);
#14121=EDGE_CURVE('',#11321,#11319,#7024,.T.);
#14122=EDGE_CURVE('',#11320,#11321,#7025,.T.);
#14123=EDGE_CURVE('',#11307,#11320,#7026,.T.);
#14124=EDGE_CURVE('',#11308,#11321,#7027,.T.);
#14125=EDGE_CURVE('',#11322,#11323,#7028,.T.);
#14126=EDGE_CURVE('',#11322,#11324,#7029,.T.);
#14127=EDGE_CURVE('',#11325,#11324,#7030,.T.);
#14128=EDGE_CURVE('',#11323,#11325,#7031,.T.);
#14129=EDGE_CURVE('',#11323,#11326,#7032,.T.);
#14130=EDGE_CURVE('',#11327,#11325,#7033,.T.);
#14131=EDGE_CURVE('',#11326,#11327,#7034,.T.);
#14132=EDGE_CURVE('',#11326,#11328,#7035,.T.);
#14133=EDGE_CURVE('',#11329,#11327,#7036,.T.);
#14134=EDGE_CURVE('',#11328,#11329,#7037,.T.);
#14135=EDGE_CURVE('',#11328,#11330,#7038,.T.);
#14136=EDGE_CURVE('',#11331,#11329,#7039,.T.);
#14137=EDGE_CURVE('',#11330,#11331,#7040,.T.);
#14138=EDGE_CURVE('',#11330,#11332,#7041,.T.);
#14139=EDGE_CURVE('',#11333,#11331,#7042,.T.);
#14140=EDGE_CURVE('',#11332,#11333,#7043,.T.);
#14141=EDGE_CURVE('',#11332,#11334,#7044,.T.);
#14142=EDGE_CURVE('',#11335,#11333,#7045,.T.);
#14143=EDGE_CURVE('',#11334,#11335,#7046,.T.);
#14144=EDGE_CURVE('',#11334,#11336,#7047,.T.);
#14145=EDGE_CURVE('',#11337,#11335,#7048,.T.);
#14146=EDGE_CURVE('',#11336,#11337,#7049,.T.);
#14147=EDGE_CURVE('',#11336,#11322,#7050,.T.);
#14148=EDGE_CURVE('',#11324,#11337,#7051,.T.);
#14149=EDGE_CURVE('',#11338,#11338,#9671,.T.);
#14150=EDGE_CURVE('',#11338,#11339,#7052,.T.);
#14151=EDGE_CURVE('',#11339,#11339,#9672,.T.);
#14152=EDGE_CURVE('',#11339,#11340,#7053,.T.);
#14153=EDGE_CURVE('',#11340,#11340,#9673,.T.);
#14154=EDGE_CURVE('',#11341,#11341,#9674,.T.);
#14155=EDGE_CURVE('',#11341,#11342,#7054,.T.);
#14156=EDGE_CURVE('',#11342,#11342,#9675,.T.);
#14157=EDGE_CURVE('',#11343,#11344,#7055,.T.);
#14158=EDGE_CURVE('',#11344,#11345,#7056,.T.);
#14159=EDGE_CURVE('',#11345,#11346,#7057,.T.);
#14160=EDGE_CURVE('',#11343,#11346,#7058,.T.);
#14161=EDGE_CURVE('',#11344,#11347,#7059,.T.);
#14162=EDGE_CURVE('',#11347,#11348,#7060,.T.);
#14163=EDGE_CURVE('',#11348,#11345,#7061,.T.);
#14164=EDGE_CURVE('',#11347,#11349,#7062,.T.);
#14165=EDGE_CURVE('',#11349,#11350,#7063,.T.);
#14166=EDGE_CURVE('',#11350,#11348,#7064,.T.);
#14167=EDGE_CURVE('',#11349,#11351,#7065,.T.);
#14168=EDGE_CURVE('',#11351,#11352,#7066,.T.);
#14169=EDGE_CURVE('',#11352,#11350,#7067,.T.);
#14170=EDGE_CURVE('',#11351,#11353,#7068,.T.);
#14171=EDGE_CURVE('',#11353,#11354,#7069,.T.);
#14172=EDGE_CURVE('',#11354,#11352,#7070,.T.);
#14173=EDGE_CURVE('',#11353,#11343,#7071,.T.);
#14174=EDGE_CURVE('',#11346,#11354,#7072,.T.);
#14175=EDGE_CURVE('',#11355,#11355,#9676,.T.);
#14176=EDGE_CURVE('',#11356,#11356,#9677,.T.);
#14177=EDGE_CURVE('',#11355,#11357,#7073,.T.);
#14178=EDGE_CURVE('',#11357,#11357,#9678,.T.);
#14179=EDGE_CURVE('',#11358,#11358,#9679,.T.);
#14180=EDGE_CURVE('',#11359,#11359,#9680,.T.);
#14181=EDGE_CURVE('',#11359,#11358,#7074,.T.);
#14182=EDGE_CURVE('',#11360,#11360,#9681,.T.);
#14183=EDGE_CURVE('',#11360,#11359,#7075,.T.);
#14184=EDGE_CURVE('',#11361,#11361,#9682,.T.);
#14185=EDGE_CURVE('',#11361,#11360,#7076,.T.);
#14186=EDGE_CURVE('',#11362,#11362,#9683,.T.);
#14187=EDGE_CURVE('',#11363,#11363,#9684,.F.);
#14188=EDGE_CURVE('',#11363,#11362,#7077,.T.);
#14189=EDGE_CURVE('',#11356,#11363,#7078,.T.);
#14190=EDGE_CURVE('',#11364,#11365,#7079,.T.);
#14191=EDGE_CURVE('',#11365,#11366,#1069,.T.);
#14192=EDGE_CURVE('',#11366,#11367,#9685,.F.);
#14193=EDGE_CURVE('',#11367,#11364,#1070,.T.);
#14194=EDGE_CURVE('',#11368,#11369,#7080,.T.);
#14195=EDGE_CURVE('',#11369,#11365,#1071,.T.);
#14196=EDGE_CURVE('',#11364,#11368,#1072,.T.);
#14197=EDGE_CURVE('',#11370,#11371,#7081,.T.);
#14198=EDGE_CURVE('',#11371,#11369,#1073,.T.);
#14199=EDGE_CURVE('',#11368,#11370,#1074,.T.);
#14200=EDGE_CURVE('',#11372,#11373,#7082,.T.);
#14201=EDGE_CURVE('',#11373,#11371,#1075,.T.);
#14202=EDGE_CURVE('',#11370,#11372,#1076,.T.);
#14203=EDGE_CURVE('',#11374,#11375,#7083,.T.);
#14204=EDGE_CURVE('',#11375,#11373,#1077,.T.);
#14205=EDGE_CURVE('',#11372,#11374,#1078,.T.);
#14206=EDGE_CURVE('',#11376,#11377,#7084,.T.);
#14207=EDGE_CURVE('',#11377,#11375,#1079,.T.);
#14208=EDGE_CURVE('',#11374,#11376,#1080,.T.);
#14209=EDGE_CURVE('',#11378,#11379,#7085,.T.);
#14210=EDGE_CURVE('',#11379,#11377,#1081,.T.);
#14211=EDGE_CURVE('',#11376,#11378,#1082,.T.);
#14212=EDGE_CURVE('',#11380,#11381,#7086,.T.);
#14213=EDGE_CURVE('',#11381,#11379,#1083,.T.);
#14214=EDGE_CURVE('',#11378,#11380,#1084,.T.);
#14215=EDGE_CURVE('',#11382,#11383,#7087,.T.);
#14216=EDGE_CURVE('',#11384,#11382,#9686,.F.);
#14217=EDGE_CURVE('',#11384,#11383,#1085,.T.);
#14218=EDGE_CURVE('',#11385,#11386,#7088,.T.);
#14219=EDGE_CURVE('',#11386,#11387,#1086,.T.);
#14220=EDGE_CURVE('',#11388,#11387,#9687,.T.);
#14221=EDGE_CURVE('',#11385,#11388,#1087,.T.);
#14222=EDGE_CURVE('',#11389,#11390,#7089,.T.);
#14223=EDGE_CURVE('',#11390,#11386,#1088,.T.);
#14224=EDGE_CURVE('',#11389,#11385,#1089,.T.);
#14225=EDGE_CURVE('',#11391,#11392,#7090,.T.);
#14226=EDGE_CURVE('',#11392,#11390,#1090,.T.);
#14227=EDGE_CURVE('',#11391,#11389,#1091,.T.);
#14228=EDGE_CURVE('',#11393,#11394,#7091,.T.);
#14229=EDGE_CURVE('',#11394,#11392,#1092,.T.);
#14230=EDGE_CURVE('',#11393,#11391,#1093,.T.);
#14231=EDGE_CURVE('',#11395,#11396,#7092,.T.);
#14232=EDGE_CURVE('',#11396,#11394,#1094,.T.);
#14233=EDGE_CURVE('',#11395,#11393,#1095,.T.);
#14234=EDGE_CURVE('',#11397,#11398,#7093,.T.);
#14235=EDGE_CURVE('',#11398,#11396,#1096,.T.);
#14236=EDGE_CURVE('',#11397,#11395,#1097,.T.);
#14237=EDGE_CURVE('',#11399,#11400,#7094,.T.);
#14238=EDGE_CURVE('',#11400,#11398,#1098,.T.);
#14239=EDGE_CURVE('',#11399,#11397,#1099,.T.);
#14240=EDGE_CURVE('',#11401,#11402,#7095,.T.);
#14241=EDGE_CURVE('',#11402,#11400,#1100,.T.);
#14242=EDGE_CURVE('',#11401,#11399,#1101,.T.);
#14243=EDGE_CURVE('',#11403,#11404,#7096,.T.);
#14244=EDGE_CURVE('',#11405,#11403,#1102,.T.);
#14245=EDGE_CURVE('',#11406,#11405,#9688,.T.);
#14246=EDGE_CURVE('',#11406,#11404,#1103,.T.);
#14247=EDGE_CURVE('',#11404,#11402,#1104,.T.);
#14248=EDGE_CURVE('',#11403,#11401,#1105,.T.);
#14249=EDGE_CURVE('',#11387,#11384,#1106,.T.);
#14250=EDGE_CURVE('',#11366,#11406,#1107,.T.);
#14251=EDGE_CURVE('',#11383,#11381,#1108,.T.);
#14252=EDGE_CURVE('',#11407,#11388,#1109,.T.);
#14253=EDGE_CURVE('',#11380,#11407,#1110,.T.);
#14254=EDGE_CURVE('',#11405,#11367,#1111,.T.);
#14255=EDGE_CURVE('',#11408,#11409,#7097,.T.);
#14256=EDGE_CURVE('',#11409,#11408,#9689,.T.);
#14257=EDGE_CURVE('',#11382,#11407,#9690,.F.);
#14258=EDGE_CURVE('',#11410,#11410,#9691,.T.);
#14259=EDGE_CURVE('',#11411,#11411,#9692,.T.);
#14260=EDGE_CURVE('',#11412,#11412,#9693,.T.);
#14261=EDGE_CURVE('',#11413,#11413,#9694,.T.);
#14262=EDGE_CURVE('',#11413,#11412,#7098,.T.);
#14263=EDGE_CURVE('',#11414,#11414,#9695,.T.);
#14264=EDGE_CURVE('',#11414,#11411,#7099,.T.);
#14265=EDGE_CURVE('',#11415,#11415,#9696,.T.);
#14266=EDGE_CURVE('',#11415,#11410,#7100,.T.);
#14267=EDGE_CURVE('',#11416,#11417,#7101,.T.);
#14268=EDGE_CURVE('',#11409,#11416,#7102,.T.);
#14269=EDGE_CURVE('',#11417,#11408,#7103,.T.);
#14270=EDGE_CURVE('',#11416,#11417,#9697,.T.);
#14271=EDGE_CURVE('',#11418,#11418,#9698,.T.);
#14272=EDGE_CURVE('',#11418,#11419,#7104,.T.);
#14273=EDGE_CURVE('',#11419,#11419,#9699,.T.);
#14274=EDGE_CURVE('',#11420,#11420,#9700,.T.);
#14275=EDGE_CURVE('',#11421,#11421,#9701,.T.);
#14276=EDGE_CURVE('',#11421,#11420,#7105,.T.);
#14277=EDGE_CURVE('',#11422,#11422,#9702,.T.);
#14278=EDGE_CURVE('',#11422,#11421,#7106,.T.);
#14279=EDGE_CURVE('',#11423,#11423,#9703,.T.);
#14280=EDGE_CURVE('',#11423,#11422,#7107,.T.);
#14281=EDGE_CURVE('',#11424,#11424,#9704,.T.);
#14282=EDGE_CURVE('',#11425,#11425,#9705,.F.);
#14283=EDGE_CURVE('',#11425,#11424,#7108,.T.);
#14284=EDGE_CURVE('',#11426,#11426,#9706,.F.);
#14285=EDGE_CURVE('',#11426,#11425,#7109,.T.);
#14286=EDGE_CURVE('',#11427,#11427,#9707,.T.);
#14287=EDGE_CURVE('',#11427,#11426,#7110,.T.);
#14288=EDGE_CURVE('',#11428,#11429,#7111,.T.);
#14289=EDGE_CURVE('',#11429,#11430,#7112,.T.);
#14290=EDGE_CURVE('',#11430,#11431,#7113,.T.);
#14291=EDGE_CURVE('',#11428,#11431,#7114,.T.);
#14292=EDGE_CURVE('',#11429,#11432,#7115,.T.);
#14293=EDGE_CURVE('',#11432,#11433,#7116,.T.);
#14294=EDGE_CURVE('',#11433,#11430,#7117,.T.);
#14295=EDGE_CURVE('',#11432,#11434,#7118,.T.);
#14296=EDGE_CURVE('',#11434,#11435,#7119,.T.);
#14297=EDGE_CURVE('',#11435,#11433,#7120,.T.);
#14298=EDGE_CURVE('',#11434,#11436,#7121,.T.);
#14299=EDGE_CURVE('',#11436,#11437,#7122,.T.);
#14300=EDGE_CURVE('',#11437,#11435,#7123,.T.);
#14301=EDGE_CURVE('',#11436,#11438,#7124,.T.);
#14302=EDGE_CURVE('',#11438,#11439,#7125,.T.);
#14303=EDGE_CURVE('',#11439,#11437,#7126,.T.);
#14304=EDGE_CURVE('',#11438,#11428,#7127,.T.);
#14305=EDGE_CURVE('',#11431,#11439,#7128,.T.);
#14306=EDGE_CURVE('',#11440,#11440,#9708,.T.);
#14307=EDGE_CURVE('',#11441,#11441,#9709,.T.);
#14308=EDGE_CURVE('',#11441,#11440,#7129,.T.);
#14309=EDGE_CURVE('',#11442,#11442,#9710,.T.);
#14310=EDGE_CURVE('',#11442,#11441,#7130,.T.);
#14311=EDGE_CURVE('',#11443,#11443,#9711,.T.);
#14312=EDGE_CURVE('',#11443,#11442,#7131,.T.);
#14313=EDGE_CURVE('',#11444,#11444,#9712,.T.);
#14314=EDGE_CURVE('',#11445,#11445,#9713,.F.);
#14315=EDGE_CURVE('',#11445,#11444,#7132,.T.);
#14316=EDGE_CURVE('',#11446,#11446,#9714,.F.);
#14317=EDGE_CURVE('',#11446,#11445,#7133,.T.);
#14318=EDGE_CURVE('',#11447,#11447,#9715,.T.);
#14319=EDGE_CURVE('',#11447,#11446,#7134,.T.);
#14320=EDGE_CURVE('',#11448,#11449,#7135,.T.);
#14321=EDGE_CURVE('',#11449,#11450,#7136,.T.);
#14322=EDGE_CURVE('',#11450,#11451,#7137,.T.);
#14323=EDGE_CURVE('',#11448,#11451,#7138,.T.);
#14324=EDGE_CURVE('',#11449,#11452,#7139,.T.);
#14325=EDGE_CURVE('',#11452,#11453,#7140,.T.);
#14326=EDGE_CURVE('',#11453,#11450,#7141,.T.);
#14327=EDGE_CURVE('',#11452,#11454,#7142,.T.);
#14328=EDGE_CURVE('',#11454,#11455,#7143,.T.);
#14329=EDGE_CURVE('',#11455,#11453,#7144,.T.);
#14330=EDGE_CURVE('',#11454,#11456,#7145,.T.);
#14331=EDGE_CURVE('',#11456,#11457,#7146,.T.);
#14332=EDGE_CURVE('',#11457,#11455,#7147,.T.);
#14333=EDGE_CURVE('',#11456,#11458,#7148,.T.);
#14334=EDGE_CURVE('',#11458,#11459,#7149,.T.);
#14335=EDGE_CURVE('',#11459,#11457,#7150,.T.);
#14336=EDGE_CURVE('',#11458,#11448,#7151,.T.);
#14337=EDGE_CURVE('',#11451,#11459,#7152,.T.);
#14338=EDGE_CURVE('',#11460,#11461,#7153,.T.);
#14339=EDGE_CURVE('',#11460,#11462,#1112,.T.);
#14340=EDGE_CURVE('',#11462,#11463,#9716,.F.);
#14341=EDGE_CURVE('',#11463,#11461,#1113,.T.);
#14342=EDGE_CURVE('',#11464,#11465,#7154,.T.);
#14343=EDGE_CURVE('',#11464,#11460,#1114,.T.);
#14344=EDGE_CURVE('',#11461,#11465,#1115,.T.);
#14345=EDGE_CURVE('',#11466,#11467,#7155,.T.);
#14346=EDGE_CURVE('',#11466,#11464,#1116,.T.);
#14347=EDGE_CURVE('',#11465,#11467,#1117,.T.);
#14348=EDGE_CURVE('',#11468,#11469,#7156,.T.);
#14349=EDGE_CURVE('',#11468,#11466,#1118,.T.);
#14350=EDGE_CURVE('',#11467,#11469,#1119,.T.);
#14351=EDGE_CURVE('',#11470,#11471,#7157,.T.);
#14352=EDGE_CURVE('',#11470,#11468,#1120,.T.);
#14353=EDGE_CURVE('',#11469,#11471,#1121,.T.);
#14354=EDGE_CURVE('',#11472,#11473,#7158,.T.);
#14355=EDGE_CURVE('',#11472,#11470,#1122,.T.);
#14356=EDGE_CURVE('',#11471,#11473,#1123,.T.);
#14357=EDGE_CURVE('',#11474,#11475,#7159,.T.);
#14358=EDGE_CURVE('',#11474,#11472,#1124,.T.);
#14359=EDGE_CURVE('',#11473,#11475,#1125,.T.);
#14360=EDGE_CURVE('',#11476,#11477,#7160,.T.);
#14361=EDGE_CURVE('',#11476,#11474,#1126,.T.);
#14362=EDGE_CURVE('',#11475,#11477,#1127,.T.);
#14363=EDGE_CURVE('',#11478,#11479,#7161,.T.);
#14364=EDGE_CURVE('',#11478,#11476,#1128,.T.);
#14365=EDGE_CURVE('',#11477,#11479,#1129,.T.);
#14366=EDGE_CURVE('',#11480,#11481,#7162,.T.);
#14367=EDGE_CURVE('',#11480,#11478,#1130,.T.);
#14368=EDGE_CURVE('',#11479,#11481,#1131,.T.);
#14369=EDGE_CURVE('',#11482,#11483,#7163,.T.);
#14370=EDGE_CURVE('',#11482,#11480,#1132,.T.);
#14371=EDGE_CURVE('',#11481,#11483,#1133,.T.);
#14372=EDGE_CURVE('',#11484,#11485,#7164,.T.);
#14373=EDGE_CURVE('',#11484,#11482,#1134,.T.);
#14374=EDGE_CURVE('',#11483,#11485,#1135,.T.);
#14375=EDGE_CURVE('',#11486,#11487,#7165,.T.);
#14376=EDGE_CURVE('',#11486,#11484,#1136,.T.);
#14377=EDGE_CURVE('',#11485,#11487,#1137,.T.);
#14378=EDGE_CURVE('',#11488,#11489,#7166,.T.);
#14379=EDGE_CURVE('',#11488,#11486,#1138,.T.);
#14380=EDGE_CURVE('',#11487,#11489,#1139,.T.);
#14381=EDGE_CURVE('',#11490,#11491,#7167,.T.);
#14382=EDGE_CURVE('',#11490,#11488,#1140,.T.);
#14383=EDGE_CURVE('',#11489,#11491,#1141,.T.);
#14384=EDGE_CURVE('',#11492,#11493,#7168,.T.);
#14385=EDGE_CURVE('',#11492,#11490,#1142,.T.);
#14386=EDGE_CURVE('',#11491,#11493,#1143,.T.);
#14387=EDGE_CURVE('',#11494,#11495,#7169,.T.);
#14388=EDGE_CURVE('',#11494,#11492,#1144,.T.);
#14389=EDGE_CURVE('',#11493,#11495,#1145,.T.);
#14390=EDGE_CURVE('',#11496,#11497,#7170,.T.);
#14391=EDGE_CURVE('',#11496,#11494,#1146,.T.);
#14392=EDGE_CURVE('',#11495,#11497,#1147,.T.);
#14393=EDGE_CURVE('',#11498,#11499,#7171,.T.);
#14394=EDGE_CURVE('',#11498,#11496,#1148,.T.);
#14395=EDGE_CURVE('',#11497,#11499,#1149,.T.);
#14396=EDGE_CURVE('',#11500,#11501,#7172,.T.);
#14397=EDGE_CURVE('',#11500,#11498,#1150,.T.);
#14398=EDGE_CURVE('',#11499,#11501,#1151,.T.);
#14399=EDGE_CURVE('',#11502,#11503,#7173,.T.);
#14400=EDGE_CURVE('',#11502,#11500,#1152,.T.);
#14401=EDGE_CURVE('',#11501,#11503,#1153,.T.);
#14402=EDGE_CURVE('',#11504,#11505,#7174,.T.);
#14403=EDGE_CURVE('',#11504,#11502,#1154,.T.);
#14404=EDGE_CURVE('',#11503,#11505,#1155,.T.);
#14405=EDGE_CURVE('',#11506,#11507,#7175,.T.);
#14406=EDGE_CURVE('',#11506,#11504,#1156,.T.);
#14407=EDGE_CURVE('',#11505,#11507,#1157,.T.);
#14408=EDGE_CURVE('',#11508,#11509,#7176,.T.);
#14409=EDGE_CURVE('',#11508,#11506,#1158,.T.);
#14410=EDGE_CURVE('',#11507,#11509,#1159,.T.);
#14411=EDGE_CURVE('',#11510,#11511,#7177,.T.);
#14412=EDGE_CURVE('',#11510,#11508,#1160,.T.);
#14413=EDGE_CURVE('',#11509,#11511,#1161,.T.);
#14414=EDGE_CURVE('',#11512,#11513,#7178,.T.);
#14415=EDGE_CURVE('',#11512,#11510,#1162,.T.);
#14416=EDGE_CURVE('',#11511,#11513,#1163,.T.);
#14417=EDGE_CURVE('',#11514,#11515,#7179,.T.);
#14418=EDGE_CURVE('',#11514,#11512,#1164,.T.);
#14419=EDGE_CURVE('',#11513,#11515,#1165,.T.);
#14420=EDGE_CURVE('',#11516,#11517,#7180,.T.);
#14421=EDGE_CURVE('',#11516,#11514,#1166,.T.);
#14422=EDGE_CURVE('',#11515,#11517,#1167,.T.);
#14423=EDGE_CURVE('',#11518,#11519,#7181,.T.);
#14424=EDGE_CURVE('',#11518,#11516,#1168,.T.);
#14425=EDGE_CURVE('',#11517,#11519,#1169,.T.);
#14426=EDGE_CURVE('',#11520,#11521,#7182,.T.);
#14427=EDGE_CURVE('',#11520,#11518,#1170,.T.);
#14428=EDGE_CURVE('',#11519,#11521,#1171,.T.);
#14429=EDGE_CURVE('',#11522,#11523,#7183,.T.);
#14430=EDGE_CURVE('',#11522,#11520,#1172,.T.);
#14431=EDGE_CURVE('',#11521,#11523,#1173,.T.);
#14432=EDGE_CURVE('',#11524,#11525,#7184,.T.);
#14433=EDGE_CURVE('',#11524,#11522,#1174,.T.);
#14434=EDGE_CURVE('',#11523,#11525,#1175,.T.);
#14435=EDGE_CURVE('',#11526,#11527,#7185,.T.);
#14436=EDGE_CURVE('',#11526,#11524,#1176,.T.);
#14437=EDGE_CURVE('',#11525,#11527,#1177,.T.);
#14438=EDGE_CURVE('',#11528,#11529,#7186,.T.);
#14439=EDGE_CURVE('',#11528,#11526,#1178,.T.);
#14440=EDGE_CURVE('',#11527,#11529,#1179,.T.);
#14441=EDGE_CURVE('',#11530,#11531,#7187,.T.);
#14442=EDGE_CURVE('',#11530,#11528,#1180,.T.);
#14443=EDGE_CURVE('',#11529,#11531,#1181,.T.);
#14444=EDGE_CURVE('',#11532,#11533,#7188,.T.);
#14445=EDGE_CURVE('',#11532,#11530,#1182,.T.);
#14446=EDGE_CURVE('',#11531,#11533,#1183,.T.);
#14447=EDGE_CURVE('',#11534,#11535,#7189,.T.);
#14448=EDGE_CURVE('',#11534,#11532,#1184,.T.);
#14449=EDGE_CURVE('',#11533,#11535,#1185,.T.);
#14450=EDGE_CURVE('',#11536,#11537,#7190,.T.);
#14451=EDGE_CURVE('',#11536,#11534,#1186,.T.);
#14452=EDGE_CURVE('',#11535,#11537,#1187,.T.);
#14453=EDGE_CURVE('',#11538,#11539,#7191,.T.);
#14454=EDGE_CURVE('',#11538,#11536,#1188,.T.);
#14455=EDGE_CURVE('',#11537,#11539,#1189,.T.);
#14456=EDGE_CURVE('',#11540,#11541,#7192,.T.);
#14457=EDGE_CURVE('',#11540,#11538,#1190,.T.);
#14458=EDGE_CURVE('',#11539,#11541,#1191,.T.);
#14459=EDGE_CURVE('',#11542,#11543,#7193,.T.);
#14460=EDGE_CURVE('',#11542,#11540,#1192,.T.);
#14461=EDGE_CURVE('',#11541,#11543,#1193,.T.);
#14462=EDGE_CURVE('',#11544,#11545,#7194,.T.);
#14463=EDGE_CURVE('',#11544,#11542,#1194,.T.);
#14464=EDGE_CURVE('',#11543,#11545,#1195,.T.);
#14465=EDGE_CURVE('',#11546,#11547,#7195,.T.);
#14466=EDGE_CURVE('',#11546,#11544,#1196,.T.);
#14467=EDGE_CURVE('',#11545,#11547,#1197,.T.);
#14468=EDGE_CURVE('',#11548,#11549,#7196,.T.);
#14469=EDGE_CURVE('',#11548,#11546,#1198,.T.);
#14470=EDGE_CURVE('',#11547,#11549,#1199,.T.);
#14471=EDGE_CURVE('',#11550,#11551,#7197,.T.);
#14472=EDGE_CURVE('',#11550,#11548,#1200,.T.);
#14473=EDGE_CURVE('',#11549,#11551,#1201,.T.);
#14474=EDGE_CURVE('',#11552,#11553,#7198,.T.);
#14475=EDGE_CURVE('',#11552,#11550,#1202,.T.);
#14476=EDGE_CURVE('',#11551,#11553,#1203,.T.);
#14477=EDGE_CURVE('',#11554,#11555,#7199,.T.);
#14478=EDGE_CURVE('',#11554,#11552,#1204,.T.);
#14479=EDGE_CURVE('',#11553,#11555,#1205,.T.);
#14480=EDGE_CURVE('',#11556,#11557,#7200,.T.);
#14481=EDGE_CURVE('',#11556,#11554,#1206,.T.);
#14482=EDGE_CURVE('',#11555,#11557,#1207,.T.);
#14483=EDGE_CURVE('',#11558,#11559,#7201,.T.);
#14484=EDGE_CURVE('',#11558,#11556,#1208,.T.);
#14485=EDGE_CURVE('',#11557,#11559,#1209,.T.);
#14486=EDGE_CURVE('',#11560,#11561,#7202,.T.);
#14487=EDGE_CURVE('',#11560,#11558,#1210,.T.);
#14488=EDGE_CURVE('',#11559,#11561,#1211,.T.);
#14489=EDGE_CURVE('',#11562,#11563,#7203,.T.);
#14490=EDGE_CURVE('',#11562,#11560,#1212,.T.);
#14491=EDGE_CURVE('',#11561,#11563,#1213,.T.);
#14492=EDGE_CURVE('',#11564,#11565,#7204,.T.);
#14493=EDGE_CURVE('',#11564,#11562,#1214,.T.);
#14494=EDGE_CURVE('',#11563,#11565,#1215,.T.);
#14495=EDGE_CURVE('',#11566,#11567,#7205,.T.);
#14496=EDGE_CURVE('',#11566,#11564,#1216,.T.);
#14497=EDGE_CURVE('',#11565,#11567,#1217,.T.);
#14498=EDGE_CURVE('',#11568,#11569,#7206,.T.);
#14499=EDGE_CURVE('',#11568,#11566,#1218,.T.);
#14500=EDGE_CURVE('',#11567,#11569,#1219,.T.);
#14501=EDGE_CURVE('',#11570,#11571,#7207,.T.);
#14502=EDGE_CURVE('',#11570,#11568,#1220,.T.);
#14503=EDGE_CURVE('',#11569,#11571,#1221,.T.);
#14504=EDGE_CURVE('',#11572,#11573,#7208,.T.);
#14505=EDGE_CURVE('',#11572,#11570,#1222,.T.);
#14506=EDGE_CURVE('',#11571,#11573,#1223,.T.);
#14507=EDGE_CURVE('',#11574,#11575,#7209,.T.);
#14508=EDGE_CURVE('',#11574,#11572,#1224,.T.);
#14509=EDGE_CURVE('',#11573,#11575,#1225,.T.);
#14510=EDGE_CURVE('',#11576,#11577,#7210,.T.);
#14511=EDGE_CURVE('',#11576,#11574,#1226,.T.);
#14512=EDGE_CURVE('',#11575,#11577,#1227,.T.);
#14513=EDGE_CURVE('',#11578,#11579,#7211,.T.);
#14514=EDGE_CURVE('',#11578,#11576,#1228,.T.);
#14515=EDGE_CURVE('',#11577,#11579,#1229,.T.);
#14516=EDGE_CURVE('',#11580,#11581,#7212,.T.);
#14517=EDGE_CURVE('',#11580,#11578,#1230,.T.);
#14518=EDGE_CURVE('',#11579,#11581,#1231,.T.);
#14519=EDGE_CURVE('',#11582,#11583,#7213,.T.);
#14520=EDGE_CURVE('',#11582,#11580,#1232,.T.);
#14521=EDGE_CURVE('',#11581,#11583,#1233,.T.);
#14522=EDGE_CURVE('',#11584,#11585,#7214,.T.);
#14523=EDGE_CURVE('',#11584,#11582,#1234,.T.);
#14524=EDGE_CURVE('',#11583,#11585,#1235,.T.);
#14525=EDGE_CURVE('',#11586,#11587,#7215,.T.);
#14526=EDGE_CURVE('',#11586,#11584,#1236,.T.);
#14527=EDGE_CURVE('',#11585,#11587,#1237,.T.);
#14528=EDGE_CURVE('',#11588,#11589,#7216,.T.);
#14529=EDGE_CURVE('',#11588,#11590,#1238,.T.);
#14530=EDGE_CURVE('',#11589,#11590,#9717,.T.);
#14531=EDGE_CURVE('',#11591,#11592,#7217,.T.);
#14532=EDGE_CURVE('',#11591,#11588,#1239,.T.);
#14533=EDGE_CURVE('',#11593,#11589,#9718,.T.);
#14534=EDGE_CURVE('',#11592,#11593,#1240,.T.);
#14535=EDGE_CURVE('',#11594,#11595,#7218,.T.);
#14536=EDGE_CURVE('',#11594,#11591,#1241,.T.);
#14537=EDGE_CURVE('',#11595,#11592,#1242,.T.);
#14538=EDGE_CURVE('',#11596,#11597,#7219,.T.);
#14539=EDGE_CURVE('',#11596,#11594,#1243,.T.);
#14540=EDGE_CURVE('',#11597,#11595,#1244,.T.);
#14541=EDGE_CURVE('',#11598,#11599,#7220,.T.);
#14542=EDGE_CURVE('',#11598,#11596,#1245,.T.);
#14543=EDGE_CURVE('',#11599,#11597,#1246,.T.);
#14544=EDGE_CURVE('',#11600,#11601,#7221,.T.);
#14545=EDGE_CURVE('',#11600,#11598,#1247,.T.);
#14546=EDGE_CURVE('',#11601,#11599,#1248,.T.);
#14547=EDGE_CURVE('',#11602,#11603,#7222,.T.);
#14548=EDGE_CURVE('',#11602,#11600,#1249,.T.);
#14549=EDGE_CURVE('',#11603,#11601,#1250,.T.);
#14550=EDGE_CURVE('',#11604,#11605,#7223,.T.);
#14551=EDGE_CURVE('',#11604,#11602,#1251,.T.);
#14552=EDGE_CURVE('',#11605,#11603,#1252,.T.);
#14553=EDGE_CURVE('',#11606,#11607,#7224,.T.);
#14554=EDGE_CURVE('',#11606,#11604,#1253,.T.);
#14555=EDGE_CURVE('',#11607,#11605,#1254,.T.);
#14556=EDGE_CURVE('',#11608,#11609,#7225,.T.);
#14557=EDGE_CURVE('',#11608,#11606,#1255,.T.);
#14558=EDGE_CURVE('',#11609,#11607,#1256,.T.);
#14559=EDGE_CURVE('',#11610,#11611,#7226,.T.);
#14560=EDGE_CURVE('',#11610,#11608,#1257,.T.);
#14561=EDGE_CURVE('',#11611,#11609,#1258,.T.);
#14562=EDGE_CURVE('',#11612,#11613,#7227,.T.);
#14563=EDGE_CURVE('',#11612,#11610,#1259,.T.);
#14564=EDGE_CURVE('',#11613,#11611,#1260,.T.);
#14565=EDGE_CURVE('',#11614,#11615,#7228,.T.);
#14566=EDGE_CURVE('',#11614,#11612,#1261,.T.);
#14567=EDGE_CURVE('',#11615,#11613,#1262,.T.);
#14568=EDGE_CURVE('',#11616,#11617,#7229,.T.);
#14569=EDGE_CURVE('',#11616,#11614,#1263,.T.);
#14570=EDGE_CURVE('',#11617,#11615,#1264,.T.);
#14571=EDGE_CURVE('',#11618,#11619,#7230,.T.);
#14572=EDGE_CURVE('',#11618,#11616,#1265,.T.);
#14573=EDGE_CURVE('',#11619,#11617,#1266,.T.);
#14574=EDGE_CURVE('',#11620,#11621,#7231,.T.);
#14575=EDGE_CURVE('',#11620,#11618,#1267,.T.);
#14576=EDGE_CURVE('',#11621,#11619,#1268,.T.);
#14577=EDGE_CURVE('',#11622,#11623,#7232,.T.);
#14578=EDGE_CURVE('',#11622,#11620,#1269,.T.);
#14579=EDGE_CURVE('',#11623,#11621,#1270,.T.);
#14580=EDGE_CURVE('',#11624,#11625,#7233,.T.);
#14581=EDGE_CURVE('',#11624,#11622,#1271,.T.);
#14582=EDGE_CURVE('',#11625,#11623,#1272,.T.);
#14583=EDGE_CURVE('',#11626,#11627,#7234,.T.);
#14584=EDGE_CURVE('',#11626,#11624,#1273,.T.);
#14585=EDGE_CURVE('',#11627,#11625,#1274,.T.);
#14586=EDGE_CURVE('',#11628,#11629,#7235,.T.);
#14587=EDGE_CURVE('',#11628,#11626,#1275,.T.);
#14588=EDGE_CURVE('',#11629,#11627,#1276,.T.);
#14589=EDGE_CURVE('',#11630,#11631,#7236,.T.);
#14590=EDGE_CURVE('',#11630,#11628,#1277,.T.);
#14591=EDGE_CURVE('',#11631,#11629,#1278,.T.);
#14592=EDGE_CURVE('',#11632,#11633,#7237,.T.);
#14593=EDGE_CURVE('',#11632,#11630,#1279,.T.);
#14594=EDGE_CURVE('',#11633,#11631,#1280,.T.);
#14595=EDGE_CURVE('',#11634,#11635,#7238,.T.);
#14596=EDGE_CURVE('',#11634,#11632,#1281,.T.);
#14597=EDGE_CURVE('',#11635,#11633,#1282,.T.);
#14598=EDGE_CURVE('',#11636,#11637,#7239,.T.);
#14599=EDGE_CURVE('',#11636,#11634,#1283,.T.);
#14600=EDGE_CURVE('',#11637,#11635,#1284,.T.);
#14601=EDGE_CURVE('',#11638,#11639,#7240,.T.);
#14602=EDGE_CURVE('',#11638,#11636,#1285,.T.);
#14603=EDGE_CURVE('',#11639,#11637,#1286,.T.);
#14604=EDGE_CURVE('',#11640,#11641,#7241,.T.);
#14605=EDGE_CURVE('',#11640,#11638,#1287,.T.);
#14606=EDGE_CURVE('',#11641,#11639,#1288,.T.);
#14607=EDGE_CURVE('',#11642,#11643,#7242,.T.);
#14608=EDGE_CURVE('',#11642,#11640,#1289,.T.);
#14609=EDGE_CURVE('',#11643,#11641,#1290,.T.);
#14610=EDGE_CURVE('',#11644,#11645,#7243,.T.);
#14611=EDGE_CURVE('',#11644,#11642,#1291,.T.);
#14612=EDGE_CURVE('',#11645,#11643,#1292,.T.);
#14613=EDGE_CURVE('',#11646,#11647,#7244,.T.);
#14614=EDGE_CURVE('',#11646,#11644,#1293,.T.);
#14615=EDGE_CURVE('',#11647,#11645,#1294,.T.);
#14616=EDGE_CURVE('',#11648,#11649,#7245,.T.);
#14617=EDGE_CURVE('',#11648,#11646,#1295,.T.);
#14618=EDGE_CURVE('',#11649,#11647,#1296,.T.);
#14619=EDGE_CURVE('',#11650,#11651,#7246,.T.);
#14620=EDGE_CURVE('',#11650,#11648,#1297,.T.);
#14621=EDGE_CURVE('',#11651,#11649,#1298,.T.);
#14622=EDGE_CURVE('',#11652,#11653,#7247,.T.);
#14623=EDGE_CURVE('',#11652,#11650,#1299,.T.);
#14624=EDGE_CURVE('',#11653,#11651,#1300,.T.);
#14625=EDGE_CURVE('',#11654,#11655,#7248,.T.);
#14626=EDGE_CURVE('',#11654,#11652,#1301,.T.);
#14627=EDGE_CURVE('',#11655,#11653,#1302,.T.);
#14628=EDGE_CURVE('',#11656,#11657,#7249,.T.);
#14629=EDGE_CURVE('',#11656,#11654,#1303,.T.);
#14630=EDGE_CURVE('',#11657,#11655,#1304,.T.);
#14631=EDGE_CURVE('',#11658,#11659,#7250,.T.);
#14632=EDGE_CURVE('',#11658,#11656,#1305,.T.);
#14633=EDGE_CURVE('',#11659,#11657,#1306,.T.);
#14634=EDGE_CURVE('',#11660,#11661,#7251,.T.);
#14635=EDGE_CURVE('',#11660,#11658,#1307,.T.);
#14636=EDGE_CURVE('',#11661,#11659,#1308,.T.);
#14637=EDGE_CURVE('',#11662,#11663,#7252,.T.);
#14638=EDGE_CURVE('',#11662,#11660,#1309,.T.);
#14639=EDGE_CURVE('',#11663,#11661,#1310,.T.);
#14640=EDGE_CURVE('',#11664,#11665,#7253,.T.);
#14641=EDGE_CURVE('',#11664,#11662,#1311,.T.);
#14642=EDGE_CURVE('',#11665,#11663,#1312,.T.);
#14643=EDGE_CURVE('',#11666,#11667,#7254,.T.);
#14644=EDGE_CURVE('',#11666,#11664,#1313,.T.);
#14645=EDGE_CURVE('',#11667,#11665,#1314,.T.);
#14646=EDGE_CURVE('',#11668,#11669,#7255,.T.);
#14647=EDGE_CURVE('',#11668,#11666,#1315,.T.);
#14648=EDGE_CURVE('',#11669,#11667,#1316,.T.);
#14649=EDGE_CURVE('',#11670,#11671,#7256,.T.);
#14650=EDGE_CURVE('',#11670,#11668,#1317,.T.);
#14651=EDGE_CURVE('',#11671,#11669,#1318,.T.);
#14652=EDGE_CURVE('',#11672,#11673,#7257,.T.);
#14653=EDGE_CURVE('',#11672,#11670,#1319,.T.);
#14654=EDGE_CURVE('',#11673,#11671,#1320,.T.);
#14655=EDGE_CURVE('',#11674,#11675,#7258,.T.);
#14656=EDGE_CURVE('',#11674,#11672,#1321,.T.);
#14657=EDGE_CURVE('',#11675,#11673,#1322,.T.);
#14658=EDGE_CURVE('',#11676,#11677,#7259,.T.);
#14659=EDGE_CURVE('',#11676,#11674,#1323,.T.);
#14660=EDGE_CURVE('',#11677,#11675,#1324,.T.);
#14661=EDGE_CURVE('',#11678,#11679,#7260,.T.);
#14662=EDGE_CURVE('',#11678,#11676,#1325,.T.);
#14663=EDGE_CURVE('',#11679,#11677,#1326,.T.);
#14664=EDGE_CURVE('',#11680,#11681,#7261,.T.);
#14665=EDGE_CURVE('',#11680,#11678,#1327,.T.);
#14666=EDGE_CURVE('',#11681,#11679,#1328,.T.);
#14667=EDGE_CURVE('',#11682,#11683,#7262,.T.);
#14668=EDGE_CURVE('',#11682,#11680,#1329,.T.);
#14669=EDGE_CURVE('',#11683,#11681,#1330,.T.);
#14670=EDGE_CURVE('',#11684,#11685,#7263,.T.);
#14671=EDGE_CURVE('',#11684,#11682,#1331,.T.);
#14672=EDGE_CURVE('',#11685,#11683,#1332,.T.);
#14673=EDGE_CURVE('',#11686,#11687,#7264,.T.);
#14674=EDGE_CURVE('',#11686,#11684,#1333,.T.);
#14675=EDGE_CURVE('',#11687,#11685,#1334,.T.);
#14676=EDGE_CURVE('',#11688,#11689,#7265,.T.);
#14677=EDGE_CURVE('',#11688,#11686,#1335,.T.);
#14678=EDGE_CURVE('',#11689,#11687,#1336,.T.);
#14679=EDGE_CURVE('',#11690,#11691,#7266,.T.);
#14680=EDGE_CURVE('',#11690,#11688,#1337,.T.);
#14681=EDGE_CURVE('',#11691,#11689,#1338,.T.);
#14682=EDGE_CURVE('',#11692,#11693,#7267,.T.);
#14683=EDGE_CURVE('',#11692,#11690,#1339,.T.);
#14684=EDGE_CURVE('',#11693,#11691,#1340,.T.);
#14685=EDGE_CURVE('',#11694,#11695,#7268,.T.);
#14686=EDGE_CURVE('',#11694,#11692,#1341,.T.);
#14687=EDGE_CURVE('',#11695,#11693,#1342,.T.);
#14688=EDGE_CURVE('',#11696,#11697,#7269,.T.);
#14689=EDGE_CURVE('',#11696,#11694,#1343,.T.);
#14690=EDGE_CURVE('',#11697,#11695,#1344,.T.);
#14691=EDGE_CURVE('',#11698,#11699,#7270,.T.);
#14692=EDGE_CURVE('',#11698,#11696,#1345,.T.);
#14693=EDGE_CURVE('',#11699,#11697,#1346,.T.);
#14694=EDGE_CURVE('',#11700,#11701,#7271,.T.);
#14695=EDGE_CURVE('',#11700,#11698,#1347,.T.);
#14696=EDGE_CURVE('',#11701,#11699,#1348,.T.);
#14697=EDGE_CURVE('',#11702,#11703,#7272,.T.);
#14698=EDGE_CURVE('',#11702,#11700,#1349,.T.);
#14699=EDGE_CURVE('',#11703,#11701,#1350,.T.);
#14700=EDGE_CURVE('',#11704,#11705,#7273,.T.);
#14701=EDGE_CURVE('',#11704,#11702,#1351,.T.);
#14702=EDGE_CURVE('',#11705,#11703,#1352,.T.);
#14703=EDGE_CURVE('',#11706,#11707,#7274,.T.);
#14704=EDGE_CURVE('',#11706,#11704,#1353,.T.);
#14705=EDGE_CURVE('',#11707,#11705,#1354,.T.);
#14706=EDGE_CURVE('',#11708,#11709,#7275,.T.);
#14707=EDGE_CURVE('',#11708,#11706,#1355,.T.);
#14708=EDGE_CURVE('',#11709,#11707,#1356,.T.);
#14709=EDGE_CURVE('',#11710,#11711,#7276,.T.);
#14710=EDGE_CURVE('',#11710,#11708,#1357,.T.);
#14711=EDGE_CURVE('',#11711,#11709,#1358,.T.);
#14712=EDGE_CURVE('',#11712,#11713,#7277,.T.);
#14713=EDGE_CURVE('',#11712,#11710,#1359,.T.);
#14714=EDGE_CURVE('',#11713,#11711,#1360,.T.);
#14715=EDGE_CURVE('',#11714,#11715,#7278,.T.);
#14716=EDGE_CURVE('',#11714,#11712,#1361,.T.);
#14717=EDGE_CURVE('',#11715,#11713,#1362,.T.);
#14718=EDGE_CURVE('',#11716,#11716,#9719,.T.);
#14719=EDGE_CURVE('',#11717,#11463,#1363,.T.);
#14720=EDGE_CURVE('',#11462,#11718,#1364,.T.);
#14721=EDGE_CURVE('',#11718,#11717,#9720,.T.);
#14722=EDGE_CURVE('',#11716,#11719,#7279,.T.);
#14723=EDGE_CURVE('',#11719,#11719,#9721,.T.);
#14724=EDGE_CURVE('',#11720,#11593,#1365,.T.);
#14725=EDGE_CURVE('',#11587,#11720,#1366,.T.);
#14726=EDGE_CURVE('',#11717,#11715,#1367,.T.);
#14727=EDGE_CURVE('',#11718,#11714,#1368,.T.);
#14728=EDGE_CURVE('',#11590,#11721,#1369,.T.);
#14729=EDGE_CURVE('',#11721,#11586,#1370,.T.);
#14730=EDGE_CURVE('',#11722,#11723,#7280,.T.);
#14731=EDGE_CURVE('',#11722,#11724,#7281,.T.);
#14732=EDGE_CURVE('',#11725,#11724,#7282,.T.);
#14733=EDGE_CURVE('',#11723,#11725,#7283,.T.);
#14734=EDGE_CURVE('',#11723,#11726,#9722,.T.);
#14735=EDGE_CURVE('',#11725,#11727,#7284,.T.);
#14736=EDGE_CURVE('',#11727,#11726,#7285,.T.);
#14737=EDGE_CURVE('',#11724,#11728,#7286,.T.);
#14738=EDGE_CURVE('',#11727,#11728,#7287,.T.);
#14739=EDGE_CURVE('',#11726,#11729,#7288,.T.);
#14740=EDGE_CURVE('',#11728,#11729,#7289,.T.);
#14741=EDGE_CURVE('',#11729,#11722,#9723,.T.);
#14742=EDGE_CURVE('',#11730,#11730,#9724,.T.);
#14743=EDGE_CURVE('',#11730,#11731,#7290,.T.);
#14744=EDGE_CURVE('',#11731,#11731,#9725,.T.);
#14745=EDGE_CURVE('',#11732,#11732,#9726,.T.);
#14746=EDGE_CURVE('',#11721,#11720,#9727,.F.);
#14747=EDGE_CURVE('',#11733,#11733,#9728,.T.);
#14748=EDGE_CURVE('',#11733,#11732,#7291,.T.);
#14749=EDGE_CURVE('',#11734,#11734,#9729,.T.);
#14750=EDGE_CURVE('',#11734,#11735,#7292,.T.);
#14751=EDGE_CURVE('',#11735,#11735,#9730,.T.);
#14752=EDGE_CURVE('',#11736,#11736,#9731,.T.);
#14753=EDGE_CURVE('',#11736,#11737,#7293,.T.);
#14754=EDGE_CURVE('',#11737,#11737,#9732,.T.);
#14755=EDGE_CURVE('',#11738,#11739,#7294,.T.);
#14756=EDGE_CURVE('',#11738,#11739,#9733,.T.);
#14757=EDGE_CURVE('',#11740,#11741,#1371,.T.);
#14758=EDGE_CURVE('',#11742,#11740,#9734,.T.);
#14759=EDGE_CURVE('',#11739,#11742,#1372,.T.);
#14760=EDGE_CURVE('',#11741,#11738,#1373,.T.);
#14761=EDGE_CURVE('',#11741,#11743,#7295,.T.);
#14762=EDGE_CURVE('',#11744,#11743,#1374,.T.);
#14763=EDGE_CURVE('',#11743,#11744,#1375,.T.);
#14764=EDGE_CURVE('',#11742,#11740,#7296,.T.);
#14765=EDGE_CURVE('',#11745,#11745,#9735,.T.);
#14766=EDGE_CURVE('',#11745,#11746,#7297,.T.);
#14767=EDGE_CURVE('',#11746,#11746,#9736,.T.);
#14768=EDGE_CURVE('',#11747,#11747,#9737,.T.);
#14769=EDGE_CURVE('',#11747,#11748,#7298,.T.);
#14770=EDGE_CURVE('',#11748,#11748,#9738,.T.);
#14771=EDGE_CURVE('',#11749,#11749,#9739,.T.);
#14772=EDGE_CURVE('',#11749,#11750,#7299,.T.);
#14773=EDGE_CURVE('',#11750,#11750,#9740,.T.);
#14774=EDGE_CURVE('',#11751,#11752,#7300,.T.);
#14775=EDGE_CURVE('',#11751,#11752,#9741,.T.);
#14776=EDGE_CURVE('',#11753,#11754,#1376,.T.);
#14777=EDGE_CURVE('',#11755,#11753,#9742,.T.);
#14778=EDGE_CURVE('',#11752,#11755,#1377,.T.);
#14779=EDGE_CURVE('',#11754,#11751,#1378,.T.);
#14780=EDGE_CURVE('',#11754,#11756,#7301,.T.);
#14781=EDGE_CURVE('',#11757,#11756,#1379,.T.);
#14782=EDGE_CURVE('',#11756,#11757,#1380,.T.);
#14783=EDGE_CURVE('',#11755,#11753,#7302,.T.);
#14784=EDGE_CURVE('',#11758,#11759,#7303,.T.);
#14785=EDGE_CURVE('',#11760,#11758,#7304,.T.);
#14786=EDGE_CURVE('',#11761,#11760,#7305,.T.);
#14787=EDGE_CURVE('',#11762,#11761,#7306,.T.);
#14788=EDGE_CURVE('',#11763,#11762,#7307,.T.);
#14789=EDGE_CURVE('',#11759,#11763,#7308,.T.);
#14790=EDGE_CURVE('',#11764,#11758,#7309,.T.);
#14791=EDGE_CURVE('',#11765,#11764,#7310,.T.);
#14792=EDGE_CURVE('',#11760,#11765,#7311,.T.);
#14793=EDGE_CURVE('',#11766,#11764,#7312,.T.);
#14794=EDGE_CURVE('',#11767,#11766,#7313,.T.);
#14795=EDGE_CURVE('',#11768,#11767,#7314,.T.);
#14796=EDGE_CURVE('',#11769,#11768,#7315,.T.);
#14797=EDGE_CURVE('',#11765,#11769,#7316,.T.);
#14798=EDGE_CURVE('',#11770,#11770,#9743,.T.);
#14799=EDGE_CURVE('',#11759,#11766,#9744,.T.);
#14800=EDGE_CURVE('',#11771,#11771,#9745,.T.);
#14801=EDGE_CURVE('',#11769,#11761,#9746,.T.);
#14802=EDGE_CURVE('',#11770,#11771,#7317,.T.);
#14803=EDGE_CURVE('',#11763,#11767,#9747,.T.);
#14804=EDGE_CURVE('',#11768,#11762,#9748,.T.);
#14805=EDGE_CURVE('',#11772,#11772,#9749,.T.);
#14806=EDGE_CURVE('',#11772,#11773,#7318,.T.);
#14807=EDGE_CURVE('',#11773,#11773,#9750,.T.);
#14808=EDGE_CURVE('',#11774,#11774,#9751,.T.);
#14809=EDGE_CURVE('',#11774,#11775,#7319,.T.);
#14810=EDGE_CURVE('',#11775,#11775,#9752,.T.);
#14811=EDGE_CURVE('',#11776,#11776,#9753,.T.);
#14812=EDGE_CURVE('',#11776,#11777,#7320,.T.);
#14813=EDGE_CURVE('',#11777,#11777,#9754,.T.);
#14814=EDGE_CURVE('',#11778,#11778,#9755,.T.);
#14815=EDGE_CURVE('',#11778,#11779,#7321,.T.);
#14816=EDGE_CURVE('',#11779,#11779,#9756,.T.);
#14817=EDGE_CURVE('',#11780,#11781,#7322,.T.);
#14818=EDGE_CURVE('',#11782,#11780,#7323,.T.);
#14819=EDGE_CURVE('',#11783,#11782,#7324,.T.);
#14820=EDGE_CURVE('',#11784,#11783,#7325,.T.);
#14821=EDGE_CURVE('',#11785,#11784,#7326,.T.);
#14822=EDGE_CURVE('',#11786,#11785,#7327,.T.);
#14823=EDGE_CURVE('',#11787,#11786,#7328,.T.);
#14824=EDGE_CURVE('',#11781,#11787,#7329,.T.);
#14825=EDGE_CURVE('',#11784,#11788,#7330,.T.);
#14826=EDGE_CURVE('',#11788,#11789,#7331,.T.);
#14827=EDGE_CURVE('',#11789,#11785,#7332,.T.);
#14828=EDGE_CURVE('',#11790,#11783,#7333,.T.);
#14829=EDGE_CURVE('',#11790,#11788,#7334,.T.);
#14830=EDGE_CURVE('',#11782,#11791,#7335,.T.);
#14831=EDGE_CURVE('',#11791,#11790,#7336,.T.);
#14832=EDGE_CURVE('',#11792,#11780,#7337,.T.);
#14833=EDGE_CURVE('',#11792,#11791,#7338,.T.);
#14834=EDGE_CURVE('',#11793,#11794,#7339,.T.);
#14835=EDGE_CURVE('',#11789,#11793,#7340,.T.);
#14836=EDGE_CURVE('',#11795,#11792,#7341,.T.);
#14837=EDGE_CURVE('',#11794,#11795,#7342,.T.);
#14838=EDGE_CURVE('',#11786,#11793,#7343,.T.);
#14839=EDGE_CURVE('',#11781,#11795,#7344,.T.);
#14840=EDGE_CURVE('',#11794,#11787,#7345,.T.);
#14841=EDGE_CURVE('',#11796,#11797,#7346,.T.);
#14842=EDGE_CURVE('',#11796,#11798,#7347,.T.);
#14843=EDGE_CURVE('',#11798,#11799,#7348,.T.);
#14844=EDGE_CURVE('',#11797,#11799,#7349,.T.);
#14845=EDGE_CURVE('',#11800,#11796,#7350,.T.);
#14846=EDGE_CURVE('',#11800,#11801,#7351,.T.);
#14847=EDGE_CURVE('',#11801,#11798,#7352,.T.);
#14848=EDGE_CURVE('',#11802,#11800,#7353,.T.);
#14849=EDGE_CURVE('',#11802,#11803,#7354,.T.);
#14850=EDGE_CURVE('',#11803,#11801,#7355,.T.);
#14851=EDGE_CURVE('',#11804,#11802,#7356,.T.);
#14852=EDGE_CURVE('',#11804,#11805,#7357,.T.);
#14853=EDGE_CURVE('',#11805,#11803,#7358,.T.);
#14854=EDGE_CURVE('',#11806,#11804,#7359,.T.);
#14855=EDGE_CURVE('',#11806,#11807,#7360,.T.);
#14856=EDGE_CURVE('',#11807,#11805,#7361,.T.);
#14857=EDGE_CURVE('',#11797,#11806,#7362,.T.);
#14858=EDGE_CURVE('',#11799,#11807,#7363,.T.);
#14859=EDGE_CURVE('',#11808,#11808,#9757,.T.);
#14860=EDGE_CURVE('',#11809,#11809,#9758,.T.);
#14861=EDGE_CURVE('',#11809,#11808,#7364,.T.);
#14862=EDGE_CURVE('',#11810,#11810,#9759,.F.);
#14863=EDGE_CURVE('',#11810,#11809,#7365,.T.);
#14864=EDGE_CURVE('',#11811,#11811,#9760,.T.);
#14865=EDGE_CURVE('',#11811,#11810,#7366,.T.);
#14866=EDGE_CURVE('',#11812,#11812,#9761,.T.);
#14867=EDGE_CURVE('',#11812,#11813,#7367,.T.);
#14868=EDGE_CURVE('',#11813,#11813,#9762,.T.);
#14869=EDGE_CURVE('',#11814,#11814,#9763,.T.);
#14870=EDGE_CURVE('',#11814,#11815,#7368,.T.);
#14871=EDGE_CURVE('',#11815,#11815,#9764,.T.);
#14872=EDGE_CURVE('',#11816,#11816,#9765,.T.);
#14873=EDGE_CURVE('',#11817,#11817,#9766,.T.);
#14874=EDGE_CURVE('',#11817,#11816,#7369,.T.);
#14875=EDGE_CURVE('',#11818,#11818,#9767,.T.);
#14876=EDGE_CURVE('',#11818,#11817,#7370,.T.);
#14877=EDGE_CURVE('',#11819,#11819,#9768,.T.);
#14878=EDGE_CURVE('',#11819,#11818,#7371,.T.);
#14879=EDGE_CURVE('',#11820,#11820,#9769,.T.);
#14880=EDGE_CURVE('',#11821,#11821,#9770,.F.);
#14881=EDGE_CURVE('',#11821,#11820,#7372,.T.);
#14882=EDGE_CURVE('',#11822,#11822,#9771,.F.);
#14883=EDGE_CURVE('',#11822,#11821,#7373,.T.);
#14884=EDGE_CURVE('',#11823,#11823,#9772,.T.);
#14885=EDGE_CURVE('',#11823,#11822,#7374,.T.);
#14886=EDGE_CURVE('',#11824,#11825,#7375,.T.);
#14887=EDGE_CURVE('',#11825,#11826,#7376,.T.);
#14888=EDGE_CURVE('',#11826,#11827,#7377,.T.);
#14889=EDGE_CURVE('',#11824,#11827,#7378,.T.);
#14890=EDGE_CURVE('',#11825,#11828,#7379,.T.);
#14891=EDGE_CURVE('',#11828,#11829,#7380,.T.);
#14892=EDGE_CURVE('',#11829,#11826,#7381,.T.);
#14893=EDGE_CURVE('',#11828,#11830,#7382,.T.);
#14894=EDGE_CURVE('',#11830,#11831,#7383,.T.);
#14895=EDGE_CURVE('',#11831,#11829,#7384,.T.);
#14896=EDGE_CURVE('',#11830,#11832,#7385,.T.);
#14897=EDGE_CURVE('',#11832,#11833,#7386,.T.);
#14898=EDGE_CURVE('',#11833,#11831,#7387,.T.);
#14899=EDGE_CURVE('',#11832,#11834,#7388,.T.);
#14900=EDGE_CURVE('',#11834,#11835,#7389,.T.);
#14901=EDGE_CURVE('',#11835,#11833,#7390,.T.);
#14902=EDGE_CURVE('',#11834,#11824,#7391,.T.);
#14903=EDGE_CURVE('',#11827,#11835,#7392,.T.);
#14904=ORIENTED_EDGE('',*,*,#11836,.F.);
#14905=ORIENTED_EDGE('',*,*,#11837,.T.);
#14906=ORIENTED_EDGE('',*,*,#11838,.F.);
#14907=ORIENTED_EDGE('',*,*,#11837,.F.);
#14908=ORIENTED_EDGE('',*,*,#11839,.F.);
#14909=ORIENTED_EDGE('',*,*,#11840,.T.);
#14910=ORIENTED_EDGE('',*,*,#11841,.F.);
#14911=ORIENTED_EDGE('',*,*,#11840,.F.);
#14912=ORIENTED_EDGE('',*,*,#11842,.F.);
#14913=ORIENTED_EDGE('',*,*,#11843,.T.);
#14914=ORIENTED_EDGE('',*,*,#11844,.F.);
#14915=ORIENTED_EDGE('',*,*,#11843,.F.);
#14916=ORIENTED_EDGE('',*,*,#11845,.F.);
#14917=ORIENTED_EDGE('',*,*,#11846,.T.);
#14918=ORIENTED_EDGE('',*,*,#11847,.F.);
#14919=ORIENTED_EDGE('',*,*,#11846,.F.);
#14920=ORIENTED_EDGE('',*,*,#11848,.F.);
#14921=ORIENTED_EDGE('',*,*,#11849,.T.);
#14922=ORIENTED_EDGE('',*,*,#11850,.F.);
#14923=ORIENTED_EDGE('',*,*,#11849,.F.);
#14924=ORIENTED_EDGE('',*,*,#11851,.F.);
#14925=ORIENTED_EDGE('',*,*,#11852,.T.);
#14926=ORIENTED_EDGE('',*,*,#11853,.F.);
#14927=ORIENTED_EDGE('',*,*,#11852,.F.);
#14928=ORIENTED_EDGE('',*,*,#11854,.F.);
#14929=ORIENTED_EDGE('',*,*,#11855,.T.);
#14930=ORIENTED_EDGE('',*,*,#11856,.F.);
#14931=ORIENTED_EDGE('',*,*,#11855,.F.);
#14932=ORIENTED_EDGE('',*,*,#11857,.F.);
#14933=ORIENTED_EDGE('',*,*,#11858,.T.);
#14934=ORIENTED_EDGE('',*,*,#11859,.F.);
#14935=ORIENTED_EDGE('',*,*,#11858,.F.);
#14936=ORIENTED_EDGE('',*,*,#11860,.F.);
#14937=ORIENTED_EDGE('',*,*,#11861,.T.);
#14938=ORIENTED_EDGE('',*,*,#11862,.F.);
#14939=ORIENTED_EDGE('',*,*,#11861,.F.);
#14940=ORIENTED_EDGE('',*,*,#11863,.F.);
#14941=ORIENTED_EDGE('',*,*,#11864,.T.);
#14942=ORIENTED_EDGE('',*,*,#11865,.F.);
#14943=ORIENTED_EDGE('',*,*,#11864,.F.);
#14944=ORIENTED_EDGE('',*,*,#11866,.T.);
#14945=ORIENTED_EDGE('',*,*,#11867,.T.);
#14946=ORIENTED_EDGE('',*,*,#11868,.F.);
#14947=ORIENTED_EDGE('',*,*,#11869,.F.);
#14948=ORIENTED_EDGE('',*,*,#11870,.T.);
#14949=ORIENTED_EDGE('',*,*,#11869,.T.);
#14950=ORIENTED_EDGE('',*,*,#11871,.F.);
#14951=ORIENTED_EDGE('',*,*,#11872,.F.);
#14952=ORIENTED_EDGE('',*,*,#11873,.T.);
#14953=ORIENTED_EDGE('',*,*,#11872,.T.);
#14954=ORIENTED_EDGE('',*,*,#11874,.F.);
#14955=ORIENTED_EDGE('',*,*,#11875,.F.);
#14956=ORIENTED_EDGE('',*,*,#11876,.T.);
#14957=ORIENTED_EDGE('',*,*,#11875,.T.);
#14958=ORIENTED_EDGE('',*,*,#11877,.F.);
#14959=ORIENTED_EDGE('',*,*,#11867,.F.);
#14960=ORIENTED_EDGE('',*,*,#11877,.T.);
#14961=ORIENTED_EDGE('',*,*,#11874,.T.);
#14962=ORIENTED_EDGE('',*,*,#11871,.T.);
#14963=ORIENTED_EDGE('',*,*,#11868,.T.);
#14964=ORIENTED_EDGE('',*,*,#11841,.T.);
#14965=ORIENTED_EDGE('',*,*,#11865,.T.);
#14966=ORIENTED_EDGE('',*,*,#11862,.T.);
#14967=ORIENTED_EDGE('',*,*,#11859,.T.);
#14968=ORIENTED_EDGE('',*,*,#11856,.T.);
#14969=ORIENTED_EDGE('',*,*,#11853,.T.);
#14970=ORIENTED_EDGE('',*,*,#11850,.T.);
#14971=ORIENTED_EDGE('',*,*,#11847,.T.);
#14972=ORIENTED_EDGE('',*,*,#11844,.T.);
#14973=ORIENTED_EDGE('',*,*,#11838,.T.);
#14974=ORIENTED_EDGE('',*,*,#11876,.F.);
#14975=ORIENTED_EDGE('',*,*,#11866,.F.);
#14976=ORIENTED_EDGE('',*,*,#11870,.F.);
#14977=ORIENTED_EDGE('',*,*,#11873,.F.);
#14978=ORIENTED_EDGE('',*,*,#11839,.T.);
#14979=ORIENTED_EDGE('',*,*,#11863,.T.);
#14980=ORIENTED_EDGE('',*,*,#11860,.T.);
#14981=ORIENTED_EDGE('',*,*,#11857,.T.);
#14982=ORIENTED_EDGE('',*,*,#11854,.T.);
#14983=ORIENTED_EDGE('',*,*,#11851,.T.);
#14984=ORIENTED_EDGE('',*,*,#11848,.T.);
#14985=ORIENTED_EDGE('',*,*,#11845,.T.);
#14986=ORIENTED_EDGE('',*,*,#11842,.T.);
#14987=ORIENTED_EDGE('',*,*,#11836,.T.);
#14988=ORIENTED_EDGE('',*,*,#11878,.T.);
#14989=ORIENTED_EDGE('',*,*,#11879,.T.);
#14990=ORIENTED_EDGE('',*,*,#11880,.F.);
#14991=ORIENTED_EDGE('',*,*,#11881,.F.);
#14992=ORIENTED_EDGE('',*,*,#11882,.T.);
#14993=ORIENTED_EDGE('',*,*,#11881,.T.);
#14994=ORIENTED_EDGE('',*,*,#11883,.F.);
#14995=ORIENTED_EDGE('',*,*,#11884,.F.);
#14996=ORIENTED_EDGE('',*,*,#11885,.T.);
#14997=ORIENTED_EDGE('',*,*,#11884,.T.);
#14998=ORIENTED_EDGE('',*,*,#11886,.F.);
#14999=ORIENTED_EDGE('',*,*,#11887,.F.);
#15000=ORIENTED_EDGE('',*,*,#11888,.T.);
#15001=ORIENTED_EDGE('',*,*,#11887,.T.);
#15002=ORIENTED_EDGE('',*,*,#11889,.F.);
#15003=ORIENTED_EDGE('',*,*,#11879,.F.);
#15004=ORIENTED_EDGE('',*,*,#11889,.T.);
#15005=ORIENTED_EDGE('',*,*,#11886,.T.);
#15006=ORIENTED_EDGE('',*,*,#11883,.T.);
#15007=ORIENTED_EDGE('',*,*,#11880,.T.);
#15008=ORIENTED_EDGE('',*,*,#11888,.F.);
#15009=ORIENTED_EDGE('',*,*,#11878,.F.);
#15010=ORIENTED_EDGE('',*,*,#11882,.F.);
#15011=ORIENTED_EDGE('',*,*,#11885,.F.);
#15012=ORIENTED_EDGE('',*,*,#11890,.T.);
#15013=ORIENTED_EDGE('',*,*,#11891,.T.);
#15014=ORIENTED_EDGE('',*,*,#11892,.F.);
#15015=ORIENTED_EDGE('',*,*,#11893,.F.);
#15016=ORIENTED_EDGE('',*,*,#11894,.T.);
#15017=ORIENTED_EDGE('',*,*,#11893,.T.);
#15018=ORIENTED_EDGE('',*,*,#11895,.F.);
#15019=ORIENTED_EDGE('',*,*,#11896,.F.);
#15020=ORIENTED_EDGE('',*,*,#11897,.T.);
#15021=ORIENTED_EDGE('',*,*,#11896,.T.);
#15022=ORIENTED_EDGE('',*,*,#11898,.F.);
#15023=ORIENTED_EDGE('',*,*,#11899,.F.);
#15024=ORIENTED_EDGE('',*,*,#11900,.T.);
#15025=ORIENTED_EDGE('',*,*,#11899,.T.);
#15026=ORIENTED_EDGE('',*,*,#11901,.F.);
#15027=ORIENTED_EDGE('',*,*,#11891,.F.);
#15028=ORIENTED_EDGE('',*,*,#11901,.T.);
#15029=ORIENTED_EDGE('',*,*,#11898,.T.);
#15030=ORIENTED_EDGE('',*,*,#11895,.T.);
#15031=ORIENTED_EDGE('',*,*,#11892,.T.);
#15032=ORIENTED_EDGE('',*,*,#11900,.F.);
#15033=ORIENTED_EDGE('',*,*,#11890,.F.);
#15034=ORIENTED_EDGE('',*,*,#11894,.F.);
#15035=ORIENTED_EDGE('',*,*,#11897,.F.);
#15036=ORIENTED_EDGE('',*,*,#11902,.F.);
#15037=ORIENTED_EDGE('',*,*,#11903,.F.);
#15038=ORIENTED_EDGE('',*,*,#11904,.T.);
#15039=ORIENTED_EDGE('',*,*,#11905,.F.);
#15040=ORIENTED_EDGE('',*,*,#11906,.F.);
#15041=ORIENTED_EDGE('',*,*,#11907,.F.);
#15042=ORIENTED_EDGE('',*,*,#11908,.T.);
#15043=ORIENTED_EDGE('',*,*,#11909,.F.);
#15044=ORIENTED_EDGE('',*,*,#11910,.F.);
#15045=ORIENTED_EDGE('',*,*,#11911,.T.);
#15046=ORIENTED_EDGE('',*,*,#11912,.F.);
#15047=ORIENTED_EDGE('',*,*,#11911,.F.);
#15048=ORIENTED_EDGE('',*,*,#11913,.F.);
#15049=ORIENTED_EDGE('',*,*,#11914,.T.);
#15050=ORIENTED_EDGE('',*,*,#11915,.F.);
#15051=ORIENTED_EDGE('',*,*,#11914,.F.);
#15052=ORIENTED_EDGE('',*,*,#11916,.F.);
#15053=ORIENTED_EDGE('',*,*,#11917,.T.);
#15054=ORIENTED_EDGE('',*,*,#11918,.F.);
#15055=ORIENTED_EDGE('',*,*,#11917,.F.);
#15056=ORIENTED_EDGE('',*,*,#11919,.F.);
#15057=ORIENTED_EDGE('',*,*,#11920,.T.);
#15058=ORIENTED_EDGE('',*,*,#11921,.F.);
#15059=ORIENTED_EDGE('',*,*,#11920,.F.);
#15060=ORIENTED_EDGE('',*,*,#11922,.F.);
#15061=ORIENTED_EDGE('',*,*,#11923,.T.);
#15062=ORIENTED_EDGE('',*,*,#11924,.F.);
#15063=ORIENTED_EDGE('',*,*,#11923,.F.);
#15064=ORIENTED_EDGE('',*,*,#11922,.T.);
#15065=ORIENTED_EDGE('',*,*,#11925,.F.);
#15066=ORIENTED_EDGE('',*,*,#11906,.T.);
#15067=ORIENTED_EDGE('',*,*,#11926,.F.);
#15068=ORIENTED_EDGE('',*,*,#11927,.F.);
#15069=ORIENTED_EDGE('',*,*,#11928,.F.);
#15070=ORIENTED_EDGE('',*,*,#11907,.T.);
#15071=ORIENTED_EDGE('',*,*,#11928,.T.);
#15072=ORIENTED_EDGE('',*,*,#11929,.F.);
#15073=ORIENTED_EDGE('',*,*,#11930,.F.);
#15074=ORIENTED_EDGE('',*,*,#11931,.T.);
#15075=ORIENTED_EDGE('',*,*,#11932,.F.);
#15076=ORIENTED_EDGE('',*,*,#11931,.F.);
#15077=ORIENTED_EDGE('',*,*,#11930,.T.);
#15078=ORIENTED_EDGE('',*,*,#11933,.F.);
#15079=ORIENTED_EDGE('',*,*,#11902,.T.);
#15080=ORIENTED_EDGE('',*,*,#11934,.F.);
#15081=ORIENTED_EDGE('',*,*,#11935,.F.);
#15082=ORIENTED_EDGE('',*,*,#11936,.F.);
#15083=ORIENTED_EDGE('',*,*,#11903,.T.);
#15084=ORIENTED_EDGE('',*,*,#11936,.T.);
#15085=ORIENTED_EDGE('',*,*,#11937,.F.);
#15086=ORIENTED_EDGE('',*,*,#11938,.T.);
#15087=ORIENTED_EDGE('',*,*,#11939,.T.);
#15088=ORIENTED_EDGE('',*,*,#11940,.T.);
#15089=ORIENTED_EDGE('',*,*,#11941,.T.);
#15090=ORIENTED_EDGE('',*,*,#11934,.T.);
#15091=ORIENTED_EDGE('',*,*,#11905,.T.);
#15092=ORIENTED_EDGE('',*,*,#11942,.T.);
#15093=ORIENTED_EDGE('',*,*,#11926,.T.);
#15094=ORIENTED_EDGE('',*,*,#11909,.T.);
#15095=ORIENTED_EDGE('',*,*,#11943,.T.);
#15096=ORIENTED_EDGE('',*,*,#11924,.T.);
#15097=ORIENTED_EDGE('',*,*,#11932,.T.);
#15098=ORIENTED_EDGE('',*,*,#11921,.T.);
#15099=ORIENTED_EDGE('',*,*,#11918,.T.);
#15100=ORIENTED_EDGE('',*,*,#11915,.T.);
#15101=ORIENTED_EDGE('',*,*,#11912,.T.);
#15102=ORIENTED_EDGE('',*,*,#11944,.F.);
#15103=ORIENTED_EDGE('',*,*,#11945,.T.);
#15104=ORIENTED_EDGE('',*,*,#11925,.T.);
#15105=ORIENTED_EDGE('',*,*,#11945,.F.);
#15106=ORIENTED_EDGE('',*,*,#11946,.F.);
#15107=ORIENTED_EDGE('',*,*,#11947,.T.);
#15108=ORIENTED_EDGE('',*,*,#11929,.T.);
#15109=ORIENTED_EDGE('',*,*,#11947,.F.);
#15110=ORIENTED_EDGE('',*,*,#11948,.F.);
#15111=ORIENTED_EDGE('',*,*,#11949,.T.);
#15112=ORIENTED_EDGE('',*,*,#11933,.T.);
#15113=ORIENTED_EDGE('',*,*,#11949,.F.);
#15114=ORIENTED_EDGE('',*,*,#11950,.F.);
#15115=ORIENTED_EDGE('',*,*,#11951,.T.);
#15116=ORIENTED_EDGE('',*,*,#11937,.T.);
#15117=ORIENTED_EDGE('',*,*,#11951,.F.);
#15118=ORIENTED_EDGE('',*,*,#11952,.T.);
#15119=ORIENTED_EDGE('',*,*,#11953,.T.);
#15120=ORIENTED_EDGE('',*,*,#11943,.F.);
#15121=ORIENTED_EDGE('',*,*,#11908,.F.);
#15122=ORIENTED_EDGE('',*,*,#11927,.T.);
#15123=ORIENTED_EDGE('',*,*,#11942,.F.);
#15124=ORIENTED_EDGE('',*,*,#11904,.F.);
#15125=ORIENTED_EDGE('',*,*,#11935,.T.);
#15126=ORIENTED_EDGE('',*,*,#11941,.F.);
#15127=ORIENTED_EDGE('',*,*,#11954,.F.);
#15128=ORIENTED_EDGE('',*,*,#11955,.T.);
#15129=ORIENTED_EDGE('',*,*,#11954,.T.);
#15130=ORIENTED_EDGE('',*,*,#11940,.F.);
#15131=ORIENTED_EDGE('',*,*,#11956,.F.);
#15132=ORIENTED_EDGE('',*,*,#11957,.T.);
#15133=ORIENTED_EDGE('',*,*,#11956,.T.);
#15134=ORIENTED_EDGE('',*,*,#11939,.F.);
#15135=ORIENTED_EDGE('',*,*,#11958,.F.);
#15136=ORIENTED_EDGE('',*,*,#11959,.T.);
#15137=ORIENTED_EDGE('',*,*,#11958,.T.);
#15138=ORIENTED_EDGE('',*,*,#11938,.F.);
#15139=ORIENTED_EDGE('',*,*,#11953,.F.);
#15140=ORIENTED_EDGE('',*,*,#11959,.F.);
#15141=ORIENTED_EDGE('',*,*,#11952,.F.);
#15142=ORIENTED_EDGE('',*,*,#11955,.F.);
#15143=ORIENTED_EDGE('',*,*,#11957,.F.);
#15144=ORIENTED_EDGE('',*,*,#11950,.T.);
#15145=ORIENTED_EDGE('',*,*,#11948,.T.);
#15146=ORIENTED_EDGE('',*,*,#11946,.T.);
#15147=ORIENTED_EDGE('',*,*,#11944,.T.);
#15148=ORIENTED_EDGE('',*,*,#11919,.T.);
#15149=ORIENTED_EDGE('',*,*,#11916,.T.);
#15150=ORIENTED_EDGE('',*,*,#11913,.T.);
#15151=ORIENTED_EDGE('',*,*,#11910,.T.);
#15152=ORIENTED_EDGE('',*,*,#11960,.F.);
#15153=ORIENTED_EDGE('',*,*,#11961,.T.);
#15154=ORIENTED_EDGE('',*,*,#11962,.F.);
#15155=ORIENTED_EDGE('',*,*,#11961,.F.);
#15156=ORIENTED_EDGE('',*,*,#11963,.F.);
#15157=ORIENTED_EDGE('',*,*,#11964,.T.);
#15158=ORIENTED_EDGE('',*,*,#11965,.F.);
#15159=ORIENTED_EDGE('',*,*,#11964,.F.);
#15160=ORIENTED_EDGE('',*,*,#11966,.F.);
#15161=ORIENTED_EDGE('',*,*,#11967,.T.);
#15162=ORIENTED_EDGE('',*,*,#11968,.F.);
#15163=ORIENTED_EDGE('',*,*,#11967,.F.);
#15164=ORIENTED_EDGE('',*,*,#11969,.F.);
#15165=ORIENTED_EDGE('',*,*,#11970,.T.);
#15166=ORIENTED_EDGE('',*,*,#11971,.T.);
#15167=ORIENTED_EDGE('',*,*,#11970,.F.);
#15168=ORIENTED_EDGE('',*,*,#11971,.F.);
#15169=ORIENTED_EDGE('',*,*,#11972,.F.);
#15170=ORIENTED_EDGE('',*,*,#11972,.T.);
#15171=ORIENTED_EDGE('',*,*,#11973,.T.);
#15172=ORIENTED_EDGE('',*,*,#11974,.F.);
#15173=ORIENTED_EDGE('',*,*,#11973,.F.);
#15174=ORIENTED_EDGE('',*,*,#11975,.F.);
#15175=ORIENTED_EDGE('',*,*,#11976,.T.);
#15176=ORIENTED_EDGE('',*,*,#11977,.T.);
#15177=ORIENTED_EDGE('',*,*,#11976,.F.);
#15178=ORIENTED_EDGE('',*,*,#11977,.F.);
#15179=ORIENTED_EDGE('',*,*,#11978,.F.);
#15180=ORIENTED_EDGE('',*,*,#11979,.T.);
#15181=ORIENTED_EDGE('',*,*,#11980,.T.);
#15182=ORIENTED_EDGE('',*,*,#11979,.F.);
#15183=ORIENTED_EDGE('',*,*,#11980,.F.);
#15184=ORIENTED_EDGE('',*,*,#11981,.T.);
#15185=ORIENTED_EDGE('',*,*,#11982,.T.);
#15186=ORIENTED_EDGE('',*,*,#11983,.F.);
#15187=ORIENTED_EDGE('',*,*,#11984,.F.);
#15188=ORIENTED_EDGE('',*,*,#11985,.T.);
#15189=ORIENTED_EDGE('',*,*,#11984,.T.);
#15190=ORIENTED_EDGE('',*,*,#11986,.F.);
#15191=ORIENTED_EDGE('',*,*,#11987,.F.);
#15192=ORIENTED_EDGE('',*,*,#11962,.T.);
#15193=ORIENTED_EDGE('',*,*,#11965,.T.);
#15194=ORIENTED_EDGE('',*,*,#11968,.T.);
#15195=ORIENTED_EDGE('',*,*,#11974,.T.);
#15196=ORIENTED_EDGE('',*,*,#11988,.T.);
#15197=ORIENTED_EDGE('',*,*,#11987,.T.);
#15198=ORIENTED_EDGE('',*,*,#11989,.F.);
#15199=ORIENTED_EDGE('',*,*,#11990,.F.);
#15200=ORIENTED_EDGE('',*,*,#11991,.T.);
#15201=ORIENTED_EDGE('',*,*,#11990,.T.);
#15202=ORIENTED_EDGE('',*,*,#11992,.F.);
#15203=ORIENTED_EDGE('',*,*,#11982,.F.);
#15204=ORIENTED_EDGE('',*,*,#11960,.T.);
#15205=ORIENTED_EDGE('',*,*,#11963,.T.);
#15206=ORIENTED_EDGE('',*,*,#11966,.T.);
#15207=ORIENTED_EDGE('',*,*,#11969,.T.);
#15208=ORIENTED_EDGE('',*,*,#11992,.T.);
#15209=ORIENTED_EDGE('',*,*,#11989,.T.);
#15210=ORIENTED_EDGE('',*,*,#11986,.T.);
#15211=ORIENTED_EDGE('',*,*,#11983,.T.);
#15212=ORIENTED_EDGE('',*,*,#11991,.F.);
#15213=ORIENTED_EDGE('',*,*,#11981,.F.);
#15214=ORIENTED_EDGE('',*,*,#11985,.F.);
#15215=ORIENTED_EDGE('',*,*,#11988,.F.);
#15216=ORIENTED_EDGE('',*,*,#11975,.T.);
#15217=ORIENTED_EDGE('',*,*,#11978,.T.);
#15218=ORIENTED_EDGE('',*,*,#11993,.F.);
#15219=ORIENTED_EDGE('',*,*,#11994,.T.);
#15220=ORIENTED_EDGE('',*,*,#11995,.F.);
#15221=ORIENTED_EDGE('',*,*,#11994,.F.);
#15222=ORIENTED_EDGE('',*,*,#11996,.F.);
#15223=ORIENTED_EDGE('',*,*,#11997,.T.);
#15224=ORIENTED_EDGE('',*,*,#11998,.F.);
#15225=ORIENTED_EDGE('',*,*,#11997,.F.);
#15226=ORIENTED_EDGE('',*,*,#11999,.F.);
#15227=ORIENTED_EDGE('',*,*,#12000,.T.);
#15228=ORIENTED_EDGE('',*,*,#12001,.F.);
#15229=ORIENTED_EDGE('',*,*,#12000,.F.);
#15230=ORIENTED_EDGE('',*,*,#12002,.F.);
#15231=ORIENTED_EDGE('',*,*,#12003,.T.);
#15232=ORIENTED_EDGE('',*,*,#12004,.F.);
#15233=ORIENTED_EDGE('',*,*,#12003,.F.);
#15234=ORIENTED_EDGE('',*,*,#12002,.T.);
#15235=ORIENTED_EDGE('',*,*,#12005,.T.);
#15236=ORIENTED_EDGE('',*,*,#12005,.F.);
#15237=ORIENTED_EDGE('',*,*,#12006,.T.);
#15238=ORIENTED_EDGE('',*,*,#12007,.T.);
#15239=ORIENTED_EDGE('',*,*,#12006,.F.);
#15240=ORIENTED_EDGE('',*,*,#12008,.F.);
#15241=ORIENTED_EDGE('',*,*,#12009,.T.);
#15242=ORIENTED_EDGE('',*,*,#12010,.T.);
#15243=ORIENTED_EDGE('',*,*,#12009,.F.);
#15244=ORIENTED_EDGE('',*,*,#12008,.T.);
#15245=ORIENTED_EDGE('',*,*,#11995,.T.);
#15246=ORIENTED_EDGE('',*,*,#11998,.T.);
#15247=ORIENTED_EDGE('',*,*,#12001,.T.);
#15248=ORIENTED_EDGE('',*,*,#12004,.T.);
#15249=ORIENTED_EDGE('',*,*,#12010,.F.);
#15250=ORIENTED_EDGE('',*,*,#11993,.T.);
#15251=ORIENTED_EDGE('',*,*,#11996,.T.);
#15252=ORIENTED_EDGE('',*,*,#11999,.T.);
#15253=ORIENTED_EDGE('',*,*,#12007,.F.);
#15254=ORIENTED_EDGE('',*,*,#12011,.F.);
#15255=ORIENTED_EDGE('',*,*,#12012,.T.);
#15256=ORIENTED_EDGE('',*,*,#12013,.F.);
#15257=ORIENTED_EDGE('',*,*,#12012,.F.);
#15258=ORIENTED_EDGE('',*,*,#12014,.F.);
#15259=ORIENTED_EDGE('',*,*,#12015,.T.);
#15260=ORIENTED_EDGE('',*,*,#12016,.F.);
#15261=ORIENTED_EDGE('',*,*,#12015,.F.);
#15262=ORIENTED_EDGE('',*,*,#12017,.F.);
#15263=ORIENTED_EDGE('',*,*,#12018,.T.);
#15264=ORIENTED_EDGE('',*,*,#12019,.F.);
#15265=ORIENTED_EDGE('',*,*,#12018,.F.);
#15266=ORIENTED_EDGE('',*,*,#12020,.F.);
#15267=ORIENTED_EDGE('',*,*,#12021,.T.);
#15268=ORIENTED_EDGE('',*,*,#12022,.F.);
#15269=ORIENTED_EDGE('',*,*,#12021,.F.);
#15270=ORIENTED_EDGE('',*,*,#12020,.T.);
#15271=ORIENTED_EDGE('',*,*,#12023,.F.);
#15272=ORIENTED_EDGE('',*,*,#12024,.F.);
#15273=ORIENTED_EDGE('',*,*,#12025,.T.);
#15274=ORIENTED_EDGE('',*,*,#12023,.T.);
#15275=ORIENTED_EDGE('',*,*,#12025,.F.);
#15276=ORIENTED_EDGE('',*,*,#12026,.F.);
#15277=ORIENTED_EDGE('',*,*,#12027,.T.);
#15278=ORIENTED_EDGE('',*,*,#12028,.T.);
#15279=ORIENTED_EDGE('',*,*,#12027,.F.);
#15280=ORIENTED_EDGE('',*,*,#12028,.F.);
#15281=ORIENTED_EDGE('',*,*,#12029,.F.);
#15282=ORIENTED_EDGE('',*,*,#12030,.T.);
#15283=ORIENTED_EDGE('',*,*,#12031,.T.);
#15284=ORIENTED_EDGE('',*,*,#12030,.F.);
#15285=ORIENTED_EDGE('',*,*,#12031,.F.);
#15286=ORIENTED_EDGE('',*,*,#12032,.T.);
#15287=ORIENTED_EDGE('',*,*,#12033,.T.);
#15288=ORIENTED_EDGE('',*,*,#12034,.F.);
#15289=ORIENTED_EDGE('',*,*,#12035,.F.);
#15290=ORIENTED_EDGE('',*,*,#12036,.T.);
#15291=ORIENTED_EDGE('',*,*,#12035,.T.);
#15292=ORIENTED_EDGE('',*,*,#12037,.F.);
#15293=ORIENTED_EDGE('',*,*,#12038,.F.);
#15294=ORIENTED_EDGE('',*,*,#12013,.T.);
#15295=ORIENTED_EDGE('',*,*,#12016,.T.);
#15296=ORIENTED_EDGE('',*,*,#12019,.T.);
#15297=ORIENTED_EDGE('',*,*,#12022,.T.);
#15298=ORIENTED_EDGE('',*,*,#12039,.T.);
#15299=ORIENTED_EDGE('',*,*,#12038,.T.);
#15300=ORIENTED_EDGE('',*,*,#12040,.F.);
#15301=ORIENTED_EDGE('',*,*,#12041,.F.);
#15302=ORIENTED_EDGE('',*,*,#12042,.T.);
#15303=ORIENTED_EDGE('',*,*,#12041,.T.);
#15304=ORIENTED_EDGE('',*,*,#12043,.F.);
#15305=ORIENTED_EDGE('',*,*,#12033,.F.);
#15306=ORIENTED_EDGE('',*,*,#12011,.T.);
#15307=ORIENTED_EDGE('',*,*,#12014,.T.);
#15308=ORIENTED_EDGE('',*,*,#12017,.T.);
#15309=ORIENTED_EDGE('',*,*,#12024,.T.);
#15310=ORIENTED_EDGE('',*,*,#12043,.T.);
#15311=ORIENTED_EDGE('',*,*,#12040,.T.);
#15312=ORIENTED_EDGE('',*,*,#12037,.T.);
#15313=ORIENTED_EDGE('',*,*,#12034,.T.);
#15314=ORIENTED_EDGE('',*,*,#12042,.F.);
#15315=ORIENTED_EDGE('',*,*,#12032,.F.);
#15316=ORIENTED_EDGE('',*,*,#12036,.F.);
#15317=ORIENTED_EDGE('',*,*,#12039,.F.);
#15318=ORIENTED_EDGE('',*,*,#12026,.T.);
#15319=ORIENTED_EDGE('',*,*,#12029,.T.);
#15320=ORIENTED_EDGE('',*,*,#12044,.F.);
#15321=ORIENTED_EDGE('',*,*,#12045,.T.);
#15322=ORIENTED_EDGE('',*,*,#12046,.F.);
#15323=ORIENTED_EDGE('',*,*,#12045,.F.);
#15324=ORIENTED_EDGE('',*,*,#12047,.F.);
#15325=ORIENTED_EDGE('',*,*,#12048,.T.);
#15326=ORIENTED_EDGE('',*,*,#12049,.F.);
#15327=ORIENTED_EDGE('',*,*,#12048,.F.);
#15328=ORIENTED_EDGE('',*,*,#12050,.F.);
#15329=ORIENTED_EDGE('',*,*,#12051,.T.);
#15330=ORIENTED_EDGE('',*,*,#12052,.F.);
#15331=ORIENTED_EDGE('',*,*,#12051,.F.);
#15332=ORIENTED_EDGE('',*,*,#12053,.F.);
#15333=ORIENTED_EDGE('',*,*,#12054,.F.);
#15334=ORIENTED_EDGE('',*,*,#12055,.F.);
#15335=ORIENTED_EDGE('',*,*,#12056,.F.);
#15336=ORIENTED_EDGE('',*,*,#12054,.T.);
#15337=ORIENTED_EDGE('',*,*,#12057,.F.);
#15338=ORIENTED_EDGE('',*,*,#12044,.T.);
#15339=ORIENTED_EDGE('',*,*,#12047,.T.);
#15340=ORIENTED_EDGE('',*,*,#12050,.T.);
#15341=ORIENTED_EDGE('',*,*,#12058,.T.);
#15342=ORIENTED_EDGE('',*,*,#12055,.T.);
#15343=ORIENTED_EDGE('',*,*,#12057,.T.);
#15344=ORIENTED_EDGE('',*,*,#12053,.T.);
#15345=ORIENTED_EDGE('',*,*,#12059,.F.);
#15346=ORIENTED_EDGE('',*,*,#12058,.F.);
#15347=ORIENTED_EDGE('',*,*,#12060,.T.);
#15348=ORIENTED_EDGE('',*,*,#12061,.T.);
#15349=ORIENTED_EDGE('',*,*,#12060,.F.);
#15350=ORIENTED_EDGE('',*,*,#12061,.F.);
#15351=ORIENTED_EDGE('',*,*,#12062,.F.);
#15352=ORIENTED_EDGE('',*,*,#12063,.F.);
#15353=ORIENTED_EDGE('',*,*,#12064,.T.);
#15354=ORIENTED_EDGE('',*,*,#12062,.T.);
#15355=ORIENTED_EDGE('',*,*,#12064,.F.);
#15356=ORIENTED_EDGE('',*,*,#12056,.T.);
#15357=ORIENTED_EDGE('',*,*,#12059,.T.);
#15358=ORIENTED_EDGE('',*,*,#12046,.T.);
#15359=ORIENTED_EDGE('',*,*,#12049,.T.);
#15360=ORIENTED_EDGE('',*,*,#12052,.T.);
#15361=ORIENTED_EDGE('',*,*,#12063,.T.);
#15362=ORIENTED_EDGE('',*,*,#12065,.F.);
#15363=ORIENTED_EDGE('',*,*,#12066,.T.);
#15364=ORIENTED_EDGE('',*,*,#12067,.F.);
#15365=ORIENTED_EDGE('',*,*,#12066,.F.);
#15366=ORIENTED_EDGE('',*,*,#12065,.T.);
#15367=ORIENTED_EDGE('',*,*,#12068,.F.);
#15368=ORIENTED_EDGE('',*,*,#12069,.F.);
#15369=ORIENTED_EDGE('',*,*,#12070,.T.);
#15370=ORIENTED_EDGE('',*,*,#12068,.T.);
#15371=ORIENTED_EDGE('',*,*,#12070,.F.);
#15372=ORIENTED_EDGE('',*,*,#12071,.T.);
#15373=ORIENTED_EDGE('',*,*,#12072,.T.);
#15374=ORIENTED_EDGE('',*,*,#12073,.F.);
#15375=ORIENTED_EDGE('',*,*,#12074,.F.);
#15376=ORIENTED_EDGE('',*,*,#12075,.T.);
#15377=ORIENTED_EDGE('',*,*,#12074,.T.);
#15378=ORIENTED_EDGE('',*,*,#12076,.F.);
#15379=ORIENTED_EDGE('',*,*,#12077,.F.);
#15380=ORIENTED_EDGE('',*,*,#12078,.T.);
#15381=ORIENTED_EDGE('',*,*,#12077,.T.);
#15382=ORIENTED_EDGE('',*,*,#12079,.F.);
#15383=ORIENTED_EDGE('',*,*,#12080,.F.);
#15384=ORIENTED_EDGE('',*,*,#12081,.T.);
#15385=ORIENTED_EDGE('',*,*,#12080,.T.);
#15386=ORIENTED_EDGE('',*,*,#12082,.F.);
#15387=ORIENTED_EDGE('',*,*,#12072,.F.);
#15388=ORIENTED_EDGE('',*,*,#12082,.T.);
#15389=ORIENTED_EDGE('',*,*,#12079,.T.);
#15390=ORIENTED_EDGE('',*,*,#12076,.T.);
#15391=ORIENTED_EDGE('',*,*,#12073,.T.);
#15392=ORIENTED_EDGE('',*,*,#12067,.T.);
#15393=ORIENTED_EDGE('',*,*,#12081,.F.);
#15394=ORIENTED_EDGE('',*,*,#12071,.F.);
#15395=ORIENTED_EDGE('',*,*,#12075,.F.);
#15396=ORIENTED_EDGE('',*,*,#12078,.F.);
#15397=ORIENTED_EDGE('',*,*,#12069,.T.);
#15398=ORIENTED_EDGE('',*,*,#12083,.F.);
#15399=ORIENTED_EDGE('',*,*,#12084,.T.);
#15400=ORIENTED_EDGE('',*,*,#12085,.F.);
#15401=ORIENTED_EDGE('',*,*,#12084,.F.);
#15402=ORIENTED_EDGE('',*,*,#12083,.T.);
#15403=ORIENTED_EDGE('',*,*,#12086,.F.);
#15404=ORIENTED_EDGE('',*,*,#12087,.F.);
#15405=ORIENTED_EDGE('',*,*,#12088,.T.);
#15406=ORIENTED_EDGE('',*,*,#12086,.T.);
#15407=ORIENTED_EDGE('',*,*,#12088,.F.);
#15408=ORIENTED_EDGE('',*,*,#12089,.T.);
#15409=ORIENTED_EDGE('',*,*,#12090,.T.);
#15410=ORIENTED_EDGE('',*,*,#12091,.F.);
#15411=ORIENTED_EDGE('',*,*,#12092,.F.);
#15412=ORIENTED_EDGE('',*,*,#12093,.T.);
#15413=ORIENTED_EDGE('',*,*,#12092,.T.);
#15414=ORIENTED_EDGE('',*,*,#12094,.F.);
#15415=ORIENTED_EDGE('',*,*,#12095,.F.);
#15416=ORIENTED_EDGE('',*,*,#12096,.T.);
#15417=ORIENTED_EDGE('',*,*,#12095,.T.);
#15418=ORIENTED_EDGE('',*,*,#12097,.F.);
#15419=ORIENTED_EDGE('',*,*,#12098,.F.);
#15420=ORIENTED_EDGE('',*,*,#12099,.T.);
#15421=ORIENTED_EDGE('',*,*,#12098,.T.);
#15422=ORIENTED_EDGE('',*,*,#12100,.F.);
#15423=ORIENTED_EDGE('',*,*,#12090,.F.);
#15424=ORIENTED_EDGE('',*,*,#12100,.T.);
#15425=ORIENTED_EDGE('',*,*,#12097,.T.);
#15426=ORIENTED_EDGE('',*,*,#12094,.T.);
#15427=ORIENTED_EDGE('',*,*,#12091,.T.);
#15428=ORIENTED_EDGE('',*,*,#12085,.T.);
#15429=ORIENTED_EDGE('',*,*,#12099,.F.);
#15430=ORIENTED_EDGE('',*,*,#12089,.F.);
#15431=ORIENTED_EDGE('',*,*,#12093,.F.);
#15432=ORIENTED_EDGE('',*,*,#12096,.F.);
#15433=ORIENTED_EDGE('',*,*,#12087,.T.);
#15434=ORIENTED_EDGE('',*,*,#12101,.F.);
#15435=ORIENTED_EDGE('',*,*,#12102,.T.);
#15436=ORIENTED_EDGE('',*,*,#12103,.F.);
#15437=ORIENTED_EDGE('',*,*,#12102,.F.);
#15438=ORIENTED_EDGE('',*,*,#12101,.T.);
#15439=ORIENTED_EDGE('',*,*,#12104,.F.);
#15440=ORIENTED_EDGE('',*,*,#12105,.F.);
#15441=ORIENTED_EDGE('',*,*,#12106,.T.);
#15442=ORIENTED_EDGE('',*,*,#12107,.F.);
#15443=ORIENTED_EDGE('',*,*,#12106,.F.);
#15444=ORIENTED_EDGE('',*,*,#12105,.T.);
#15445=ORIENTED_EDGE('',*,*,#12108,.F.);
#15446=ORIENTED_EDGE('',*,*,#12109,.F.);
#15447=ORIENTED_EDGE('',*,*,#12110,.T.);
#15448=ORIENTED_EDGE('',*,*,#12111,.F.);
#15449=ORIENTED_EDGE('',*,*,#12110,.F.);
#15450=ORIENTED_EDGE('',*,*,#12109,.T.);
#15451=ORIENTED_EDGE('',*,*,#12112,.F.);
#15452=ORIENTED_EDGE('',*,*,#12113,.F.);
#15453=ORIENTED_EDGE('',*,*,#12114,.T.);
#15454=ORIENTED_EDGE('',*,*,#12115,.F.);
#15455=ORIENTED_EDGE('',*,*,#12114,.F.);
#15456=ORIENTED_EDGE('',*,*,#12113,.T.);
#15457=ORIENTED_EDGE('',*,*,#12116,.F.);
#15458=ORIENTED_EDGE('',*,*,#12117,.F.);
#15459=ORIENTED_EDGE('',*,*,#12118,.T.);
#15460=ORIENTED_EDGE('',*,*,#12104,.T.);
#15461=ORIENTED_EDGE('',*,*,#12118,.F.);
#15462=ORIENTED_EDGE('',*,*,#12119,.F.);
#15463=ORIENTED_EDGE('',*,*,#12120,.T.);
#15464=ORIENTED_EDGE('',*,*,#12108,.T.);
#15465=ORIENTED_EDGE('',*,*,#12120,.F.);
#15466=ORIENTED_EDGE('',*,*,#12121,.F.);
#15467=ORIENTED_EDGE('',*,*,#12122,.T.);
#15468=ORIENTED_EDGE('',*,*,#12112,.T.);
#15469=ORIENTED_EDGE('',*,*,#12122,.F.);
#15470=ORIENTED_EDGE('',*,*,#12123,.F.);
#15471=ORIENTED_EDGE('',*,*,#12124,.T.);
#15472=ORIENTED_EDGE('',*,*,#12116,.T.);
#15473=ORIENTED_EDGE('',*,*,#12124,.F.);
#15474=ORIENTED_EDGE('',*,*,#12125,.T.);
#15475=ORIENTED_EDGE('',*,*,#12126,.T.);
#15476=ORIENTED_EDGE('',*,*,#12127,.F.);
#15477=ORIENTED_EDGE('',*,*,#12128,.F.);
#15478=ORIENTED_EDGE('',*,*,#12129,.T.);
#15479=ORIENTED_EDGE('',*,*,#12128,.T.);
#15480=ORIENTED_EDGE('',*,*,#12130,.F.);
#15481=ORIENTED_EDGE('',*,*,#12131,.F.);
#15482=ORIENTED_EDGE('',*,*,#12132,.T.);
#15483=ORIENTED_EDGE('',*,*,#12131,.T.);
#15484=ORIENTED_EDGE('',*,*,#12133,.F.);
#15485=ORIENTED_EDGE('',*,*,#12134,.F.);
#15486=ORIENTED_EDGE('',*,*,#12135,.T.);
#15487=ORIENTED_EDGE('',*,*,#12134,.T.);
#15488=ORIENTED_EDGE('',*,*,#12136,.F.);
#15489=ORIENTED_EDGE('',*,*,#12137,.F.);
#15490=ORIENTED_EDGE('',*,*,#12138,.T.);
#15491=ORIENTED_EDGE('',*,*,#12137,.T.);
#15492=ORIENTED_EDGE('',*,*,#12139,.F.);
#15493=ORIENTED_EDGE('',*,*,#12140,.F.);
#15494=ORIENTED_EDGE('',*,*,#12115,.T.);
#15495=ORIENTED_EDGE('',*,*,#12111,.T.);
#15496=ORIENTED_EDGE('',*,*,#12107,.T.);
#15497=ORIENTED_EDGE('',*,*,#12103,.T.);
#15498=ORIENTED_EDGE('',*,*,#12141,.T.);
#15499=ORIENTED_EDGE('',*,*,#12140,.T.);
#15500=ORIENTED_EDGE('',*,*,#12142,.F.);
#15501=ORIENTED_EDGE('',*,*,#12143,.F.);
#15502=ORIENTED_EDGE('',*,*,#12144,.T.);
#15503=ORIENTED_EDGE('',*,*,#12143,.T.);
#15504=ORIENTED_EDGE('',*,*,#12145,.F.);
#15505=ORIENTED_EDGE('',*,*,#12146,.F.);
#15506=ORIENTED_EDGE('',*,*,#12147,.T.);
#15507=ORIENTED_EDGE('',*,*,#12146,.T.);
#15508=ORIENTED_EDGE('',*,*,#12148,.F.);
#15509=ORIENTED_EDGE('',*,*,#12149,.F.);
#15510=ORIENTED_EDGE('',*,*,#12150,.T.);
#15511=ORIENTED_EDGE('',*,*,#12149,.T.);
#15512=ORIENTED_EDGE('',*,*,#12151,.F.);
#15513=ORIENTED_EDGE('',*,*,#12152,.F.);
#15514=ORIENTED_EDGE('',*,*,#12153,.T.);
#15515=ORIENTED_EDGE('',*,*,#12152,.T.);
#15516=ORIENTED_EDGE('',*,*,#12154,.F.);
#15517=ORIENTED_EDGE('',*,*,#12155,.F.);
#15518=ORIENTED_EDGE('',*,*,#12156,.T.);
#15519=ORIENTED_EDGE('',*,*,#12155,.T.);
#15520=ORIENTED_EDGE('',*,*,#12157,.F.);
#15521=ORIENTED_EDGE('',*,*,#12158,.F.);
#15522=ORIENTED_EDGE('',*,*,#12117,.T.);
#15523=ORIENTED_EDGE('',*,*,#12119,.T.);
#15524=ORIENTED_EDGE('',*,*,#12121,.T.);
#15525=ORIENTED_EDGE('',*,*,#12123,.T.);
#15526=ORIENTED_EDGE('',*,*,#12159,.T.);
#15527=ORIENTED_EDGE('',*,*,#12158,.T.);
#15528=ORIENTED_EDGE('',*,*,#12160,.F.);
#15529=ORIENTED_EDGE('',*,*,#12126,.F.);
#15530=ORIENTED_EDGE('',*,*,#12160,.T.);
#15531=ORIENTED_EDGE('',*,*,#12157,.T.);
#15532=ORIENTED_EDGE('',*,*,#12154,.T.);
#15533=ORIENTED_EDGE('',*,*,#12151,.T.);
#15534=ORIENTED_EDGE('',*,*,#12148,.T.);
#15535=ORIENTED_EDGE('',*,*,#12145,.T.);
#15536=ORIENTED_EDGE('',*,*,#12142,.T.);
#15537=ORIENTED_EDGE('',*,*,#12139,.T.);
#15538=ORIENTED_EDGE('',*,*,#12136,.T.);
#15539=ORIENTED_EDGE('',*,*,#12133,.T.);
#15540=ORIENTED_EDGE('',*,*,#12130,.T.);
#15541=ORIENTED_EDGE('',*,*,#12127,.T.);
#15542=ORIENTED_EDGE('',*,*,#12159,.F.);
#15543=ORIENTED_EDGE('',*,*,#12125,.F.);
#15544=ORIENTED_EDGE('',*,*,#12129,.F.);
#15545=ORIENTED_EDGE('',*,*,#12132,.F.);
#15546=ORIENTED_EDGE('',*,*,#12135,.F.);
#15547=ORIENTED_EDGE('',*,*,#12138,.F.);
#15548=ORIENTED_EDGE('',*,*,#12141,.F.);
#15549=ORIENTED_EDGE('',*,*,#12144,.F.);
#15550=ORIENTED_EDGE('',*,*,#12147,.F.);
#15551=ORIENTED_EDGE('',*,*,#12150,.F.);
#15552=ORIENTED_EDGE('',*,*,#12153,.F.);
#15553=ORIENTED_EDGE('',*,*,#12156,.F.);
#15554=ORIENTED_EDGE('',*,*,#12161,.F.);
#15555=ORIENTED_EDGE('',*,*,#12162,.F.);
#15556=ORIENTED_EDGE('',*,*,#12163,.T.);
#15557=ORIENTED_EDGE('',*,*,#12164,.F.);
#15558=ORIENTED_EDGE('',*,*,#12165,.F.);
#15559=ORIENTED_EDGE('',*,*,#12163,.F.);
#15560=ORIENTED_EDGE('',*,*,#12164,.T.);
#15561=ORIENTED_EDGE('',*,*,#12165,.T.);
#15562=ORIENTED_EDGE('',*,*,#12166,.T.);
#15563=ORIENTED_EDGE('',*,*,#12167,.T.);
#15564=ORIENTED_EDGE('',*,*,#12166,.F.);
#15565=ORIENTED_EDGE('',*,*,#12168,.T.);
#15566=ORIENTED_EDGE('',*,*,#12169,.T.);
#15567=ORIENTED_EDGE('',*,*,#12170,.F.);
#15568=ORIENTED_EDGE('',*,*,#12169,.F.);
#15569=ORIENTED_EDGE('',*,*,#12170,.T.);
#15570=ORIENTED_EDGE('',*,*,#12171,.T.);
#15571=ORIENTED_EDGE('',*,*,#12172,.F.);
#15572=ORIENTED_EDGE('',*,*,#12171,.F.);
#15573=ORIENTED_EDGE('',*,*,#12167,.F.);
#15574=ORIENTED_EDGE('',*,*,#12172,.T.);
#15575=ORIENTED_EDGE('',*,*,#12173,.F.);
#15576=ORIENTED_EDGE('',*,*,#12174,.T.);
#15577=ORIENTED_EDGE('',*,*,#12161,.T.);
#15578=ORIENTED_EDGE('',*,*,#12162,.T.);
#15579=ORIENTED_EDGE('',*,*,#12174,.F.);
#15580=ORIENTED_EDGE('',*,*,#12173,.T.);
#15581=ORIENTED_EDGE('',*,*,#12175,.F.);
#15582=ORIENTED_EDGE('',*,*,#12175,.T.);
#15583=ORIENTED_EDGE('',*,*,#12176,.T.);
#15584=ORIENTED_EDGE('',*,*,#12168,.F.);
#15585=ORIENTED_EDGE('',*,*,#12176,.F.);
#15586=ORIENTED_EDGE('',*,*,#12177,.F.);
#15587=ORIENTED_EDGE('',*,*,#12178,.F.);
#15588=ORIENTED_EDGE('',*,*,#12179,.T.);
#15589=ORIENTED_EDGE('',*,*,#12180,.F.);
#15590=ORIENTED_EDGE('',*,*,#12181,.F.);
#15591=ORIENTED_EDGE('',*,*,#12179,.F.);
#15592=ORIENTED_EDGE('',*,*,#12182,.T.);
#15593=ORIENTED_EDGE('',*,*,#12183,.T.);
#15594=ORIENTED_EDGE('',*,*,#12180,.T.);
#15595=ORIENTED_EDGE('',*,*,#12181,.T.);
#15596=ORIENTED_EDGE('',*,*,#12183,.F.);
#15597=ORIENTED_EDGE('',*,*,#12184,.F.);
#15598=ORIENTED_EDGE('',*,*,#12185,.T.);
#15599=ORIENTED_EDGE('',*,*,#12186,.F.);
#15600=ORIENTED_EDGE('',*,*,#12187,.T.);
#15601=ORIENTED_EDGE('',*,*,#12184,.T.);
#15602=ORIENTED_EDGE('',*,*,#12187,.F.);
#15603=ORIENTED_EDGE('',*,*,#12188,.F.);
#15604=ORIENTED_EDGE('',*,*,#12189,.T.);
#15605=ORIENTED_EDGE('',*,*,#12186,.T.);
#15606=ORIENTED_EDGE('',*,*,#12189,.F.);
#15607=ORIENTED_EDGE('',*,*,#12190,.F.);
#15608=ORIENTED_EDGE('',*,*,#12191,.T.);
#15609=ORIENTED_EDGE('',*,*,#12188,.T.);
#15610=ORIENTED_EDGE('',*,*,#12191,.F.);
#15611=ORIENTED_EDGE('',*,*,#12190,.T.);
#15612=ORIENTED_EDGE('',*,*,#12182,.F.);
#15613=ORIENTED_EDGE('',*,*,#12177,.T.);
#15614=ORIENTED_EDGE('',*,*,#12178,.T.);
#15615=ORIENTED_EDGE('',*,*,#12192,.T.);
#15616=ORIENTED_EDGE('',*,*,#12185,.F.);
#15617=ORIENTED_EDGE('',*,*,#12192,.F.);
#15618=ORIENTED_EDGE('',*,*,#12193,.T.);
#15619=ORIENTED_EDGE('',*,*,#12193,.F.);
#15620=ORIENTED_EDGE('',*,*,#12194,.T.);
#15621=ORIENTED_EDGE('',*,*,#12194,.F.);
#15622=ORIENTED_EDGE('',*,*,#12195,.T.);
#15623=ORIENTED_EDGE('',*,*,#12195,.F.);
#15624=ORIENTED_EDGE('',*,*,#12196,.T.);
#15625=ORIENTED_EDGE('',*,*,#12196,.F.);
#15626=ORIENTED_EDGE('',*,*,#12197,.T.);
#15627=ORIENTED_EDGE('',*,*,#12197,.F.);
#15628=ORIENTED_EDGE('',*,*,#12198,.T.);
#15629=ORIENTED_EDGE('',*,*,#12198,.F.);
#15630=ORIENTED_EDGE('',*,*,#12199,.T.);
#15631=ORIENTED_EDGE('',*,*,#12199,.F.);
#15632=ORIENTED_EDGE('',*,*,#12200,.F.);
#15633=ORIENTED_EDGE('',*,*,#12201,.F.);
#15634=ORIENTED_EDGE('',*,*,#12202,.F.);
#15635=ORIENTED_EDGE('',*,*,#12203,.F.);
#15636=ORIENTED_EDGE('',*,*,#12202,.T.);
#15637=ORIENTED_EDGE('',*,*,#12204,.F.);
#15638=ORIENTED_EDGE('',*,*,#12205,.T.);
#15639=ORIENTED_EDGE('',*,*,#12206,.F.);
#15640=ORIENTED_EDGE('',*,*,#12207,.T.);
#15641=ORIENTED_EDGE('',*,*,#12208,.F.);
#15642=ORIENTED_EDGE('',*,*,#12209,.T.);
#15643=ORIENTED_EDGE('',*,*,#12210,.F.);
#15644=ORIENTED_EDGE('',*,*,#12209,.F.);
#15645=ORIENTED_EDGE('',*,*,#12211,.F.);
#15646=ORIENTED_EDGE('',*,*,#12212,.T.);
#15647=ORIENTED_EDGE('',*,*,#12213,.F.);
#15648=ORIENTED_EDGE('',*,*,#12214,.T.);
#15649=ORIENTED_EDGE('',*,*,#12215,.F.);
#15650=ORIENTED_EDGE('',*,*,#12216,.T.);
#15651=ORIENTED_EDGE('',*,*,#12217,.F.);
#15652=ORIENTED_EDGE('',*,*,#12218,.T.);
#15653=ORIENTED_EDGE('',*,*,#12219,.F.);
#15654=ORIENTED_EDGE('',*,*,#12201,.T.);
#15655=ORIENTED_EDGE('',*,*,#12220,.T.);
#15656=ORIENTED_EDGE('',*,*,#12221,.T.);
#15657=ORIENTED_EDGE('',*,*,#12204,.T.);
#15658=ORIENTED_EDGE('',*,*,#12222,.F.);
#15659=ORIENTED_EDGE('',*,*,#12223,.F.);
#15660=ORIENTED_EDGE('',*,*,#12205,.F.);
#15661=ORIENTED_EDGE('',*,*,#12221,.F.);
#15662=ORIENTED_EDGE('',*,*,#12223,.T.);
#15663=ORIENTED_EDGE('',*,*,#12224,.T.);
#15664=ORIENTED_EDGE('',*,*,#12225,.T.);
#15665=ORIENTED_EDGE('',*,*,#12206,.T.);
#15666=ORIENTED_EDGE('',*,*,#12226,.F.);
#15667=ORIENTED_EDGE('',*,*,#12227,.F.);
#15668=ORIENTED_EDGE('',*,*,#12207,.F.);
#15669=ORIENTED_EDGE('',*,*,#12225,.F.);
#15670=ORIENTED_EDGE('',*,*,#12227,.T.);
#15671=ORIENTED_EDGE('',*,*,#12228,.T.);
#15672=ORIENTED_EDGE('',*,*,#12229,.T.);
#15673=ORIENTED_EDGE('',*,*,#12230,.T.);
#15674=ORIENTED_EDGE('',*,*,#12211,.T.);
#15675=ORIENTED_EDGE('',*,*,#12208,.T.);
#15676=ORIENTED_EDGE('',*,*,#12231,.F.);
#15677=ORIENTED_EDGE('',*,*,#12232,.F.);
#15678=ORIENTED_EDGE('',*,*,#12212,.F.);
#15679=ORIENTED_EDGE('',*,*,#12230,.F.);
#15680=ORIENTED_EDGE('',*,*,#12232,.T.);
#15681=ORIENTED_EDGE('',*,*,#12233,.T.);
#15682=ORIENTED_EDGE('',*,*,#12234,.T.);
#15683=ORIENTED_EDGE('',*,*,#12213,.T.);
#15684=ORIENTED_EDGE('',*,*,#12235,.F.);
#15685=ORIENTED_EDGE('',*,*,#12236,.F.);
#15686=ORIENTED_EDGE('',*,*,#12214,.F.);
#15687=ORIENTED_EDGE('',*,*,#12234,.F.);
#15688=ORIENTED_EDGE('',*,*,#12236,.T.);
#15689=ORIENTED_EDGE('',*,*,#12237,.T.);
#15690=ORIENTED_EDGE('',*,*,#12238,.T.);
#15691=ORIENTED_EDGE('',*,*,#12215,.T.);
#15692=ORIENTED_EDGE('',*,*,#12216,.F.);
#15693=ORIENTED_EDGE('',*,*,#12238,.F.);
#15694=ORIENTED_EDGE('',*,*,#12239,.F.);
#15695=ORIENTED_EDGE('',*,*,#12240,.F.);
#15696=ORIENTED_EDGE('',*,*,#12241,.F.);
#15697=ORIENTED_EDGE('',*,*,#12242,.T.);
#15698=ORIENTED_EDGE('',*,*,#12228,.F.);
#15699=ORIENTED_EDGE('',*,*,#12226,.T.);
#15700=ORIENTED_EDGE('',*,*,#12224,.F.);
#15701=ORIENTED_EDGE('',*,*,#12222,.T.);
#15702=ORIENTED_EDGE('',*,*,#12220,.F.);
#15703=ORIENTED_EDGE('',*,*,#12200,.T.);
#15704=ORIENTED_EDGE('',*,*,#12243,.F.);
#15705=ORIENTED_EDGE('',*,*,#12244,.T.);
#15706=ORIENTED_EDGE('',*,*,#12245,.F.);
#15707=ORIENTED_EDGE('',*,*,#12239,.T.);
#15708=ORIENTED_EDGE('',*,*,#12237,.F.);
#15709=ORIENTED_EDGE('',*,*,#12235,.T.);
#15710=ORIENTED_EDGE('',*,*,#12233,.F.);
#15711=ORIENTED_EDGE('',*,*,#12231,.T.);
#15712=ORIENTED_EDGE('',*,*,#12229,.F.);
#15713=ORIENTED_EDGE('',*,*,#12242,.F.);
#15714=ORIENTED_EDGE('',*,*,#12203,.T.);
#15715=ORIENTED_EDGE('',*,*,#12219,.T.);
#15716=ORIENTED_EDGE('',*,*,#12246,.T.);
#15717=ORIENTED_EDGE('',*,*,#12243,.T.);
#15718=ORIENTED_EDGE('',*,*,#12218,.F.);
#15719=ORIENTED_EDGE('',*,*,#12247,.F.);
#15720=ORIENTED_EDGE('',*,*,#12244,.F.);
#15721=ORIENTED_EDGE('',*,*,#12246,.F.);
#15722=ORIENTED_EDGE('',*,*,#12210,.T.);
#15723=ORIENTED_EDGE('',*,*,#12241,.T.);
#15724=ORIENTED_EDGE('',*,*,#12240,.T.);
#15725=ORIENTED_EDGE('',*,*,#12245,.T.);
#15726=ORIENTED_EDGE('',*,*,#12247,.T.);
#15727=ORIENTED_EDGE('',*,*,#12217,.T.);
#15728=ORIENTED_EDGE('',*,*,#12248,.F.);
#15729=ORIENTED_EDGE('',*,*,#12249,.T.);
#15730=ORIENTED_EDGE('',*,*,#12250,.F.);
#15731=ORIENTED_EDGE('',*,*,#12251,.T.);
#15732=ORIENTED_EDGE('',*,*,#12248,.T.);
#15733=ORIENTED_EDGE('',*,*,#12251,.F.);
#15734=ORIENTED_EDGE('',*,*,#12250,.T.);
#15735=ORIENTED_EDGE('',*,*,#12252,.F.);
#15736=ORIENTED_EDGE('',*,*,#12252,.T.);
#15737=ORIENTED_EDGE('',*,*,#12253,.T.);
#15738=ORIENTED_EDGE('',*,*,#12249,.F.);
#15739=ORIENTED_EDGE('',*,*,#12253,.F.);
#15740=ORIENTED_EDGE('',*,*,#12254,.F.);
#15741=ORIENTED_EDGE('',*,*,#12255,.T.);
#15742=ORIENTED_EDGE('',*,*,#12256,.F.);
#15743=ORIENTED_EDGE('',*,*,#12257,.T.);
#15744=ORIENTED_EDGE('',*,*,#12254,.T.);
#15745=ORIENTED_EDGE('',*,*,#12257,.F.);
#15746=ORIENTED_EDGE('',*,*,#12256,.T.);
#15747=ORIENTED_EDGE('',*,*,#12258,.F.);
#15748=ORIENTED_EDGE('',*,*,#12258,.T.);
#15749=ORIENTED_EDGE('',*,*,#12259,.T.);
#15750=ORIENTED_EDGE('',*,*,#12255,.F.);
#15751=ORIENTED_EDGE('',*,*,#12259,.F.);
#15752=ORIENTED_EDGE('',*,*,#12260,.F.);
#15753=ORIENTED_EDGE('',*,*,#12261,.F.);
#15754=ORIENTED_EDGE('',*,*,#12262,.T.);
#15755=ORIENTED_EDGE('',*,*,#12263,.F.);
#15756=ORIENTED_EDGE('',*,*,#12264,.F.);
#15757=ORIENTED_EDGE('',*,*,#12262,.F.);
#15758=ORIENTED_EDGE('',*,*,#12263,.T.);
#15759=ORIENTED_EDGE('',*,*,#12264,.T.);
#15760=ORIENTED_EDGE('',*,*,#12265,.T.);
#15761=ORIENTED_EDGE('',*,*,#12266,.T.);
#15762=ORIENTED_EDGE('',*,*,#12265,.F.);
#15763=ORIENTED_EDGE('',*,*,#12267,.T.);
#15764=ORIENTED_EDGE('',*,*,#12268,.T.);
#15765=ORIENTED_EDGE('',*,*,#12269,.F.);
#15766=ORIENTED_EDGE('',*,*,#12268,.F.);
#15767=ORIENTED_EDGE('',*,*,#12269,.T.);
#15768=ORIENTED_EDGE('',*,*,#12270,.T.);
#15769=ORIENTED_EDGE('',*,*,#12271,.F.);
#15770=ORIENTED_EDGE('',*,*,#12270,.F.);
#15771=ORIENTED_EDGE('',*,*,#12266,.F.);
#15772=ORIENTED_EDGE('',*,*,#12271,.T.);
#15773=ORIENTED_EDGE('',*,*,#12272,.F.);
#15774=ORIENTED_EDGE('',*,*,#12273,.T.);
#15775=ORIENTED_EDGE('',*,*,#12260,.T.);
#15776=ORIENTED_EDGE('',*,*,#12261,.T.);
#15777=ORIENTED_EDGE('',*,*,#12273,.F.);
#15778=ORIENTED_EDGE('',*,*,#12272,.T.);
#15779=ORIENTED_EDGE('',*,*,#12274,.F.);
#15780=ORIENTED_EDGE('',*,*,#12274,.T.);
#15781=ORIENTED_EDGE('',*,*,#12275,.T.);
#15782=ORIENTED_EDGE('',*,*,#12267,.F.);
#15783=ORIENTED_EDGE('',*,*,#12275,.F.);
#15784=ORIENTED_EDGE('',*,*,#12276,.F.);
#15785=ORIENTED_EDGE('',*,*,#12277,.F.);
#15786=ORIENTED_EDGE('',*,*,#12278,.T.);
#15787=ORIENTED_EDGE('',*,*,#12279,.F.);
#15788=ORIENTED_EDGE('',*,*,#12280,.F.);
#15789=ORIENTED_EDGE('',*,*,#12278,.F.);
#15790=ORIENTED_EDGE('',*,*,#12281,.T.);
#15791=ORIENTED_EDGE('',*,*,#12282,.T.);
#15792=ORIENTED_EDGE('',*,*,#12279,.T.);
#15793=ORIENTED_EDGE('',*,*,#12280,.T.);
#15794=ORIENTED_EDGE('',*,*,#12282,.F.);
#15795=ORIENTED_EDGE('',*,*,#12283,.F.);
#15796=ORIENTED_EDGE('',*,*,#12284,.T.);
#15797=ORIENTED_EDGE('',*,*,#12285,.F.);
#15798=ORIENTED_EDGE('',*,*,#12286,.T.);
#15799=ORIENTED_EDGE('',*,*,#12283,.T.);
#15800=ORIENTED_EDGE('',*,*,#12286,.F.);
#15801=ORIENTED_EDGE('',*,*,#12287,.F.);
#15802=ORIENTED_EDGE('',*,*,#12288,.T.);
#15803=ORIENTED_EDGE('',*,*,#12285,.T.);
#15804=ORIENTED_EDGE('',*,*,#12288,.F.);
#15805=ORIENTED_EDGE('',*,*,#12289,.F.);
#15806=ORIENTED_EDGE('',*,*,#12290,.T.);
#15807=ORIENTED_EDGE('',*,*,#12287,.T.);
#15808=ORIENTED_EDGE('',*,*,#12290,.F.);
#15809=ORIENTED_EDGE('',*,*,#12289,.T.);
#15810=ORIENTED_EDGE('',*,*,#12281,.F.);
#15811=ORIENTED_EDGE('',*,*,#12276,.T.);
#15812=ORIENTED_EDGE('',*,*,#12277,.T.);
#15813=ORIENTED_EDGE('',*,*,#12291,.T.);
#15814=ORIENTED_EDGE('',*,*,#12284,.F.);
#15815=ORIENTED_EDGE('',*,*,#12291,.F.);
#15816=ORIENTED_EDGE('',*,*,#12292,.T.);
#15817=ORIENTED_EDGE('',*,*,#12292,.F.);
#15818=ORIENTED_EDGE('',*,*,#12293,.T.);
#15819=ORIENTED_EDGE('',*,*,#12293,.F.);
#15820=ORIENTED_EDGE('',*,*,#12294,.T.);
#15821=ORIENTED_EDGE('',*,*,#12294,.F.);
#15822=ORIENTED_EDGE('',*,*,#12295,.T.);
#15823=ORIENTED_EDGE('',*,*,#12295,.F.);
#15824=ORIENTED_EDGE('',*,*,#12296,.T.);
#15825=ORIENTED_EDGE('',*,*,#12296,.F.);
#15826=ORIENTED_EDGE('',*,*,#12297,.T.);
#15827=ORIENTED_EDGE('',*,*,#12297,.F.);
#15828=ORIENTED_EDGE('',*,*,#12298,.T.);
#15829=ORIENTED_EDGE('',*,*,#12298,.F.);
#15830=ORIENTED_EDGE('',*,*,#12299,.T.);
#15831=ORIENTED_EDGE('',*,*,#12299,.F.);
#15832=ORIENTED_EDGE('',*,*,#12300,.F.);
#15833=ORIENTED_EDGE('',*,*,#12301,.F.);
#15834=ORIENTED_EDGE('',*,*,#12302,.F.);
#15835=ORIENTED_EDGE('',*,*,#12303,.F.);
#15836=ORIENTED_EDGE('',*,*,#12302,.T.);
#15837=ORIENTED_EDGE('',*,*,#12304,.F.);
#15838=ORIENTED_EDGE('',*,*,#12305,.T.);
#15839=ORIENTED_EDGE('',*,*,#12306,.F.);
#15840=ORIENTED_EDGE('',*,*,#12307,.T.);
#15841=ORIENTED_EDGE('',*,*,#12308,.F.);
#15842=ORIENTED_EDGE('',*,*,#12309,.T.);
#15843=ORIENTED_EDGE('',*,*,#12310,.T.);
#15844=ORIENTED_EDGE('',*,*,#12311,.F.);
#15845=ORIENTED_EDGE('',*,*,#12310,.F.);
#15846=ORIENTED_EDGE('',*,*,#12312,.T.);
#15847=ORIENTED_EDGE('',*,*,#12313,.F.);
#15848=ORIENTED_EDGE('',*,*,#12314,.T.);
#15849=ORIENTED_EDGE('',*,*,#12315,.F.);
#15850=ORIENTED_EDGE('',*,*,#12316,.T.);
#15851=ORIENTED_EDGE('',*,*,#12317,.F.);
#15852=ORIENTED_EDGE('',*,*,#12318,.T.);
#15853=ORIENTED_EDGE('',*,*,#12319,.F.);
#15854=ORIENTED_EDGE('',*,*,#12320,.T.);
#15855=ORIENTED_EDGE('',*,*,#12321,.F.);
#15856=ORIENTED_EDGE('',*,*,#12301,.T.);
#15857=ORIENTED_EDGE('',*,*,#12322,.T.);
#15858=ORIENTED_EDGE('',*,*,#12323,.T.);
#15859=ORIENTED_EDGE('',*,*,#12304,.T.);
#15860=ORIENTED_EDGE('',*,*,#12324,.F.);
#15861=ORIENTED_EDGE('',*,*,#12325,.F.);
#15862=ORIENTED_EDGE('',*,*,#12305,.F.);
#15863=ORIENTED_EDGE('',*,*,#12323,.F.);
#15864=ORIENTED_EDGE('',*,*,#12325,.T.);
#15865=ORIENTED_EDGE('',*,*,#12326,.T.);
#15866=ORIENTED_EDGE('',*,*,#12327,.T.);
#15867=ORIENTED_EDGE('',*,*,#12306,.T.);
#15868=ORIENTED_EDGE('',*,*,#12328,.F.);
#15869=ORIENTED_EDGE('',*,*,#12329,.F.);
#15870=ORIENTED_EDGE('',*,*,#12307,.F.);
#15871=ORIENTED_EDGE('',*,*,#12327,.F.);
#15872=ORIENTED_EDGE('',*,*,#12329,.T.);
#15873=ORIENTED_EDGE('',*,*,#12330,.T.);
#15874=ORIENTED_EDGE('',*,*,#12331,.T.);
#15875=ORIENTED_EDGE('',*,*,#12308,.T.);
#15876=ORIENTED_EDGE('',*,*,#12332,.F.);
#15877=ORIENTED_EDGE('',*,*,#12333,.F.);
#15878=ORIENTED_EDGE('',*,*,#12312,.F.);
#15879=ORIENTED_EDGE('',*,*,#12309,.F.);
#15880=ORIENTED_EDGE('',*,*,#12331,.F.);
#15881=ORIENTED_EDGE('',*,*,#12334,.F.);
#15882=ORIENTED_EDGE('',*,*,#12333,.T.);
#15883=ORIENTED_EDGE('',*,*,#12335,.T.);
#15884=ORIENTED_EDGE('',*,*,#12336,.T.);
#15885=ORIENTED_EDGE('',*,*,#12313,.T.);
#15886=ORIENTED_EDGE('',*,*,#12337,.F.);
#15887=ORIENTED_EDGE('',*,*,#12338,.F.);
#15888=ORIENTED_EDGE('',*,*,#12314,.F.);
#15889=ORIENTED_EDGE('',*,*,#12336,.F.);
#15890=ORIENTED_EDGE('',*,*,#12338,.T.);
#15891=ORIENTED_EDGE('',*,*,#12339,.T.);
#15892=ORIENTED_EDGE('',*,*,#12340,.T.);
#15893=ORIENTED_EDGE('',*,*,#12315,.T.);
#15894=ORIENTED_EDGE('',*,*,#12341,.F.);
#15895=ORIENTED_EDGE('',*,*,#12342,.F.);
#15896=ORIENTED_EDGE('',*,*,#12316,.F.);
#15897=ORIENTED_EDGE('',*,*,#12340,.F.);
#15898=ORIENTED_EDGE('',*,*,#12342,.T.);
#15899=ORIENTED_EDGE('',*,*,#12343,.T.);
#15900=ORIENTED_EDGE('',*,*,#12344,.T.);
#15901=ORIENTED_EDGE('',*,*,#12317,.T.);
#15902=ORIENTED_EDGE('',*,*,#12318,.F.);
#15903=ORIENTED_EDGE('',*,*,#12344,.F.);
#15904=ORIENTED_EDGE('',*,*,#12345,.F.);
#15905=ORIENTED_EDGE('',*,*,#12346,.F.);
#15906=ORIENTED_EDGE('',*,*,#12347,.F.);
#15907=ORIENTED_EDGE('',*,*,#12348,.T.);
#15908=ORIENTED_EDGE('',*,*,#12334,.T.);
#15909=ORIENTED_EDGE('',*,*,#12330,.F.);
#15910=ORIENTED_EDGE('',*,*,#12328,.T.);
#15911=ORIENTED_EDGE('',*,*,#12326,.F.);
#15912=ORIENTED_EDGE('',*,*,#12324,.T.);
#15913=ORIENTED_EDGE('',*,*,#12322,.F.);
#15914=ORIENTED_EDGE('',*,*,#12300,.T.);
#15915=ORIENTED_EDGE('',*,*,#12349,.F.);
#15916=ORIENTED_EDGE('',*,*,#12350,.T.);
#15917=ORIENTED_EDGE('',*,*,#12351,.F.);
#15918=ORIENTED_EDGE('',*,*,#12345,.T.);
#15919=ORIENTED_EDGE('',*,*,#12343,.F.);
#15920=ORIENTED_EDGE('',*,*,#12341,.T.);
#15921=ORIENTED_EDGE('',*,*,#12339,.F.);
#15922=ORIENTED_EDGE('',*,*,#12337,.T.);
#15923=ORIENTED_EDGE('',*,*,#12335,.F.);
#15924=ORIENTED_EDGE('',*,*,#12332,.T.);
#15925=ORIENTED_EDGE('',*,*,#12348,.F.);
#15926=ORIENTED_EDGE('',*,*,#12303,.T.);
#15927=ORIENTED_EDGE('',*,*,#12321,.T.);
#15928=ORIENTED_EDGE('',*,*,#12352,.T.);
#15929=ORIENTED_EDGE('',*,*,#12349,.T.);
#15930=ORIENTED_EDGE('',*,*,#12320,.F.);
#15931=ORIENTED_EDGE('',*,*,#12353,.F.);
#15932=ORIENTED_EDGE('',*,*,#12350,.F.);
#15933=ORIENTED_EDGE('',*,*,#12352,.F.);
#15934=ORIENTED_EDGE('',*,*,#12311,.T.);
#15935=ORIENTED_EDGE('',*,*,#12347,.T.);
#15936=ORIENTED_EDGE('',*,*,#12346,.T.);
#15937=ORIENTED_EDGE('',*,*,#12351,.T.);
#15938=ORIENTED_EDGE('',*,*,#12353,.T.);
#15939=ORIENTED_EDGE('',*,*,#12319,.T.);
#15940=ORIENTED_EDGE('',*,*,#12354,.F.);
#15941=ORIENTED_EDGE('',*,*,#12355,.T.);
#15942=ORIENTED_EDGE('',*,*,#12356,.F.);
#15943=ORIENTED_EDGE('',*,*,#12357,.T.);
#15944=ORIENTED_EDGE('',*,*,#12354,.T.);
#15945=ORIENTED_EDGE('',*,*,#12357,.F.);
#15946=ORIENTED_EDGE('',*,*,#12356,.T.);
#15947=ORIENTED_EDGE('',*,*,#12358,.F.);
#15948=ORIENTED_EDGE('',*,*,#12358,.T.);
#15949=ORIENTED_EDGE('',*,*,#12359,.T.);
#15950=ORIENTED_EDGE('',*,*,#12355,.F.);
#15951=ORIENTED_EDGE('',*,*,#12359,.F.);
#15952=ORIENTED_EDGE('',*,*,#12360,.F.);
#15953=ORIENTED_EDGE('',*,*,#12361,.T.);
#15954=ORIENTED_EDGE('',*,*,#12362,.F.);
#15955=ORIENTED_EDGE('',*,*,#12363,.T.);
#15956=ORIENTED_EDGE('',*,*,#12360,.T.);
#15957=ORIENTED_EDGE('',*,*,#12363,.F.);
#15958=ORIENTED_EDGE('',*,*,#12362,.T.);
#15959=ORIENTED_EDGE('',*,*,#12364,.F.);
#15960=ORIENTED_EDGE('',*,*,#12364,.T.);
#15961=ORIENTED_EDGE('',*,*,#12365,.T.);
#15962=ORIENTED_EDGE('',*,*,#12361,.F.);
#15963=ORIENTED_EDGE('',*,*,#12365,.F.);
#15964=ORIENTED_EDGE('',*,*,#12366,.F.);
#15965=ORIENTED_EDGE('',*,*,#12367,.T.);
#15966=ORIENTED_EDGE('',*,*,#12368,.F.);
#15967=ORIENTED_EDGE('',*,*,#12367,.F.);
#15968=ORIENTED_EDGE('',*,*,#12369,.F.);
#15969=ORIENTED_EDGE('',*,*,#12370,.T.);
#15970=ORIENTED_EDGE('',*,*,#12371,.F.);
#15971=ORIENTED_EDGE('',*,*,#12370,.F.);
#15972=ORIENTED_EDGE('',*,*,#12372,.F.);
#15973=ORIENTED_EDGE('',*,*,#12373,.T.);
#15974=ORIENTED_EDGE('',*,*,#12374,.F.);
#15975=ORIENTED_EDGE('',*,*,#12373,.F.);
#15976=ORIENTED_EDGE('',*,*,#12375,.F.);
#15977=ORIENTED_EDGE('',*,*,#12376,.T.);
#15978=ORIENTED_EDGE('',*,*,#12377,.F.);
#15979=ORIENTED_EDGE('',*,*,#12376,.F.);
#15980=ORIENTED_EDGE('',*,*,#12378,.T.);
#15981=ORIENTED_EDGE('',*,*,#12379,.T.);
#15982=ORIENTED_EDGE('',*,*,#12380,.F.);
#15983=ORIENTED_EDGE('',*,*,#12381,.F.);
#15984=ORIENTED_EDGE('',*,*,#12382,.T.);
#15985=ORIENTED_EDGE('',*,*,#12381,.T.);
#15986=ORIENTED_EDGE('',*,*,#12383,.F.);
#15987=ORIENTED_EDGE('',*,*,#12384,.F.);
#15988=ORIENTED_EDGE('',*,*,#12385,.T.);
#15989=ORIENTED_EDGE('',*,*,#12384,.T.);
#15990=ORIENTED_EDGE('',*,*,#12386,.F.);
#15991=ORIENTED_EDGE('',*,*,#12387,.F.);
#15992=ORIENTED_EDGE('',*,*,#12388,.T.);
#15993=ORIENTED_EDGE('',*,*,#12387,.T.);
#15994=ORIENTED_EDGE('',*,*,#12389,.F.);
#15995=ORIENTED_EDGE('',*,*,#12379,.F.);
#15996=ORIENTED_EDGE('',*,*,#12389,.T.);
#15997=ORIENTED_EDGE('',*,*,#12386,.T.);
#15998=ORIENTED_EDGE('',*,*,#12383,.T.);
#15999=ORIENTED_EDGE('',*,*,#12380,.T.);
#16000=ORIENTED_EDGE('',*,*,#12368,.T.);
#16001=ORIENTED_EDGE('',*,*,#12371,.T.);
#16002=ORIENTED_EDGE('',*,*,#12374,.T.);
#16003=ORIENTED_EDGE('',*,*,#12377,.T.);
#16004=ORIENTED_EDGE('',*,*,#12388,.F.);
#16005=ORIENTED_EDGE('',*,*,#12378,.F.);
#16006=ORIENTED_EDGE('',*,*,#12382,.F.);
#16007=ORIENTED_EDGE('',*,*,#12385,.F.);
#16008=ORIENTED_EDGE('',*,*,#12366,.T.);
#16009=ORIENTED_EDGE('',*,*,#12369,.T.);
#16010=ORIENTED_EDGE('',*,*,#12372,.T.);
#16011=ORIENTED_EDGE('',*,*,#12375,.T.);
#16012=ORIENTED_EDGE('',*,*,#12390,.F.);
#16013=ORIENTED_EDGE('',*,*,#12391,.T.);
#16014=ORIENTED_EDGE('',*,*,#12392,.F.);
#16015=ORIENTED_EDGE('',*,*,#12391,.F.);
#16016=ORIENTED_EDGE('',*,*,#12393,.F.);
#16017=ORIENTED_EDGE('',*,*,#12394,.T.);
#16018=ORIENTED_EDGE('',*,*,#12395,.F.);
#16019=ORIENTED_EDGE('',*,*,#12394,.F.);
#16020=ORIENTED_EDGE('',*,*,#12396,.F.);
#16021=ORIENTED_EDGE('',*,*,#12397,.T.);
#16022=ORIENTED_EDGE('',*,*,#12398,.F.);
#16023=ORIENTED_EDGE('',*,*,#12397,.F.);
#16024=ORIENTED_EDGE('',*,*,#12399,.F.);
#16025=ORIENTED_EDGE('',*,*,#12400,.T.);
#16026=ORIENTED_EDGE('',*,*,#12401,.F.);
#16027=ORIENTED_EDGE('',*,*,#12400,.F.);
#16028=ORIENTED_EDGE('',*,*,#12402,.F.);
#16029=ORIENTED_EDGE('',*,*,#12403,.T.);
#16030=ORIENTED_EDGE('',*,*,#12404,.F.);
#16031=ORIENTED_EDGE('',*,*,#12403,.F.);
#16032=ORIENTED_EDGE('',*,*,#12405,.F.);
#16033=ORIENTED_EDGE('',*,*,#12406,.T.);
#16034=ORIENTED_EDGE('',*,*,#12407,.F.);
#16035=ORIENTED_EDGE('',*,*,#12406,.F.);
#16036=ORIENTED_EDGE('',*,*,#12408,.F.);
#16037=ORIENTED_EDGE('',*,*,#12409,.T.);
#16038=ORIENTED_EDGE('',*,*,#12410,.F.);
#16039=ORIENTED_EDGE('',*,*,#12409,.F.);
#16040=ORIENTED_EDGE('',*,*,#12411,.F.);
#16041=ORIENTED_EDGE('',*,*,#12412,.T.);
#16042=ORIENTED_EDGE('',*,*,#12413,.F.);
#16043=ORIENTED_EDGE('',*,*,#12412,.F.);
#16044=ORIENTED_EDGE('',*,*,#12414,.F.);
#16045=ORIENTED_EDGE('',*,*,#12415,.T.);
#16046=ORIENTED_EDGE('',*,*,#12416,.F.);
#16047=ORIENTED_EDGE('',*,*,#12415,.F.);
#16048=ORIENTED_EDGE('',*,*,#12417,.F.);
#16049=ORIENTED_EDGE('',*,*,#12418,.T.);
#16050=ORIENTED_EDGE('',*,*,#12419,.F.);
#16051=ORIENTED_EDGE('',*,*,#12418,.F.);
#16052=ORIENTED_EDGE('',*,*,#12420,.F.);
#16053=ORIENTED_EDGE('',*,*,#12421,.T.);
#16054=ORIENTED_EDGE('',*,*,#12422,.F.);
#16055=ORIENTED_EDGE('',*,*,#12421,.F.);
#16056=ORIENTED_EDGE('',*,*,#12423,.F.);
#16057=ORIENTED_EDGE('',*,*,#12424,.T.);
#16058=ORIENTED_EDGE('',*,*,#12425,.F.);
#16059=ORIENTED_EDGE('',*,*,#12424,.F.);
#16060=ORIENTED_EDGE('',*,*,#12426,.T.);
#16061=ORIENTED_EDGE('',*,*,#12427,.T.);
#16062=ORIENTED_EDGE('',*,*,#12428,.F.);
#16063=ORIENTED_EDGE('',*,*,#12429,.F.);
#16064=ORIENTED_EDGE('',*,*,#12430,.T.);
#16065=ORIENTED_EDGE('',*,*,#12429,.T.);
#16066=ORIENTED_EDGE('',*,*,#12431,.F.);
#16067=ORIENTED_EDGE('',*,*,#12432,.F.);
#16068=ORIENTED_EDGE('',*,*,#12433,.T.);
#16069=ORIENTED_EDGE('',*,*,#12432,.T.);
#16070=ORIENTED_EDGE('',*,*,#12434,.F.);
#16071=ORIENTED_EDGE('',*,*,#12435,.F.);
#16072=ORIENTED_EDGE('',*,*,#12436,.T.);
#16073=ORIENTED_EDGE('',*,*,#12435,.T.);
#16074=ORIENTED_EDGE('',*,*,#12437,.F.);
#16075=ORIENTED_EDGE('',*,*,#12427,.F.);
#16076=ORIENTED_EDGE('',*,*,#12437,.T.);
#16077=ORIENTED_EDGE('',*,*,#12434,.T.);
#16078=ORIENTED_EDGE('',*,*,#12431,.T.);
#16079=ORIENTED_EDGE('',*,*,#12428,.T.);
#16080=ORIENTED_EDGE('',*,*,#12404,.T.);
#16081=ORIENTED_EDGE('',*,*,#12407,.T.);
#16082=ORIENTED_EDGE('',*,*,#12410,.T.);
#16083=ORIENTED_EDGE('',*,*,#12413,.T.);
#16084=ORIENTED_EDGE('',*,*,#12416,.T.);
#16085=ORIENTED_EDGE('',*,*,#12419,.T.);
#16086=ORIENTED_EDGE('',*,*,#12422,.T.);
#16087=ORIENTED_EDGE('',*,*,#12425,.T.);
#16088=ORIENTED_EDGE('',*,*,#12401,.T.);
#16089=ORIENTED_EDGE('',*,*,#12398,.T.);
#16090=ORIENTED_EDGE('',*,*,#12395,.T.);
#16091=ORIENTED_EDGE('',*,*,#12392,.T.);
#16092=ORIENTED_EDGE('',*,*,#12436,.F.);
#16093=ORIENTED_EDGE('',*,*,#12426,.F.);
#16094=ORIENTED_EDGE('',*,*,#12430,.F.);
#16095=ORIENTED_EDGE('',*,*,#12433,.F.);
#16096=ORIENTED_EDGE('',*,*,#12402,.T.);
#16097=ORIENTED_EDGE('',*,*,#12405,.T.);
#16098=ORIENTED_EDGE('',*,*,#12408,.T.);
#16099=ORIENTED_EDGE('',*,*,#12411,.T.);
#16100=ORIENTED_EDGE('',*,*,#12414,.T.);
#16101=ORIENTED_EDGE('',*,*,#12417,.T.);
#16102=ORIENTED_EDGE('',*,*,#12420,.T.);
#16103=ORIENTED_EDGE('',*,*,#12423,.T.);
#16104=ORIENTED_EDGE('',*,*,#12399,.T.);
#16105=ORIENTED_EDGE('',*,*,#12396,.T.);
#16106=ORIENTED_EDGE('',*,*,#12393,.T.);
#16107=ORIENTED_EDGE('',*,*,#12390,.T.);
#16108=ORIENTED_EDGE('',*,*,#12438,.F.);
#16109=ORIENTED_EDGE('',*,*,#12439,.T.);
#16110=ORIENTED_EDGE('',*,*,#12440,.F.);
#16111=ORIENTED_EDGE('',*,*,#12439,.F.);
#16112=ORIENTED_EDGE('',*,*,#12438,.T.);
#16113=ORIENTED_EDGE('',*,*,#12441,.F.);
#16114=ORIENTED_EDGE('',*,*,#12442,.T.);
#16115=ORIENTED_EDGE('',*,*,#12443,.F.);
#16116=ORIENTED_EDGE('',*,*,#12442,.F.);
#16117=ORIENTED_EDGE('',*,*,#12441,.T.);
#16118=ORIENTED_EDGE('',*,*,#12444,.F.);
#16119=ORIENTED_EDGE('',*,*,#12445,.T.);
#16120=ORIENTED_EDGE('',*,*,#12446,.F.);
#16121=ORIENTED_EDGE('',*,*,#12445,.F.);
#16122=ORIENTED_EDGE('',*,*,#12444,.T.);
#16123=ORIENTED_EDGE('',*,*,#12447,.F.);
#16124=ORIENTED_EDGE('',*,*,#12448,.T.);
#16125=ORIENTED_EDGE('',*,*,#12449,.F.);
#16126=ORIENTED_EDGE('',*,*,#12448,.F.);
#16127=ORIENTED_EDGE('',*,*,#12447,.T.);
#16128=ORIENTED_EDGE('',*,*,#12450,.F.);
#16129=ORIENTED_EDGE('',*,*,#12451,.T.);
#16130=ORIENTED_EDGE('',*,*,#12452,.F.);
#16131=ORIENTED_EDGE('',*,*,#12451,.F.);
#16132=ORIENTED_EDGE('',*,*,#12450,.T.);
#16133=ORIENTED_EDGE('',*,*,#12453,.F.);
#16134=ORIENTED_EDGE('',*,*,#12454,.T.);
#16135=ORIENTED_EDGE('',*,*,#12455,.F.);
#16136=ORIENTED_EDGE('',*,*,#12454,.F.);
#16137=ORIENTED_EDGE('',*,*,#12453,.T.);
#16138=ORIENTED_EDGE('',*,*,#12456,.F.);
#16139=ORIENTED_EDGE('',*,*,#12457,.T.);
#16140=ORIENTED_EDGE('',*,*,#12458,.F.);
#16141=ORIENTED_EDGE('',*,*,#12457,.F.);
#16142=ORIENTED_EDGE('',*,*,#12456,.T.);
#16143=ORIENTED_EDGE('',*,*,#12459,.F.);
#16144=ORIENTED_EDGE('',*,*,#12460,.T.);
#16145=ORIENTED_EDGE('',*,*,#12461,.F.);
#16146=ORIENTED_EDGE('',*,*,#12460,.F.);
#16147=ORIENTED_EDGE('',*,*,#12462,.T.);
#16148=ORIENTED_EDGE('',*,*,#12463,.T.);
#16149=ORIENTED_EDGE('',*,*,#12464,.F.);
#16150=ORIENTED_EDGE('',*,*,#12465,.F.);
#16151=ORIENTED_EDGE('',*,*,#12466,.T.);
#16152=ORIENTED_EDGE('',*,*,#12465,.T.);
#16153=ORIENTED_EDGE('',*,*,#12467,.F.);
#16154=ORIENTED_EDGE('',*,*,#12468,.F.);
#16155=ORIENTED_EDGE('',*,*,#12452,.T.);
#16156=ORIENTED_EDGE('',*,*,#12455,.T.);
#16157=ORIENTED_EDGE('',*,*,#12458,.T.);
#16158=ORIENTED_EDGE('',*,*,#12461,.T.);
#16159=ORIENTED_EDGE('',*,*,#12469,.T.);
#16160=ORIENTED_EDGE('',*,*,#12468,.T.);
#16161=ORIENTED_EDGE('',*,*,#12470,.F.);
#16162=ORIENTED_EDGE('',*,*,#12471,.F.);
#16163=ORIENTED_EDGE('',*,*,#12472,.T.);
#16164=ORIENTED_EDGE('',*,*,#12471,.T.);
#16165=ORIENTED_EDGE('',*,*,#12473,.F.);
#16166=ORIENTED_EDGE('',*,*,#12463,.F.);
#16167=ORIENTED_EDGE('',*,*,#12459,.T.);
#16168=ORIENTED_EDGE('',*,*,#12473,.T.);
#16169=ORIENTED_EDGE('',*,*,#12470,.T.);
#16170=ORIENTED_EDGE('',*,*,#12467,.T.);
#16171=ORIENTED_EDGE('',*,*,#12464,.T.);
#16172=ORIENTED_EDGE('',*,*,#12440,.T.);
#16173=ORIENTED_EDGE('',*,*,#12443,.T.);
#16174=ORIENTED_EDGE('',*,*,#12446,.T.);
#16175=ORIENTED_EDGE('',*,*,#12449,.T.);
#16176=ORIENTED_EDGE('',*,*,#12472,.F.);
#16177=ORIENTED_EDGE('',*,*,#12462,.F.);
#16178=ORIENTED_EDGE('',*,*,#12466,.F.);
#16179=ORIENTED_EDGE('',*,*,#12469,.F.);
#16180=ORIENTED_EDGE('',*,*,#12474,.F.);
#16181=ORIENTED_EDGE('',*,*,#12475,.T.);
#16182=ORIENTED_EDGE('',*,*,#12476,.F.);
#16183=ORIENTED_EDGE('',*,*,#12477,.F.);
#16184=ORIENTED_EDGE('',*,*,#12478,.T.);
#16185=ORIENTED_EDGE('',*,*,#12479,.F.);
#16186=ORIENTED_EDGE('',*,*,#12478,.F.);
#16187=ORIENTED_EDGE('',*,*,#12480,.F.);
#16188=ORIENTED_EDGE('',*,*,#12481,.F.);
#16189=ORIENTED_EDGE('',*,*,#12475,.F.);
#16190=ORIENTED_EDGE('',*,*,#12482,.F.);
#16191=ORIENTED_EDGE('',*,*,#12483,.T.);
#16192=ORIENTED_EDGE('',*,*,#12484,.F.);
#16193=ORIENTED_EDGE('',*,*,#12485,.F.);
#16194=ORIENTED_EDGE('',*,*,#12486,.T.);
#16195=ORIENTED_EDGE('',*,*,#12487,.F.);
#16196=ORIENTED_EDGE('',*,*,#12486,.F.);
#16197=ORIENTED_EDGE('',*,*,#12488,.F.);
#16198=ORIENTED_EDGE('',*,*,#12489,.F.);
#16199=ORIENTED_EDGE('',*,*,#12483,.F.);
#16200=ORIENTED_EDGE('',*,*,#12490,.F.);
#16201=ORIENTED_EDGE('',*,*,#12491,.T.);
#16202=ORIENTED_EDGE('',*,*,#12492,.F.);
#16203=ORIENTED_EDGE('',*,*,#12493,.F.);
#16204=ORIENTED_EDGE('',*,*,#12494,.T.);
#16205=ORIENTED_EDGE('',*,*,#12495,.F.);
#16206=ORIENTED_EDGE('',*,*,#12494,.F.);
#16207=ORIENTED_EDGE('',*,*,#12496,.F.);
#16208=ORIENTED_EDGE('',*,*,#12497,.F.);
#16209=ORIENTED_EDGE('',*,*,#12491,.F.);
#16210=ORIENTED_EDGE('',*,*,#12498,.F.);
#16211=ORIENTED_EDGE('',*,*,#12499,.T.);
#16212=ORIENTED_EDGE('',*,*,#12500,.F.);
#16213=ORIENTED_EDGE('',*,*,#12501,.F.);
#16214=ORIENTED_EDGE('',*,*,#12502,.T.);
#16215=ORIENTED_EDGE('',*,*,#12503,.F.);
#16216=ORIENTED_EDGE('',*,*,#12502,.F.);
#16217=ORIENTED_EDGE('',*,*,#12504,.F.);
#16218=ORIENTED_EDGE('',*,*,#12505,.F.);
#16219=ORIENTED_EDGE('',*,*,#12499,.F.);
#16220=ORIENTED_EDGE('',*,*,#12476,.T.);
#16221=ORIENTED_EDGE('',*,*,#12474,.T.);
#16222=ORIENTED_EDGE('',*,*,#12481,.T.);
#16223=ORIENTED_EDGE('',*,*,#12506,.T.);
#16224=ORIENTED_EDGE('',*,*,#12492,.T.);
#16225=ORIENTED_EDGE('',*,*,#12490,.T.);
#16226=ORIENTED_EDGE('',*,*,#12497,.T.);
#16227=ORIENTED_EDGE('',*,*,#12507,.T.);
#16228=ORIENTED_EDGE('',*,*,#12508,.F.);
#16229=ORIENTED_EDGE('',*,*,#12509,.T.);
#16230=ORIENTED_EDGE('',*,*,#12510,.F.);
#16231=ORIENTED_EDGE('',*,*,#12511,.T.);
#16232=ORIENTED_EDGE('',*,*,#12484,.T.);
#16233=ORIENTED_EDGE('',*,*,#12482,.T.);
#16234=ORIENTED_EDGE('',*,*,#12489,.T.);
#16235=ORIENTED_EDGE('',*,*,#12512,.T.);
#16236=ORIENTED_EDGE('',*,*,#12500,.T.);
#16237=ORIENTED_EDGE('',*,*,#12498,.T.);
#16238=ORIENTED_EDGE('',*,*,#12505,.T.);
#16239=ORIENTED_EDGE('',*,*,#12513,.T.);
#16240=ORIENTED_EDGE('',*,*,#12514,.F.);
#16241=ORIENTED_EDGE('',*,*,#12515,.F.);
#16242=ORIENTED_EDGE('',*,*,#12516,.F.);
#16243=ORIENTED_EDGE('',*,*,#12517,.T.);
#16244=ORIENTED_EDGE('',*,*,#12508,.T.);
#16245=ORIENTED_EDGE('',*,*,#12518,.T.);
#16246=ORIENTED_EDGE('',*,*,#12519,.T.);
#16247=ORIENTED_EDGE('',*,*,#12520,.T.);
#16248=ORIENTED_EDGE('',*,*,#12521,.T.);
#16249=ORIENTED_EDGE('',*,*,#12522,.T.);
#16250=ORIENTED_EDGE('',*,*,#12516,.T.);
#16251=ORIENTED_EDGE('',*,*,#12523,.T.);
#16252=ORIENTED_EDGE('',*,*,#12524,.T.);
#16253=ORIENTED_EDGE('',*,*,#12525,.T.);
#16254=ORIENTED_EDGE('',*,*,#12526,.T.);
#16255=ORIENTED_EDGE('',*,*,#12527,.T.);
#16256=ORIENTED_EDGE('',*,*,#12480,.T.);
#16257=ORIENTED_EDGE('',*,*,#12477,.T.);
#16258=ORIENTED_EDGE('',*,*,#12511,.F.);
#16259=ORIENTED_EDGE('',*,*,#12528,.F.);
#16260=ORIENTED_EDGE('',*,*,#12529,.F.);
#16261=ORIENTED_EDGE('',*,*,#12518,.F.);
#16262=ORIENTED_EDGE('',*,*,#12507,.F.);
#16263=ORIENTED_EDGE('',*,*,#12496,.T.);
#16264=ORIENTED_EDGE('',*,*,#12493,.T.);
#16265=ORIENTED_EDGE('',*,*,#12506,.F.);
#16266=ORIENTED_EDGE('',*,*,#12529,.T.);
#16267=ORIENTED_EDGE('',*,*,#12530,.F.);
#16268=ORIENTED_EDGE('',*,*,#12531,.F.);
#16269=ORIENTED_EDGE('',*,*,#12519,.F.);
#16270=ORIENTED_EDGE('',*,*,#12531,.T.);
#16271=ORIENTED_EDGE('',*,*,#12532,.F.);
#16272=ORIENTED_EDGE('',*,*,#12533,.F.);
#16273=ORIENTED_EDGE('',*,*,#12520,.F.);
#16274=ORIENTED_EDGE('',*,*,#12479,.T.);
#16275=ORIENTED_EDGE('',*,*,#12487,.T.);
#16276=ORIENTED_EDGE('',*,*,#12495,.T.);
#16277=ORIENTED_EDGE('',*,*,#12503,.T.);
#16278=ORIENTED_EDGE('',*,*,#12533,.T.);
#16279=ORIENTED_EDGE('',*,*,#12534,.F.);
#16280=ORIENTED_EDGE('',*,*,#12535,.F.);
#16281=ORIENTED_EDGE('',*,*,#12521,.F.);
#16282=ORIENTED_EDGE('',*,*,#12488,.T.);
#16283=ORIENTED_EDGE('',*,*,#12485,.T.);
#16284=ORIENTED_EDGE('',*,*,#12517,.F.);
#16285=ORIENTED_EDGE('',*,*,#12522,.F.);
#16286=ORIENTED_EDGE('',*,*,#12535,.T.);
#16287=ORIENTED_EDGE('',*,*,#12536,.F.);
#16288=ORIENTED_EDGE('',*,*,#12513,.F.);
#16289=ORIENTED_EDGE('',*,*,#12504,.T.);
#16290=ORIENTED_EDGE('',*,*,#12501,.T.);
#16291=ORIENTED_EDGE('',*,*,#12512,.F.);
#16292=ORIENTED_EDGE('',*,*,#12515,.T.);
#16293=ORIENTED_EDGE('',*,*,#12537,.F.);
#16294=ORIENTED_EDGE('',*,*,#12538,.F.);
#16295=ORIENTED_EDGE('',*,*,#12523,.F.);
#16296=ORIENTED_EDGE('',*,*,#12538,.T.);
#16297=ORIENTED_EDGE('',*,*,#12539,.F.);
#16298=ORIENTED_EDGE('',*,*,#12540,.F.);
#16299=ORIENTED_EDGE('',*,*,#12524,.F.);
#16300=ORIENTED_EDGE('',*,*,#12540,.T.);
#16301=ORIENTED_EDGE('',*,*,#12541,.F.);
#16302=ORIENTED_EDGE('',*,*,#12542,.F.);
#16303=ORIENTED_EDGE('',*,*,#12525,.F.);
#16304=ORIENTED_EDGE('',*,*,#12542,.T.);
#16305=ORIENTED_EDGE('',*,*,#12543,.F.);
#16306=ORIENTED_EDGE('',*,*,#12544,.F.);
#16307=ORIENTED_EDGE('',*,*,#12526,.F.);
#16308=ORIENTED_EDGE('',*,*,#12544,.T.);
#16309=ORIENTED_EDGE('',*,*,#12545,.F.);
#16310=ORIENTED_EDGE('',*,*,#12509,.F.);
#16311=ORIENTED_EDGE('',*,*,#12527,.F.);
#16312=ORIENTED_EDGE('',*,*,#12510,.T.);
#16313=ORIENTED_EDGE('',*,*,#12545,.T.);
#16314=ORIENTED_EDGE('',*,*,#12543,.T.);
#16315=ORIENTED_EDGE('',*,*,#12541,.T.);
#16316=ORIENTED_EDGE('',*,*,#12539,.T.);
#16317=ORIENTED_EDGE('',*,*,#12537,.T.);
#16318=ORIENTED_EDGE('',*,*,#12514,.T.);
#16319=ORIENTED_EDGE('',*,*,#12536,.T.);
#16320=ORIENTED_EDGE('',*,*,#12534,.T.);
#16321=ORIENTED_EDGE('',*,*,#12532,.T.);
#16322=ORIENTED_EDGE('',*,*,#12530,.T.);
#16323=ORIENTED_EDGE('',*,*,#12528,.T.);
#16324=ORIENTED_EDGE('',*,*,#12546,.T.);
#16325=ORIENTED_EDGE('',*,*,#12547,.T.);
#16326=ORIENTED_EDGE('',*,*,#12548,.F.);
#16327=ORIENTED_EDGE('',*,*,#12549,.F.);
#16328=ORIENTED_EDGE('',*,*,#12550,.T.);
#16329=ORIENTED_EDGE('',*,*,#12549,.T.);
#16330=ORIENTED_EDGE('',*,*,#12551,.F.);
#16331=ORIENTED_EDGE('',*,*,#12552,.F.);
#16332=ORIENTED_EDGE('',*,*,#12553,.T.);
#16333=ORIENTED_EDGE('',*,*,#12552,.T.);
#16334=ORIENTED_EDGE('',*,*,#12554,.F.);
#16335=ORIENTED_EDGE('',*,*,#12555,.F.);
#16336=ORIENTED_EDGE('',*,*,#12556,.T.);
#16337=ORIENTED_EDGE('',*,*,#12555,.T.);
#16338=ORIENTED_EDGE('',*,*,#12557,.F.);
#16339=ORIENTED_EDGE('',*,*,#12558,.F.);
#16340=ORIENTED_EDGE('',*,*,#12559,.T.);
#16341=ORIENTED_EDGE('',*,*,#12558,.T.);
#16342=ORIENTED_EDGE('',*,*,#12560,.F.);
#16343=ORIENTED_EDGE('',*,*,#12561,.F.);
#16344=ORIENTED_EDGE('',*,*,#12562,.T.);
#16345=ORIENTED_EDGE('',*,*,#12561,.T.);
#16346=ORIENTED_EDGE('',*,*,#12563,.F.);
#16347=ORIENTED_EDGE('',*,*,#12564,.F.);
#16348=ORIENTED_EDGE('',*,*,#12565,.T.);
#16349=ORIENTED_EDGE('',*,*,#12564,.T.);
#16350=ORIENTED_EDGE('',*,*,#12566,.F.);
#16351=ORIENTED_EDGE('',*,*,#12567,.F.);
#16352=ORIENTED_EDGE('',*,*,#12568,.T.);
#16353=ORIENTED_EDGE('',*,*,#12567,.T.);
#16354=ORIENTED_EDGE('',*,*,#12569,.F.);
#16355=ORIENTED_EDGE('',*,*,#12547,.F.);
#16356=ORIENTED_EDGE('',*,*,#12569,.T.);
#16357=ORIENTED_EDGE('',*,*,#12566,.T.);
#16358=ORIENTED_EDGE('',*,*,#12563,.T.);
#16359=ORIENTED_EDGE('',*,*,#12560,.T.);
#16360=ORIENTED_EDGE('',*,*,#12557,.T.);
#16361=ORIENTED_EDGE('',*,*,#12554,.T.);
#16362=ORIENTED_EDGE('',*,*,#12551,.T.);
#16363=ORIENTED_EDGE('',*,*,#12548,.T.);
#16364=ORIENTED_EDGE('',*,*,#12568,.F.);
#16365=ORIENTED_EDGE('',*,*,#12546,.F.);
#16366=ORIENTED_EDGE('',*,*,#12550,.F.);
#16367=ORIENTED_EDGE('',*,*,#12553,.F.);
#16368=ORIENTED_EDGE('',*,*,#12556,.F.);
#16369=ORIENTED_EDGE('',*,*,#12559,.F.);
#16370=ORIENTED_EDGE('',*,*,#12562,.F.);
#16371=ORIENTED_EDGE('',*,*,#12565,.F.);
#16372=ORIENTED_EDGE('',*,*,#12570,.F.);
#16373=ORIENTED_EDGE('',*,*,#12571,.T.);
#16374=ORIENTED_EDGE('',*,*,#12572,.F.);
#16375=ORIENTED_EDGE('',*,*,#12573,.F.);
#16376=ORIENTED_EDGE('',*,*,#12574,.F.);
#16377=ORIENTED_EDGE('',*,*,#12573,.T.);
#16378=ORIENTED_EDGE('',*,*,#12575,.F.);
#16379=ORIENTED_EDGE('',*,*,#12576,.F.);
#16380=ORIENTED_EDGE('',*,*,#12577,.F.);
#16381=ORIENTED_EDGE('',*,*,#12576,.T.);
#16382=ORIENTED_EDGE('',*,*,#12578,.F.);
#16383=ORIENTED_EDGE('',*,*,#12579,.F.);
#16384=ORIENTED_EDGE('',*,*,#12580,.F.);
#16385=ORIENTED_EDGE('',*,*,#12579,.T.);
#16386=ORIENTED_EDGE('',*,*,#12581,.F.);
#16387=ORIENTED_EDGE('',*,*,#12582,.F.);
#16388=ORIENTED_EDGE('',*,*,#12583,.F.);
#16389=ORIENTED_EDGE('',*,*,#12582,.T.);
#16390=ORIENTED_EDGE('',*,*,#12584,.F.);
#16391=ORIENTED_EDGE('',*,*,#12585,.F.);
#16392=ORIENTED_EDGE('',*,*,#12586,.F.);
#16393=ORIENTED_EDGE('',*,*,#12585,.T.);
#16394=ORIENTED_EDGE('',*,*,#12587,.F.);
#16395=ORIENTED_EDGE('',*,*,#12588,.F.);
#16396=ORIENTED_EDGE('',*,*,#12589,.F.);
#16397=ORIENTED_EDGE('',*,*,#12588,.T.);
#16398=ORIENTED_EDGE('',*,*,#12590,.F.);
#16399=ORIENTED_EDGE('',*,*,#12591,.F.);
#16400=ORIENTED_EDGE('',*,*,#12592,.F.);
#16401=ORIENTED_EDGE('',*,*,#12591,.T.);
#16402=ORIENTED_EDGE('',*,*,#12593,.F.);
#16403=ORIENTED_EDGE('',*,*,#12571,.F.);
#16404=ORIENTED_EDGE('',*,*,#12592,.T.);
#16405=ORIENTED_EDGE('',*,*,#12570,.T.);
#16406=ORIENTED_EDGE('',*,*,#12574,.T.);
#16407=ORIENTED_EDGE('',*,*,#12577,.T.);
#16408=ORIENTED_EDGE('',*,*,#12580,.T.);
#16409=ORIENTED_EDGE('',*,*,#12583,.T.);
#16410=ORIENTED_EDGE('',*,*,#12586,.T.);
#16411=ORIENTED_EDGE('',*,*,#12589,.T.);
#16412=ORIENTED_EDGE('',*,*,#12593,.T.);
#16413=ORIENTED_EDGE('',*,*,#12590,.T.);
#16414=ORIENTED_EDGE('',*,*,#12587,.T.);
#16415=ORIENTED_EDGE('',*,*,#12584,.T.);
#16416=ORIENTED_EDGE('',*,*,#12581,.T.);
#16417=ORIENTED_EDGE('',*,*,#12578,.T.);
#16418=ORIENTED_EDGE('',*,*,#12575,.T.);
#16419=ORIENTED_EDGE('',*,*,#12572,.T.);
#16420=ORIENTED_EDGE('',*,*,#12594,.T.);
#16421=ORIENTED_EDGE('',*,*,#12595,.T.);
#16422=ORIENTED_EDGE('',*,*,#12596,.T.);
#16423=ORIENTED_EDGE('',*,*,#12595,.F.);
#16424=ORIENTED_EDGE('',*,*,#12596,.F.);
#16425=ORIENTED_EDGE('',*,*,#12597,.T.);
#16426=ORIENTED_EDGE('',*,*,#12598,.T.);
#16427=ORIENTED_EDGE('',*,*,#12597,.F.);
#16428=ORIENTED_EDGE('',*,*,#12599,.T.);
#16429=ORIENTED_EDGE('',*,*,#12594,.F.);
#16430=ORIENTED_EDGE('',*,*,#12599,.F.);
#16431=ORIENTED_EDGE('',*,*,#12600,.T.);
#16432=ORIENTED_EDGE('',*,*,#12601,.T.);
#16433=ORIENTED_EDGE('',*,*,#12600,.F.);
#16434=ORIENTED_EDGE('',*,*,#12601,.F.);
#16435=ORIENTED_EDGE('',*,*,#12598,.F.);
#16436=ORIENTED_EDGE('',*,*,#12602,.T.);
#16437=ORIENTED_EDGE('',*,*,#12603,.T.);
#16438=ORIENTED_EDGE('',*,*,#12604,.T.);
#16439=ORIENTED_EDGE('',*,*,#12605,.F.);
#16440=ORIENTED_EDGE('',*,*,#12606,.T.);
#16441=ORIENTED_EDGE('',*,*,#12607,.T.);
#16442=ORIENTED_EDGE('',*,*,#12608,.T.);
#16443=ORIENTED_EDGE('',*,*,#12603,.F.);
#16444=ORIENTED_EDGE('',*,*,#12609,.T.);
#16445=ORIENTED_EDGE('',*,*,#12610,.T.);
#16446=ORIENTED_EDGE('',*,*,#12611,.T.);
#16447=ORIENTED_EDGE('',*,*,#12607,.F.);
#16448=ORIENTED_EDGE('',*,*,#12612,.T.);
#16449=ORIENTED_EDGE('',*,*,#12613,.T.);
#16450=ORIENTED_EDGE('',*,*,#12614,.T.);
#16451=ORIENTED_EDGE('',*,*,#12610,.F.);
#16452=ORIENTED_EDGE('',*,*,#12615,.T.);
#16453=ORIENTED_EDGE('',*,*,#12616,.T.);
#16454=ORIENTED_EDGE('',*,*,#12617,.T.);
#16455=ORIENTED_EDGE('',*,*,#12613,.F.);
#16456=ORIENTED_EDGE('',*,*,#12618,.T.);
#16457=ORIENTED_EDGE('',*,*,#12605,.T.);
#16458=ORIENTED_EDGE('',*,*,#12619,.T.);
#16459=ORIENTED_EDGE('',*,*,#12616,.F.);
#16460=ORIENTED_EDGE('',*,*,#12618,.F.);
#16461=ORIENTED_EDGE('',*,*,#12615,.F.);
#16462=ORIENTED_EDGE('',*,*,#12612,.F.);
#16463=ORIENTED_EDGE('',*,*,#12609,.F.);
#16464=ORIENTED_EDGE('',*,*,#12606,.F.);
#16465=ORIENTED_EDGE('',*,*,#12602,.F.);
#16466=ORIENTED_EDGE('',*,*,#12619,.F.);
#16467=ORIENTED_EDGE('',*,*,#12604,.F.);
#16468=ORIENTED_EDGE('',*,*,#12608,.F.);
#16469=ORIENTED_EDGE('',*,*,#12611,.F.);
#16470=ORIENTED_EDGE('',*,*,#12614,.F.);
#16471=ORIENTED_EDGE('',*,*,#12617,.F.);
#16472=ORIENTED_EDGE('',*,*,#12620,.T.);
#16473=ORIENTED_EDGE('',*,*,#12621,.F.);
#16474=ORIENTED_EDGE('',*,*,#12620,.F.);
#16475=ORIENTED_EDGE('',*,*,#12622,.T.);
#16476=ORIENTED_EDGE('',*,*,#12623,.T.);
#16477=ORIENTED_EDGE('',*,*,#12622,.F.);
#16478=ORIENTED_EDGE('',*,*,#12623,.F.);
#16479=ORIENTED_EDGE('',*,*,#12624,.F.);
#16480=ORIENTED_EDGE('',*,*,#12625,.F.);
#16481=ORIENTED_EDGE('',*,*,#12626,.T.);
#16482=ORIENTED_EDGE('',*,*,#12624,.T.);
#16483=ORIENTED_EDGE('',*,*,#12626,.F.);
#16484=ORIENTED_EDGE('',*,*,#12627,.F.);
#16485=ORIENTED_EDGE('',*,*,#12628,.T.);
#16486=ORIENTED_EDGE('',*,*,#12625,.T.);
#16487=ORIENTED_EDGE('',*,*,#12628,.F.);
#16488=ORIENTED_EDGE('',*,*,#12629,.F.);
#16489=ORIENTED_EDGE('',*,*,#12630,.T.);
#16490=ORIENTED_EDGE('',*,*,#12627,.T.);
#16491=ORIENTED_EDGE('',*,*,#12630,.F.);
#16492=ORIENTED_EDGE('',*,*,#12629,.T.);
#16493=ORIENTED_EDGE('',*,*,#12631,.F.);
#16494=ORIENTED_EDGE('',*,*,#12632,.F.);
#16495=ORIENTED_EDGE('',*,*,#12633,.T.);
#16496=ORIENTED_EDGE('',*,*,#12631,.T.);
#16497=ORIENTED_EDGE('',*,*,#12633,.F.);
#16498=ORIENTED_EDGE('',*,*,#12621,.T.);
#16499=ORIENTED_EDGE('',*,*,#12634,.T.);
#16500=ORIENTED_EDGE('',*,*,#12632,.T.);
#16501=ORIENTED_EDGE('',*,*,#12634,.F.);
#16502=ORIENTED_EDGE('',*,*,#12635,.T.);
#16503=ORIENTED_EDGE('',*,*,#12636,.T.);
#16504=ORIENTED_EDGE('',*,*,#12637,.T.);
#16505=ORIENTED_EDGE('',*,*,#12638,.T.);
#16506=ORIENTED_EDGE('',*,*,#12639,.T.);
#16507=ORIENTED_EDGE('',*,*,#12640,.T.);
#16508=ORIENTED_EDGE('',*,*,#12635,.F.);
#16509=ORIENTED_EDGE('',*,*,#12641,.T.);
#16510=ORIENTED_EDGE('',*,*,#12642,.T.);
#16511=ORIENTED_EDGE('',*,*,#12643,.T.);
#16512=ORIENTED_EDGE('',*,*,#12639,.F.);
#16513=ORIENTED_EDGE('',*,*,#12644,.T.);
#16514=ORIENTED_EDGE('',*,*,#12645,.T.);
#16515=ORIENTED_EDGE('',*,*,#12646,.T.);
#16516=ORIENTED_EDGE('',*,*,#12642,.F.);
#16517=ORIENTED_EDGE('',*,*,#12647,.T.);
#16518=ORIENTED_EDGE('',*,*,#12648,.T.);
#16519=ORIENTED_EDGE('',*,*,#12649,.T.);
#16520=ORIENTED_EDGE('',*,*,#12645,.F.);
#16521=ORIENTED_EDGE('',*,*,#12650,.T.);
#16522=ORIENTED_EDGE('',*,*,#12651,.T.);
#16523=ORIENTED_EDGE('',*,*,#12652,.T.);
#16524=ORIENTED_EDGE('',*,*,#12648,.F.);
#16525=ORIENTED_EDGE('',*,*,#12653,.T.);
#16526=ORIENTED_EDGE('',*,*,#12654,.T.);
#16527=ORIENTED_EDGE('',*,*,#12655,.T.);
#16528=ORIENTED_EDGE('',*,*,#12651,.F.);
#16529=ORIENTED_EDGE('',*,*,#12656,.T.);
#16530=ORIENTED_EDGE('',*,*,#12657,.T.);
#16531=ORIENTED_EDGE('',*,*,#12658,.T.);
#16532=ORIENTED_EDGE('',*,*,#12654,.F.);
#16533=ORIENTED_EDGE('',*,*,#12659,.T.);
#16534=ORIENTED_EDGE('',*,*,#12660,.F.);
#16535=ORIENTED_EDGE('',*,*,#12661,.F.);
#16536=ORIENTED_EDGE('',*,*,#12662,.T.);
#16537=ORIENTED_EDGE('',*,*,#12663,.T.);
#16538=ORIENTED_EDGE('',*,*,#12664,.T.);
#16539=ORIENTED_EDGE('',*,*,#12665,.F.);
#16540=ORIENTED_EDGE('',*,*,#12666,.F.);
#16541=ORIENTED_EDGE('',*,*,#12667,.T.);
#16542=ORIENTED_EDGE('',*,*,#12668,.T.);
#16543=ORIENTED_EDGE('',*,*,#12663,.F.);
#16544=ORIENTED_EDGE('',*,*,#12669,.F.);
#16545=ORIENTED_EDGE('',*,*,#12670,.T.);
#16546=ORIENTED_EDGE('',*,*,#12671,.T.);
#16547=ORIENTED_EDGE('',*,*,#12667,.F.);
#16548=ORIENTED_EDGE('',*,*,#12672,.F.);
#16549=ORIENTED_EDGE('',*,*,#12673,.T.);
#16550=ORIENTED_EDGE('',*,*,#12674,.T.);
#16551=ORIENTED_EDGE('',*,*,#12670,.F.);
#16552=ORIENTED_EDGE('',*,*,#12675,.F.);
#16553=ORIENTED_EDGE('',*,*,#12676,.T.);
#16554=ORIENTED_EDGE('',*,*,#12677,.T.);
#16555=ORIENTED_EDGE('',*,*,#12673,.F.);
#16556=ORIENTED_EDGE('',*,*,#12678,.F.);
#16557=ORIENTED_EDGE('',*,*,#12679,.T.);
#16558=ORIENTED_EDGE('',*,*,#12680,.T.);
#16559=ORIENTED_EDGE('',*,*,#12676,.F.);
#16560=ORIENTED_EDGE('',*,*,#12681,.F.);
#16561=ORIENTED_EDGE('',*,*,#12682,.T.);
#16562=ORIENTED_EDGE('',*,*,#12683,.T.);
#16563=ORIENTED_EDGE('',*,*,#12679,.F.);
#16564=ORIENTED_EDGE('',*,*,#12684,.F.);
#16565=ORIENTED_EDGE('',*,*,#12685,.T.);
#16566=ORIENTED_EDGE('',*,*,#12686,.T.);
#16567=ORIENTED_EDGE('',*,*,#12682,.F.);
#16568=ORIENTED_EDGE('',*,*,#12687,.F.);
#16569=ORIENTED_EDGE('',*,*,#12688,.F.);
#16570=ORIENTED_EDGE('',*,*,#12689,.F.);
#16571=ORIENTED_EDGE('',*,*,#12690,.F.);
#16572=ORIENTED_EDGE('',*,*,#12691,.T.);
#16573=ORIENTED_EDGE('',*,*,#12688,.T.);
#16574=ORIENTED_EDGE('',*,*,#12692,.T.);
#16575=ORIENTED_EDGE('',*,*,#12685,.F.);
#16576=ORIENTED_EDGE('',*,*,#12693,.F.);
#16577=ORIENTED_EDGE('',*,*,#12694,.F.);
#16578=ORIENTED_EDGE('',*,*,#12664,.F.);
#16579=ORIENTED_EDGE('',*,*,#12668,.F.);
#16580=ORIENTED_EDGE('',*,*,#12671,.F.);
#16581=ORIENTED_EDGE('',*,*,#12674,.F.);
#16582=ORIENTED_EDGE('',*,*,#12677,.F.);
#16583=ORIENTED_EDGE('',*,*,#12680,.F.);
#16584=ORIENTED_EDGE('',*,*,#12683,.F.);
#16585=ORIENTED_EDGE('',*,*,#12686,.F.);
#16586=ORIENTED_EDGE('',*,*,#12692,.F.);
#16587=ORIENTED_EDGE('',*,*,#12691,.F.);
#16588=ORIENTED_EDGE('',*,*,#12695,.F.);
#16589=ORIENTED_EDGE('',*,*,#12636,.F.);
#16590=ORIENTED_EDGE('',*,*,#12640,.F.);
#16591=ORIENTED_EDGE('',*,*,#12643,.F.);
#16592=ORIENTED_EDGE('',*,*,#12646,.F.);
#16593=ORIENTED_EDGE('',*,*,#12649,.F.);
#16594=ORIENTED_EDGE('',*,*,#12652,.F.);
#16595=ORIENTED_EDGE('',*,*,#12655,.F.);
#16596=ORIENTED_EDGE('',*,*,#12658,.F.);
#16597=ORIENTED_EDGE('',*,*,#12696,.F.);
#16598=ORIENTED_EDGE('',*,*,#12662,.F.);
#16599=ORIENTED_EDGE('',*,*,#12697,.F.);
#16600=ORIENTED_EDGE('',*,*,#12698,.F.);
#16601=ORIENTED_EDGE('',*,*,#12659,.F.);
#16602=ORIENTED_EDGE('',*,*,#12656,.F.);
#16603=ORIENTED_EDGE('',*,*,#12653,.F.);
#16604=ORIENTED_EDGE('',*,*,#12650,.F.);
#16605=ORIENTED_EDGE('',*,*,#12647,.F.);
#16606=ORIENTED_EDGE('',*,*,#12644,.F.);
#16607=ORIENTED_EDGE('',*,*,#12641,.F.);
#16608=ORIENTED_EDGE('',*,*,#12638,.F.);
#16609=ORIENTED_EDGE('',*,*,#12699,.F.);
#16610=ORIENTED_EDGE('',*,*,#12689,.T.);
#16611=ORIENTED_EDGE('',*,*,#12693,.T.);
#16612=ORIENTED_EDGE('',*,*,#12687,.T.);
#16613=ORIENTED_EDGE('',*,*,#12684,.T.);
#16614=ORIENTED_EDGE('',*,*,#12681,.T.);
#16615=ORIENTED_EDGE('',*,*,#12678,.T.);
#16616=ORIENTED_EDGE('',*,*,#12675,.T.);
#16617=ORIENTED_EDGE('',*,*,#12672,.T.);
#16618=ORIENTED_EDGE('',*,*,#12669,.T.);
#16619=ORIENTED_EDGE('',*,*,#12666,.T.);
#16620=ORIENTED_EDGE('',*,*,#12700,.T.);
#16621=ORIENTED_EDGE('',*,*,#12701,.T.);
#16622=ORIENTED_EDGE('',*,*,#12697,.T.);
#16623=ORIENTED_EDGE('',*,*,#12665,.T.);
#16624=ORIENTED_EDGE('',*,*,#12694,.T.);
#16625=ORIENTED_EDGE('',*,*,#12661,.T.);
#16626=ORIENTED_EDGE('',*,*,#12702,.T.);
#16627=ORIENTED_EDGE('',*,*,#12703,.T.);
#16628=ORIENTED_EDGE('',*,*,#12704,.T.);
#16629=ORIENTED_EDGE('',*,*,#12705,.T.);
#16630=ORIENTED_EDGE('',*,*,#12706,.F.);
#16631=ORIENTED_EDGE('',*,*,#12707,.T.);
#16632=ORIENTED_EDGE('',*,*,#12705,.F.);
#16633=ORIENTED_EDGE('',*,*,#12707,.F.);
#16634=ORIENTED_EDGE('',*,*,#12708,.F.);
#16635=ORIENTED_EDGE('',*,*,#12709,.T.);
#16636=ORIENTED_EDGE('',*,*,#12704,.F.);
#16637=ORIENTED_EDGE('',*,*,#12709,.F.);
#16638=ORIENTED_EDGE('',*,*,#12710,.F.);
#16639=ORIENTED_EDGE('',*,*,#12711,.T.);
#16640=ORIENTED_EDGE('',*,*,#12703,.F.);
#16641=ORIENTED_EDGE('',*,*,#12711,.F.);
#16642=ORIENTED_EDGE('',*,*,#12712,.F.);
#16643=ORIENTED_EDGE('',*,*,#12713,.F.);
#16644=ORIENTED_EDGE('',*,*,#12700,.F.);
#16645=ORIENTED_EDGE('',*,*,#12714,.F.);
#16646=ORIENTED_EDGE('',*,*,#12712,.T.);
#16647=ORIENTED_EDGE('',*,*,#12715,.F.);
#16648=ORIENTED_EDGE('',*,*,#12706,.T.);
#16649=ORIENTED_EDGE('',*,*,#12708,.T.);
#16650=ORIENTED_EDGE('',*,*,#12710,.T.);
#16651=ORIENTED_EDGE('',*,*,#12716,.T.);
#16652=ORIENTED_EDGE('',*,*,#12714,.T.);
#16653=ORIENTED_EDGE('',*,*,#12701,.F.);
#16654=ORIENTED_EDGE('',*,*,#12713,.T.);
#16655=ORIENTED_EDGE('',*,*,#12715,.T.);
#16656=ORIENTED_EDGE('',*,*,#12660,.T.);
#16657=ORIENTED_EDGE('',*,*,#12696,.T.);
#16658=ORIENTED_EDGE('',*,*,#12657,.F.);
#16659=ORIENTED_EDGE('',*,*,#12698,.T.);
#16660=ORIENTED_EDGE('',*,*,#12702,.F.);
#16661=ORIENTED_EDGE('',*,*,#12716,.F.);
#16662=ORIENTED_EDGE('',*,*,#12717,.T.);
#16663=ORIENTED_EDGE('',*,*,#12718,.T.);
#16664=ORIENTED_EDGE('',*,*,#12717,.F.);
#16665=ORIENTED_EDGE('',*,*,#12718,.F.);
#16666=ORIENTED_EDGE('',*,*,#12699,.T.);
#16667=ORIENTED_EDGE('',*,*,#12637,.F.);
#16668=ORIENTED_EDGE('',*,*,#12695,.T.);
#16669=ORIENTED_EDGE('',*,*,#12690,.T.);
#16670=ORIENTED_EDGE('',*,*,#12719,.F.);
#16671=ORIENTED_EDGE('',*,*,#12720,.F.);
#16672=ORIENTED_EDGE('',*,*,#12721,.T.);
#16673=ORIENTED_EDGE('',*,*,#12719,.T.);
#16674=ORIENTED_EDGE('',*,*,#12721,.F.);
#16675=ORIENTED_EDGE('',*,*,#12722,.F.);
#16676=ORIENTED_EDGE('',*,*,#12723,.T.);
#16677=ORIENTED_EDGE('',*,*,#12720,.T.);
#16678=ORIENTED_EDGE('',*,*,#12723,.F.);
#16679=ORIENTED_EDGE('',*,*,#12724,.F.);
#16680=ORIENTED_EDGE('',*,*,#12725,.T.);
#16681=ORIENTED_EDGE('',*,*,#12722,.T.);
#16682=ORIENTED_EDGE('',*,*,#12725,.F.);
#16683=ORIENTED_EDGE('',*,*,#12724,.T.);
#16684=ORIENTED_EDGE('',*,*,#12726,.F.);
#16685=ORIENTED_EDGE('',*,*,#12727,.F.);
#16686=ORIENTED_EDGE('',*,*,#12728,.T.);
#16687=ORIENTED_EDGE('',*,*,#12726,.T.);
#16688=ORIENTED_EDGE('',*,*,#12728,.F.);
#16689=ORIENTED_EDGE('',*,*,#12729,.F.);
#16690=ORIENTED_EDGE('',*,*,#12730,.T.);
#16691=ORIENTED_EDGE('',*,*,#12727,.T.);
#16692=ORIENTED_EDGE('',*,*,#12730,.F.);
#16693=ORIENTED_EDGE('',*,*,#12731,.F.);
#16694=ORIENTED_EDGE('',*,*,#12732,.T.);
#16695=ORIENTED_EDGE('',*,*,#12729,.T.);
#16696=ORIENTED_EDGE('',*,*,#12732,.F.);
#16697=ORIENTED_EDGE('',*,*,#12731,.T.);
#16698=ORIENTED_EDGE('',*,*,#12733,.T.);
#16699=ORIENTED_EDGE('',*,*,#12734,.T.);
#16700=ORIENTED_EDGE('',*,*,#12735,.T.);
#16701=ORIENTED_EDGE('',*,*,#12736,.F.);
#16702=ORIENTED_EDGE('',*,*,#12737,.T.);
#16703=ORIENTED_EDGE('',*,*,#12738,.T.);
#16704=ORIENTED_EDGE('',*,*,#12739,.T.);
#16705=ORIENTED_EDGE('',*,*,#12734,.F.);
#16706=ORIENTED_EDGE('',*,*,#12740,.T.);
#16707=ORIENTED_EDGE('',*,*,#12741,.T.);
#16708=ORIENTED_EDGE('',*,*,#12742,.T.);
#16709=ORIENTED_EDGE('',*,*,#12738,.F.);
#16710=ORIENTED_EDGE('',*,*,#12743,.T.);
#16711=ORIENTED_EDGE('',*,*,#12744,.T.);
#16712=ORIENTED_EDGE('',*,*,#12745,.T.);
#16713=ORIENTED_EDGE('',*,*,#12741,.F.);
#16714=ORIENTED_EDGE('',*,*,#12746,.T.);
#16715=ORIENTED_EDGE('',*,*,#12747,.T.);
#16716=ORIENTED_EDGE('',*,*,#12748,.T.);
#16717=ORIENTED_EDGE('',*,*,#12744,.F.);
#16718=ORIENTED_EDGE('',*,*,#12749,.T.);
#16719=ORIENTED_EDGE('',*,*,#12736,.T.);
#16720=ORIENTED_EDGE('',*,*,#12750,.T.);
#16721=ORIENTED_EDGE('',*,*,#12747,.F.);
#16722=ORIENTED_EDGE('',*,*,#12749,.F.);
#16723=ORIENTED_EDGE('',*,*,#12746,.F.);
#16724=ORIENTED_EDGE('',*,*,#12743,.F.);
#16725=ORIENTED_EDGE('',*,*,#12740,.F.);
#16726=ORIENTED_EDGE('',*,*,#12737,.F.);
#16727=ORIENTED_EDGE('',*,*,#12733,.F.);
#16728=ORIENTED_EDGE('',*,*,#12750,.F.);
#16729=ORIENTED_EDGE('',*,*,#12735,.F.);
#16730=ORIENTED_EDGE('',*,*,#12739,.F.);
#16731=ORIENTED_EDGE('',*,*,#12742,.F.);
#16732=ORIENTED_EDGE('',*,*,#12745,.F.);
#16733=ORIENTED_EDGE('',*,*,#12748,.F.);
#16734=ORIENTED_EDGE('',*,*,#12751,.F.);
#16735=ORIENTED_EDGE('',*,*,#12752,.F.);
#16736=ORIENTED_EDGE('',*,*,#12753,.T.);
#16737=ORIENTED_EDGE('',*,*,#12751,.T.);
#16738=ORIENTED_EDGE('',*,*,#12753,.F.);
#16739=ORIENTED_EDGE('',*,*,#12754,.F.);
#16740=ORIENTED_EDGE('',*,*,#12755,.T.);
#16741=ORIENTED_EDGE('',*,*,#12752,.T.);
#16742=ORIENTED_EDGE('',*,*,#12755,.F.);
#16743=ORIENTED_EDGE('',*,*,#12756,.F.);
#16744=ORIENTED_EDGE('',*,*,#12757,.T.);
#16745=ORIENTED_EDGE('',*,*,#12754,.T.);
#16746=ORIENTED_EDGE('',*,*,#12757,.F.);
#16747=ORIENTED_EDGE('',*,*,#12756,.T.);
#16748=ORIENTED_EDGE('',*,*,#12758,.F.);
#16749=ORIENTED_EDGE('',*,*,#12759,.F.);
#16750=ORIENTED_EDGE('',*,*,#12760,.T.);
#16751=ORIENTED_EDGE('',*,*,#12758,.T.);
#16752=ORIENTED_EDGE('',*,*,#12760,.F.);
#16753=ORIENTED_EDGE('',*,*,#12761,.F.);
#16754=ORIENTED_EDGE('',*,*,#12762,.T.);
#16755=ORIENTED_EDGE('',*,*,#12759,.T.);
#16756=ORIENTED_EDGE('',*,*,#12762,.F.);
#16757=ORIENTED_EDGE('',*,*,#12763,.F.);
#16758=ORIENTED_EDGE('',*,*,#12764,.T.);
#16759=ORIENTED_EDGE('',*,*,#12761,.T.);
#16760=ORIENTED_EDGE('',*,*,#12764,.F.);
#16761=ORIENTED_EDGE('',*,*,#12763,.T.);
#16762=ORIENTED_EDGE('',*,*,#12765,.T.);
#16763=ORIENTED_EDGE('',*,*,#12766,.T.);
#16764=ORIENTED_EDGE('',*,*,#12767,.T.);
#16765=ORIENTED_EDGE('',*,*,#12768,.F.);
#16766=ORIENTED_EDGE('',*,*,#12769,.T.);
#16767=ORIENTED_EDGE('',*,*,#12770,.T.);
#16768=ORIENTED_EDGE('',*,*,#12771,.T.);
#16769=ORIENTED_EDGE('',*,*,#12766,.F.);
#16770=ORIENTED_EDGE('',*,*,#12772,.T.);
#16771=ORIENTED_EDGE('',*,*,#12773,.T.);
#16772=ORIENTED_EDGE('',*,*,#12774,.T.);
#16773=ORIENTED_EDGE('',*,*,#12770,.F.);
#16774=ORIENTED_EDGE('',*,*,#12775,.T.);
#16775=ORIENTED_EDGE('',*,*,#12776,.T.);
#16776=ORIENTED_EDGE('',*,*,#12777,.T.);
#16777=ORIENTED_EDGE('',*,*,#12773,.F.);
#16778=ORIENTED_EDGE('',*,*,#12778,.T.);
#16779=ORIENTED_EDGE('',*,*,#12779,.T.);
#16780=ORIENTED_EDGE('',*,*,#12780,.T.);
#16781=ORIENTED_EDGE('',*,*,#12776,.F.);
#16782=ORIENTED_EDGE('',*,*,#12781,.T.);
#16783=ORIENTED_EDGE('',*,*,#12768,.T.);
#16784=ORIENTED_EDGE('',*,*,#12782,.T.);
#16785=ORIENTED_EDGE('',*,*,#12779,.F.);
#16786=ORIENTED_EDGE('',*,*,#12781,.F.);
#16787=ORIENTED_EDGE('',*,*,#12778,.F.);
#16788=ORIENTED_EDGE('',*,*,#12775,.F.);
#16789=ORIENTED_EDGE('',*,*,#12772,.F.);
#16790=ORIENTED_EDGE('',*,*,#12769,.F.);
#16791=ORIENTED_EDGE('',*,*,#12765,.F.);
#16792=ORIENTED_EDGE('',*,*,#12782,.F.);
#16793=ORIENTED_EDGE('',*,*,#12767,.F.);
#16794=ORIENTED_EDGE('',*,*,#12771,.F.);
#16795=ORIENTED_EDGE('',*,*,#12774,.F.);
#16796=ORIENTED_EDGE('',*,*,#12777,.F.);
#16797=ORIENTED_EDGE('',*,*,#12780,.F.);
#16798=ORIENTED_EDGE('',*,*,#12783,.F.);
#16799=ORIENTED_EDGE('',*,*,#12784,.T.);
#16800=ORIENTED_EDGE('',*,*,#12785,.T.);
#16801=ORIENTED_EDGE('',*,*,#12786,.T.);
#16802=ORIENTED_EDGE('',*,*,#12787,.F.);
#16803=ORIENTED_EDGE('',*,*,#12788,.T.);
#16804=ORIENTED_EDGE('',*,*,#12783,.T.);
#16805=ORIENTED_EDGE('',*,*,#12789,.T.);
#16806=ORIENTED_EDGE('',*,*,#12790,.F.);
#16807=ORIENTED_EDGE('',*,*,#12791,.T.);
#16808=ORIENTED_EDGE('',*,*,#12787,.T.);
#16809=ORIENTED_EDGE('',*,*,#12792,.T.);
#16810=ORIENTED_EDGE('',*,*,#12793,.F.);
#16811=ORIENTED_EDGE('',*,*,#12794,.T.);
#16812=ORIENTED_EDGE('',*,*,#12790,.T.);
#16813=ORIENTED_EDGE('',*,*,#12795,.T.);
#16814=ORIENTED_EDGE('',*,*,#12796,.F.);
#16815=ORIENTED_EDGE('',*,*,#12797,.T.);
#16816=ORIENTED_EDGE('',*,*,#12793,.T.);
#16817=ORIENTED_EDGE('',*,*,#12798,.T.);
#16818=ORIENTED_EDGE('',*,*,#12799,.F.);
#16819=ORIENTED_EDGE('',*,*,#12800,.T.);
#16820=ORIENTED_EDGE('',*,*,#12796,.T.);
#16821=ORIENTED_EDGE('',*,*,#12801,.T.);
#16822=ORIENTED_EDGE('',*,*,#12802,.F.);
#16823=ORIENTED_EDGE('',*,*,#12803,.T.);
#16824=ORIENTED_EDGE('',*,*,#12799,.T.);
#16825=ORIENTED_EDGE('',*,*,#12804,.T.);
#16826=ORIENTED_EDGE('',*,*,#12805,.F.);
#16827=ORIENTED_EDGE('',*,*,#12806,.T.);
#16828=ORIENTED_EDGE('',*,*,#12802,.T.);
#16829=ORIENTED_EDGE('',*,*,#12807,.T.);
#16830=ORIENTED_EDGE('',*,*,#12808,.F.);
#16831=ORIENTED_EDGE('',*,*,#12809,.T.);
#16832=ORIENTED_EDGE('',*,*,#12805,.T.);
#16833=ORIENTED_EDGE('',*,*,#12810,.T.);
#16834=ORIENTED_EDGE('',*,*,#12811,.F.);
#16835=ORIENTED_EDGE('',*,*,#12812,.T.);
#16836=ORIENTED_EDGE('',*,*,#12808,.T.);
#16837=ORIENTED_EDGE('',*,*,#12813,.T.);
#16838=ORIENTED_EDGE('',*,*,#12814,.F.);
#16839=ORIENTED_EDGE('',*,*,#12815,.T.);
#16840=ORIENTED_EDGE('',*,*,#12811,.T.);
#16841=ORIENTED_EDGE('',*,*,#12816,.T.);
#16842=ORIENTED_EDGE('',*,*,#12817,.F.);
#16843=ORIENTED_EDGE('',*,*,#12818,.T.);
#16844=ORIENTED_EDGE('',*,*,#12814,.T.);
#16845=ORIENTED_EDGE('',*,*,#12819,.T.);
#16846=ORIENTED_EDGE('',*,*,#12820,.F.);
#16847=ORIENTED_EDGE('',*,*,#12821,.T.);
#16848=ORIENTED_EDGE('',*,*,#12817,.T.);
#16849=ORIENTED_EDGE('',*,*,#12822,.T.);
#16850=ORIENTED_EDGE('',*,*,#12823,.F.);
#16851=ORIENTED_EDGE('',*,*,#12824,.T.);
#16852=ORIENTED_EDGE('',*,*,#12820,.T.);
#16853=ORIENTED_EDGE('',*,*,#12825,.T.);
#16854=ORIENTED_EDGE('',*,*,#12826,.F.);
#16855=ORIENTED_EDGE('',*,*,#12827,.T.);
#16856=ORIENTED_EDGE('',*,*,#12823,.T.);
#16857=ORIENTED_EDGE('',*,*,#12828,.T.);
#16858=ORIENTED_EDGE('',*,*,#12829,.F.);
#16859=ORIENTED_EDGE('',*,*,#12830,.T.);
#16860=ORIENTED_EDGE('',*,*,#12826,.T.);
#16861=ORIENTED_EDGE('',*,*,#12831,.T.);
#16862=ORIENTED_EDGE('',*,*,#12832,.F.);
#16863=ORIENTED_EDGE('',*,*,#12833,.T.);
#16864=ORIENTED_EDGE('',*,*,#12829,.T.);
#16865=ORIENTED_EDGE('',*,*,#12834,.T.);
#16866=ORIENTED_EDGE('',*,*,#12835,.F.);
#16867=ORIENTED_EDGE('',*,*,#12836,.T.);
#16868=ORIENTED_EDGE('',*,*,#12832,.T.);
#16869=ORIENTED_EDGE('',*,*,#12837,.T.);
#16870=ORIENTED_EDGE('',*,*,#12838,.F.);
#16871=ORIENTED_EDGE('',*,*,#12839,.T.);
#16872=ORIENTED_EDGE('',*,*,#12835,.T.);
#16873=ORIENTED_EDGE('',*,*,#12840,.T.);
#16874=ORIENTED_EDGE('',*,*,#12841,.F.);
#16875=ORIENTED_EDGE('',*,*,#12842,.T.);
#16876=ORIENTED_EDGE('',*,*,#12838,.T.);
#16877=ORIENTED_EDGE('',*,*,#12843,.T.);
#16878=ORIENTED_EDGE('',*,*,#12844,.F.);
#16879=ORIENTED_EDGE('',*,*,#12845,.T.);
#16880=ORIENTED_EDGE('',*,*,#12841,.T.);
#16881=ORIENTED_EDGE('',*,*,#12846,.T.);
#16882=ORIENTED_EDGE('',*,*,#12847,.F.);
#16883=ORIENTED_EDGE('',*,*,#12848,.T.);
#16884=ORIENTED_EDGE('',*,*,#12844,.T.);
#16885=ORIENTED_EDGE('',*,*,#12849,.T.);
#16886=ORIENTED_EDGE('',*,*,#12850,.F.);
#16887=ORIENTED_EDGE('',*,*,#12851,.T.);
#16888=ORIENTED_EDGE('',*,*,#12847,.T.);
#16889=ORIENTED_EDGE('',*,*,#12852,.T.);
#16890=ORIENTED_EDGE('',*,*,#12853,.F.);
#16891=ORIENTED_EDGE('',*,*,#12854,.T.);
#16892=ORIENTED_EDGE('',*,*,#12850,.T.);
#16893=ORIENTED_EDGE('',*,*,#12855,.T.);
#16894=ORIENTED_EDGE('',*,*,#12856,.F.);
#16895=ORIENTED_EDGE('',*,*,#12857,.T.);
#16896=ORIENTED_EDGE('',*,*,#12853,.T.);
#16897=ORIENTED_EDGE('',*,*,#12858,.T.);
#16898=ORIENTED_EDGE('',*,*,#12859,.F.);
#16899=ORIENTED_EDGE('',*,*,#12860,.T.);
#16900=ORIENTED_EDGE('',*,*,#12856,.T.);
#16901=ORIENTED_EDGE('',*,*,#12861,.T.);
#16902=ORIENTED_EDGE('',*,*,#12862,.F.);
#16903=ORIENTED_EDGE('',*,*,#12863,.T.);
#16904=ORIENTED_EDGE('',*,*,#12859,.T.);
#16905=ORIENTED_EDGE('',*,*,#12864,.T.);
#16906=ORIENTED_EDGE('',*,*,#12865,.F.);
#16907=ORIENTED_EDGE('',*,*,#12866,.T.);
#16908=ORIENTED_EDGE('',*,*,#12862,.T.);
#16909=ORIENTED_EDGE('',*,*,#12867,.T.);
#16910=ORIENTED_EDGE('',*,*,#12868,.F.);
#16911=ORIENTED_EDGE('',*,*,#12869,.T.);
#16912=ORIENTED_EDGE('',*,*,#12865,.T.);
#16913=ORIENTED_EDGE('',*,*,#12870,.T.);
#16914=ORIENTED_EDGE('',*,*,#12871,.F.);
#16915=ORIENTED_EDGE('',*,*,#12872,.T.);
#16916=ORIENTED_EDGE('',*,*,#12868,.T.);
#16917=ORIENTED_EDGE('',*,*,#12873,.T.);
#16918=ORIENTED_EDGE('',*,*,#12874,.F.);
#16919=ORIENTED_EDGE('',*,*,#12875,.T.);
#16920=ORIENTED_EDGE('',*,*,#12871,.T.);
#16921=ORIENTED_EDGE('',*,*,#12876,.T.);
#16922=ORIENTED_EDGE('',*,*,#12877,.F.);
#16923=ORIENTED_EDGE('',*,*,#12878,.T.);
#16924=ORIENTED_EDGE('',*,*,#12874,.T.);
#16925=ORIENTED_EDGE('',*,*,#12879,.T.);
#16926=ORIENTED_EDGE('',*,*,#12880,.F.);
#16927=ORIENTED_EDGE('',*,*,#12881,.T.);
#16928=ORIENTED_EDGE('',*,*,#12877,.T.);
#16929=ORIENTED_EDGE('',*,*,#12882,.T.);
#16930=ORIENTED_EDGE('',*,*,#12883,.F.);
#16931=ORIENTED_EDGE('',*,*,#12884,.T.);
#16932=ORIENTED_EDGE('',*,*,#12880,.T.);
#16933=ORIENTED_EDGE('',*,*,#12885,.T.);
#16934=ORIENTED_EDGE('',*,*,#12886,.F.);
#16935=ORIENTED_EDGE('',*,*,#12887,.T.);
#16936=ORIENTED_EDGE('',*,*,#12883,.T.);
#16937=ORIENTED_EDGE('',*,*,#12888,.T.);
#16938=ORIENTED_EDGE('',*,*,#12889,.F.);
#16939=ORIENTED_EDGE('',*,*,#12890,.T.);
#16940=ORIENTED_EDGE('',*,*,#12886,.T.);
#16941=ORIENTED_EDGE('',*,*,#12891,.T.);
#16942=ORIENTED_EDGE('',*,*,#12892,.F.);
#16943=ORIENTED_EDGE('',*,*,#12893,.T.);
#16944=ORIENTED_EDGE('',*,*,#12889,.T.);
#16945=ORIENTED_EDGE('',*,*,#12894,.T.);
#16946=ORIENTED_EDGE('',*,*,#12895,.F.);
#16947=ORIENTED_EDGE('',*,*,#12896,.T.);
#16948=ORIENTED_EDGE('',*,*,#12892,.T.);
#16949=ORIENTED_EDGE('',*,*,#12897,.T.);
#16950=ORIENTED_EDGE('',*,*,#12898,.F.);
#16951=ORIENTED_EDGE('',*,*,#12899,.T.);
#16952=ORIENTED_EDGE('',*,*,#12895,.T.);
#16953=ORIENTED_EDGE('',*,*,#12900,.T.);
#16954=ORIENTED_EDGE('',*,*,#12901,.F.);
#16955=ORIENTED_EDGE('',*,*,#12902,.T.);
#16956=ORIENTED_EDGE('',*,*,#12898,.T.);
#16957=ORIENTED_EDGE('',*,*,#12903,.T.);
#16958=ORIENTED_EDGE('',*,*,#12904,.F.);
#16959=ORIENTED_EDGE('',*,*,#12905,.T.);
#16960=ORIENTED_EDGE('',*,*,#12901,.T.);
#16961=ORIENTED_EDGE('',*,*,#12906,.T.);
#16962=ORIENTED_EDGE('',*,*,#12907,.F.);
#16963=ORIENTED_EDGE('',*,*,#12908,.T.);
#16964=ORIENTED_EDGE('',*,*,#12904,.T.);
#16965=ORIENTED_EDGE('',*,*,#12909,.T.);
#16966=ORIENTED_EDGE('',*,*,#12910,.F.);
#16967=ORIENTED_EDGE('',*,*,#12911,.T.);
#16968=ORIENTED_EDGE('',*,*,#12907,.T.);
#16969=ORIENTED_EDGE('',*,*,#12912,.T.);
#16970=ORIENTED_EDGE('',*,*,#12913,.F.);
#16971=ORIENTED_EDGE('',*,*,#12914,.T.);
#16972=ORIENTED_EDGE('',*,*,#12910,.T.);
#16973=ORIENTED_EDGE('',*,*,#12915,.T.);
#16974=ORIENTED_EDGE('',*,*,#12916,.F.);
#16975=ORIENTED_EDGE('',*,*,#12917,.T.);
#16976=ORIENTED_EDGE('',*,*,#12913,.T.);
#16977=ORIENTED_EDGE('',*,*,#12918,.T.);
#16978=ORIENTED_EDGE('',*,*,#12919,.F.);
#16979=ORIENTED_EDGE('',*,*,#12920,.T.);
#16980=ORIENTED_EDGE('',*,*,#12916,.T.);
#16981=ORIENTED_EDGE('',*,*,#12921,.T.);
#16982=ORIENTED_EDGE('',*,*,#12922,.F.);
#16983=ORIENTED_EDGE('',*,*,#12923,.T.);
#16984=ORIENTED_EDGE('',*,*,#12919,.T.);
#16985=ORIENTED_EDGE('',*,*,#12924,.T.);
#16986=ORIENTED_EDGE('',*,*,#12925,.F.);
#16987=ORIENTED_EDGE('',*,*,#12926,.T.);
#16988=ORIENTED_EDGE('',*,*,#12922,.T.);
#16989=ORIENTED_EDGE('',*,*,#12927,.T.);
#16990=ORIENTED_EDGE('',*,*,#12928,.F.);
#16991=ORIENTED_EDGE('',*,*,#12929,.T.);
#16992=ORIENTED_EDGE('',*,*,#12925,.T.);
#16993=ORIENTED_EDGE('',*,*,#12930,.T.);
#16994=ORIENTED_EDGE('',*,*,#12931,.F.);
#16995=ORIENTED_EDGE('',*,*,#12932,.T.);
#16996=ORIENTED_EDGE('',*,*,#12928,.T.);
#16997=ORIENTED_EDGE('',*,*,#12933,.T.);
#16998=ORIENTED_EDGE('',*,*,#12934,.F.);
#16999=ORIENTED_EDGE('',*,*,#12935,.T.);
#17000=ORIENTED_EDGE('',*,*,#12931,.T.);
#17001=ORIENTED_EDGE('',*,*,#12936,.T.);
#17002=ORIENTED_EDGE('',*,*,#12937,.F.);
#17003=ORIENTED_EDGE('',*,*,#12938,.T.);
#17004=ORIENTED_EDGE('',*,*,#12934,.T.);
#17005=ORIENTED_EDGE('',*,*,#12939,.T.);
#17006=ORIENTED_EDGE('',*,*,#12940,.F.);
#17007=ORIENTED_EDGE('',*,*,#12941,.T.);
#17008=ORIENTED_EDGE('',*,*,#12937,.T.);
#17009=ORIENTED_EDGE('',*,*,#12942,.T.);
#17010=ORIENTED_EDGE('',*,*,#12943,.F.);
#17011=ORIENTED_EDGE('',*,*,#12944,.T.);
#17012=ORIENTED_EDGE('',*,*,#12940,.T.);
#17013=ORIENTED_EDGE('',*,*,#12945,.T.);
#17014=ORIENTED_EDGE('',*,*,#12946,.F.);
#17015=ORIENTED_EDGE('',*,*,#12947,.T.);
#17016=ORIENTED_EDGE('',*,*,#12943,.T.);
#17017=ORIENTED_EDGE('',*,*,#12948,.T.);
#17018=ORIENTED_EDGE('',*,*,#12949,.F.);
#17019=ORIENTED_EDGE('',*,*,#12950,.T.);
#17020=ORIENTED_EDGE('',*,*,#12946,.T.);
#17021=ORIENTED_EDGE('',*,*,#12951,.T.);
#17022=ORIENTED_EDGE('',*,*,#12952,.F.);
#17023=ORIENTED_EDGE('',*,*,#12953,.T.);
#17024=ORIENTED_EDGE('',*,*,#12949,.T.);
#17025=ORIENTED_EDGE('',*,*,#12954,.T.);
#17026=ORIENTED_EDGE('',*,*,#12955,.F.);
#17027=ORIENTED_EDGE('',*,*,#12956,.T.);
#17028=ORIENTED_EDGE('',*,*,#12952,.T.);
#17029=ORIENTED_EDGE('',*,*,#12957,.T.);
#17030=ORIENTED_EDGE('',*,*,#12958,.F.);
#17031=ORIENTED_EDGE('',*,*,#12959,.T.);
#17032=ORIENTED_EDGE('',*,*,#12955,.T.);
#17033=ORIENTED_EDGE('',*,*,#12960,.T.);
#17034=ORIENTED_EDGE('',*,*,#12961,.F.);
#17035=ORIENTED_EDGE('',*,*,#12962,.T.);
#17036=ORIENTED_EDGE('',*,*,#12958,.T.);
#17037=ORIENTED_EDGE('',*,*,#12963,.T.);
#17038=ORIENTED_EDGE('',*,*,#12964,.F.);
#17039=ORIENTED_EDGE('',*,*,#12965,.T.);
#17040=ORIENTED_EDGE('',*,*,#12961,.T.);
#17041=ORIENTED_EDGE('',*,*,#12966,.T.);
#17042=ORIENTED_EDGE('',*,*,#12967,.F.);
#17043=ORIENTED_EDGE('',*,*,#12968,.T.);
#17044=ORIENTED_EDGE('',*,*,#12964,.T.);
#17045=ORIENTED_EDGE('',*,*,#12969,.T.);
#17046=ORIENTED_EDGE('',*,*,#12970,.F.);
#17047=ORIENTED_EDGE('',*,*,#12971,.T.);
#17048=ORIENTED_EDGE('',*,*,#12967,.T.);
#17049=ORIENTED_EDGE('',*,*,#12972,.T.);
#17050=ORIENTED_EDGE('',*,*,#12973,.F.);
#17051=ORIENTED_EDGE('',*,*,#12974,.T.);
#17052=ORIENTED_EDGE('',*,*,#12975,.F.);
#17053=ORIENTED_EDGE('',*,*,#12976,.F.);
#17054=ORIENTED_EDGE('',*,*,#12977,.T.);
#17055=ORIENTED_EDGE('',*,*,#12973,.T.);
#17056=ORIENTED_EDGE('',*,*,#12978,.F.);
#17057=ORIENTED_EDGE('',*,*,#12979,.F.);
#17058=ORIENTED_EDGE('',*,*,#12980,.F.);
#17059=ORIENTED_EDGE('',*,*,#12981,.T.);
#17060=ORIENTED_EDGE('',*,*,#12976,.T.);
#17061=ORIENTED_EDGE('',*,*,#12982,.F.);
#17062=ORIENTED_EDGE('',*,*,#12983,.F.);
#17063=ORIENTED_EDGE('',*,*,#12984,.T.);
#17064=ORIENTED_EDGE('',*,*,#12980,.T.);
#17065=ORIENTED_EDGE('',*,*,#12985,.F.);
#17066=ORIENTED_EDGE('',*,*,#12986,.F.);
#17067=ORIENTED_EDGE('',*,*,#12987,.T.);
#17068=ORIENTED_EDGE('',*,*,#12983,.T.);
#17069=ORIENTED_EDGE('',*,*,#12988,.F.);
#17070=ORIENTED_EDGE('',*,*,#12989,.F.);
#17071=ORIENTED_EDGE('',*,*,#12990,.T.);
#17072=ORIENTED_EDGE('',*,*,#12986,.T.);
#17073=ORIENTED_EDGE('',*,*,#12991,.F.);
#17074=ORIENTED_EDGE('',*,*,#12992,.F.);
#17075=ORIENTED_EDGE('',*,*,#12993,.T.);
#17076=ORIENTED_EDGE('',*,*,#12989,.T.);
#17077=ORIENTED_EDGE('',*,*,#12994,.F.);
#17078=ORIENTED_EDGE('',*,*,#12995,.F.);
#17079=ORIENTED_EDGE('',*,*,#12996,.T.);
#17080=ORIENTED_EDGE('',*,*,#12992,.T.);
#17081=ORIENTED_EDGE('',*,*,#12997,.F.);
#17082=ORIENTED_EDGE('',*,*,#12998,.F.);
#17083=ORIENTED_EDGE('',*,*,#12999,.T.);
#17084=ORIENTED_EDGE('',*,*,#12995,.T.);
#17085=ORIENTED_EDGE('',*,*,#13000,.F.);
#17086=ORIENTED_EDGE('',*,*,#13001,.F.);
#17087=ORIENTED_EDGE('',*,*,#13002,.T.);
#17088=ORIENTED_EDGE('',*,*,#12998,.T.);
#17089=ORIENTED_EDGE('',*,*,#13003,.F.);
#17090=ORIENTED_EDGE('',*,*,#13004,.F.);
#17091=ORIENTED_EDGE('',*,*,#13005,.T.);
#17092=ORIENTED_EDGE('',*,*,#13001,.T.);
#17093=ORIENTED_EDGE('',*,*,#13006,.F.);
#17094=ORIENTED_EDGE('',*,*,#13007,.F.);
#17095=ORIENTED_EDGE('',*,*,#13008,.T.);
#17096=ORIENTED_EDGE('',*,*,#13004,.T.);
#17097=ORIENTED_EDGE('',*,*,#13009,.F.);
#17098=ORIENTED_EDGE('',*,*,#13010,.F.);
#17099=ORIENTED_EDGE('',*,*,#13011,.T.);
#17100=ORIENTED_EDGE('',*,*,#13007,.T.);
#17101=ORIENTED_EDGE('',*,*,#13012,.F.);
#17102=ORIENTED_EDGE('',*,*,#13013,.F.);
#17103=ORIENTED_EDGE('',*,*,#13014,.T.);
#17104=ORIENTED_EDGE('',*,*,#13010,.T.);
#17105=ORIENTED_EDGE('',*,*,#13015,.F.);
#17106=ORIENTED_EDGE('',*,*,#13016,.F.);
#17107=ORIENTED_EDGE('',*,*,#13017,.T.);
#17108=ORIENTED_EDGE('',*,*,#13013,.T.);
#17109=ORIENTED_EDGE('',*,*,#13018,.F.);
#17110=ORIENTED_EDGE('',*,*,#13019,.F.);
#17111=ORIENTED_EDGE('',*,*,#13020,.T.);
#17112=ORIENTED_EDGE('',*,*,#13016,.T.);
#17113=ORIENTED_EDGE('',*,*,#13021,.F.);
#17114=ORIENTED_EDGE('',*,*,#13022,.F.);
#17115=ORIENTED_EDGE('',*,*,#13023,.T.);
#17116=ORIENTED_EDGE('',*,*,#13019,.T.);
#17117=ORIENTED_EDGE('',*,*,#13024,.F.);
#17118=ORIENTED_EDGE('',*,*,#13025,.F.);
#17119=ORIENTED_EDGE('',*,*,#13026,.T.);
#17120=ORIENTED_EDGE('',*,*,#13022,.T.);
#17121=ORIENTED_EDGE('',*,*,#13027,.F.);
#17122=ORIENTED_EDGE('',*,*,#13028,.F.);
#17123=ORIENTED_EDGE('',*,*,#13029,.T.);
#17124=ORIENTED_EDGE('',*,*,#13025,.T.);
#17125=ORIENTED_EDGE('',*,*,#13030,.F.);
#17126=ORIENTED_EDGE('',*,*,#13031,.F.);
#17127=ORIENTED_EDGE('',*,*,#13032,.T.);
#17128=ORIENTED_EDGE('',*,*,#13028,.T.);
#17129=ORIENTED_EDGE('',*,*,#13033,.F.);
#17130=ORIENTED_EDGE('',*,*,#13034,.F.);
#17131=ORIENTED_EDGE('',*,*,#13035,.T.);
#17132=ORIENTED_EDGE('',*,*,#13031,.T.);
#17133=ORIENTED_EDGE('',*,*,#13036,.F.);
#17134=ORIENTED_EDGE('',*,*,#13037,.F.);
#17135=ORIENTED_EDGE('',*,*,#13038,.T.);
#17136=ORIENTED_EDGE('',*,*,#13034,.T.);
#17137=ORIENTED_EDGE('',*,*,#13039,.F.);
#17138=ORIENTED_EDGE('',*,*,#13040,.F.);
#17139=ORIENTED_EDGE('',*,*,#13041,.T.);
#17140=ORIENTED_EDGE('',*,*,#13037,.T.);
#17141=ORIENTED_EDGE('',*,*,#13042,.F.);
#17142=ORIENTED_EDGE('',*,*,#13043,.F.);
#17143=ORIENTED_EDGE('',*,*,#13044,.T.);
#17144=ORIENTED_EDGE('',*,*,#13040,.T.);
#17145=ORIENTED_EDGE('',*,*,#13045,.F.);
#17146=ORIENTED_EDGE('',*,*,#13046,.F.);
#17147=ORIENTED_EDGE('',*,*,#13047,.T.);
#17148=ORIENTED_EDGE('',*,*,#13043,.T.);
#17149=ORIENTED_EDGE('',*,*,#13048,.F.);
#17150=ORIENTED_EDGE('',*,*,#13049,.F.);
#17151=ORIENTED_EDGE('',*,*,#13050,.T.);
#17152=ORIENTED_EDGE('',*,*,#13046,.T.);
#17153=ORIENTED_EDGE('',*,*,#13051,.F.);
#17154=ORIENTED_EDGE('',*,*,#13052,.F.);
#17155=ORIENTED_EDGE('',*,*,#13053,.T.);
#17156=ORIENTED_EDGE('',*,*,#13049,.T.);
#17157=ORIENTED_EDGE('',*,*,#13054,.F.);
#17158=ORIENTED_EDGE('',*,*,#13055,.F.);
#17159=ORIENTED_EDGE('',*,*,#13056,.T.);
#17160=ORIENTED_EDGE('',*,*,#13052,.T.);
#17161=ORIENTED_EDGE('',*,*,#13057,.F.);
#17162=ORIENTED_EDGE('',*,*,#13058,.F.);
#17163=ORIENTED_EDGE('',*,*,#13059,.T.);
#17164=ORIENTED_EDGE('',*,*,#13055,.T.);
#17165=ORIENTED_EDGE('',*,*,#13060,.F.);
#17166=ORIENTED_EDGE('',*,*,#13061,.F.);
#17167=ORIENTED_EDGE('',*,*,#13062,.T.);
#17168=ORIENTED_EDGE('',*,*,#13058,.T.);
#17169=ORIENTED_EDGE('',*,*,#13063,.F.);
#17170=ORIENTED_EDGE('',*,*,#13064,.F.);
#17171=ORIENTED_EDGE('',*,*,#13065,.T.);
#17172=ORIENTED_EDGE('',*,*,#13061,.T.);
#17173=ORIENTED_EDGE('',*,*,#13066,.F.);
#17174=ORIENTED_EDGE('',*,*,#13067,.F.);
#17175=ORIENTED_EDGE('',*,*,#13068,.T.);
#17176=ORIENTED_EDGE('',*,*,#13064,.T.);
#17177=ORIENTED_EDGE('',*,*,#13069,.F.);
#17178=ORIENTED_EDGE('',*,*,#13070,.F.);
#17179=ORIENTED_EDGE('',*,*,#13071,.T.);
#17180=ORIENTED_EDGE('',*,*,#13067,.T.);
#17181=ORIENTED_EDGE('',*,*,#13072,.F.);
#17182=ORIENTED_EDGE('',*,*,#13073,.F.);
#17183=ORIENTED_EDGE('',*,*,#13074,.T.);
#17184=ORIENTED_EDGE('',*,*,#13070,.T.);
#17185=ORIENTED_EDGE('',*,*,#13075,.F.);
#17186=ORIENTED_EDGE('',*,*,#13076,.F.);
#17187=ORIENTED_EDGE('',*,*,#13077,.T.);
#17188=ORIENTED_EDGE('',*,*,#13073,.T.);
#17189=ORIENTED_EDGE('',*,*,#13078,.F.);
#17190=ORIENTED_EDGE('',*,*,#13079,.F.);
#17191=ORIENTED_EDGE('',*,*,#13080,.T.);
#17192=ORIENTED_EDGE('',*,*,#13076,.T.);
#17193=ORIENTED_EDGE('',*,*,#13081,.F.);
#17194=ORIENTED_EDGE('',*,*,#13082,.F.);
#17195=ORIENTED_EDGE('',*,*,#13083,.T.);
#17196=ORIENTED_EDGE('',*,*,#13079,.T.);
#17197=ORIENTED_EDGE('',*,*,#13084,.F.);
#17198=ORIENTED_EDGE('',*,*,#13085,.F.);
#17199=ORIENTED_EDGE('',*,*,#13086,.T.);
#17200=ORIENTED_EDGE('',*,*,#13082,.T.);
#17201=ORIENTED_EDGE('',*,*,#13087,.F.);
#17202=ORIENTED_EDGE('',*,*,#13088,.F.);
#17203=ORIENTED_EDGE('',*,*,#13089,.T.);
#17204=ORIENTED_EDGE('',*,*,#13085,.T.);
#17205=ORIENTED_EDGE('',*,*,#13090,.F.);
#17206=ORIENTED_EDGE('',*,*,#13091,.F.);
#17207=ORIENTED_EDGE('',*,*,#13092,.T.);
#17208=ORIENTED_EDGE('',*,*,#13088,.T.);
#17209=ORIENTED_EDGE('',*,*,#13093,.F.);
#17210=ORIENTED_EDGE('',*,*,#13094,.F.);
#17211=ORIENTED_EDGE('',*,*,#13095,.T.);
#17212=ORIENTED_EDGE('',*,*,#13091,.T.);
#17213=ORIENTED_EDGE('',*,*,#13096,.F.);
#17214=ORIENTED_EDGE('',*,*,#13097,.F.);
#17215=ORIENTED_EDGE('',*,*,#13098,.T.);
#17216=ORIENTED_EDGE('',*,*,#13094,.T.);
#17217=ORIENTED_EDGE('',*,*,#13099,.F.);
#17218=ORIENTED_EDGE('',*,*,#13100,.F.);
#17219=ORIENTED_EDGE('',*,*,#13101,.T.);
#17220=ORIENTED_EDGE('',*,*,#13097,.T.);
#17221=ORIENTED_EDGE('',*,*,#13102,.F.);
#17222=ORIENTED_EDGE('',*,*,#13103,.F.);
#17223=ORIENTED_EDGE('',*,*,#13104,.T.);
#17224=ORIENTED_EDGE('',*,*,#13100,.T.);
#17225=ORIENTED_EDGE('',*,*,#13105,.F.);
#17226=ORIENTED_EDGE('',*,*,#13106,.F.);
#17227=ORIENTED_EDGE('',*,*,#13107,.T.);
#17228=ORIENTED_EDGE('',*,*,#13103,.T.);
#17229=ORIENTED_EDGE('',*,*,#13108,.F.);
#17230=ORIENTED_EDGE('',*,*,#13109,.F.);
#17231=ORIENTED_EDGE('',*,*,#13110,.T.);
#17232=ORIENTED_EDGE('',*,*,#13106,.T.);
#17233=ORIENTED_EDGE('',*,*,#13111,.F.);
#17234=ORIENTED_EDGE('',*,*,#13112,.F.);
#17235=ORIENTED_EDGE('',*,*,#13113,.T.);
#17236=ORIENTED_EDGE('',*,*,#13109,.T.);
#17237=ORIENTED_EDGE('',*,*,#13114,.F.);
#17238=ORIENTED_EDGE('',*,*,#13115,.F.);
#17239=ORIENTED_EDGE('',*,*,#13116,.T.);
#17240=ORIENTED_EDGE('',*,*,#13112,.T.);
#17241=ORIENTED_EDGE('',*,*,#13117,.F.);
#17242=ORIENTED_EDGE('',*,*,#13118,.F.);
#17243=ORIENTED_EDGE('',*,*,#13119,.T.);
#17244=ORIENTED_EDGE('',*,*,#13115,.T.);
#17245=ORIENTED_EDGE('',*,*,#13120,.F.);
#17246=ORIENTED_EDGE('',*,*,#13121,.F.);
#17247=ORIENTED_EDGE('',*,*,#13122,.T.);
#17248=ORIENTED_EDGE('',*,*,#13118,.T.);
#17249=ORIENTED_EDGE('',*,*,#13123,.F.);
#17250=ORIENTED_EDGE('',*,*,#13124,.F.);
#17251=ORIENTED_EDGE('',*,*,#13125,.T.);
#17252=ORIENTED_EDGE('',*,*,#13121,.T.);
#17253=ORIENTED_EDGE('',*,*,#13126,.F.);
#17254=ORIENTED_EDGE('',*,*,#13127,.F.);
#17255=ORIENTED_EDGE('',*,*,#13128,.T.);
#17256=ORIENTED_EDGE('',*,*,#13124,.T.);
#17257=ORIENTED_EDGE('',*,*,#13129,.F.);
#17258=ORIENTED_EDGE('',*,*,#13130,.F.);
#17259=ORIENTED_EDGE('',*,*,#13131,.T.);
#17260=ORIENTED_EDGE('',*,*,#13127,.T.);
#17261=ORIENTED_EDGE('',*,*,#13132,.F.);
#17262=ORIENTED_EDGE('',*,*,#13133,.F.);
#17263=ORIENTED_EDGE('',*,*,#13134,.T.);
#17264=ORIENTED_EDGE('',*,*,#13130,.T.);
#17265=ORIENTED_EDGE('',*,*,#13135,.F.);
#17266=ORIENTED_EDGE('',*,*,#13136,.F.);
#17267=ORIENTED_EDGE('',*,*,#13137,.T.);
#17268=ORIENTED_EDGE('',*,*,#13133,.T.);
#17269=ORIENTED_EDGE('',*,*,#13138,.F.);
#17270=ORIENTED_EDGE('',*,*,#13139,.F.);
#17271=ORIENTED_EDGE('',*,*,#13140,.T.);
#17272=ORIENTED_EDGE('',*,*,#13136,.T.);
#17273=ORIENTED_EDGE('',*,*,#13141,.F.);
#17274=ORIENTED_EDGE('',*,*,#13142,.F.);
#17275=ORIENTED_EDGE('',*,*,#13143,.T.);
#17276=ORIENTED_EDGE('',*,*,#13139,.T.);
#17277=ORIENTED_EDGE('',*,*,#13144,.F.);
#17278=ORIENTED_EDGE('',*,*,#13145,.F.);
#17279=ORIENTED_EDGE('',*,*,#13146,.T.);
#17280=ORIENTED_EDGE('',*,*,#13142,.T.);
#17281=ORIENTED_EDGE('',*,*,#13147,.F.);
#17282=ORIENTED_EDGE('',*,*,#13148,.F.);
#17283=ORIENTED_EDGE('',*,*,#13149,.T.);
#17284=ORIENTED_EDGE('',*,*,#13145,.T.);
#17285=ORIENTED_EDGE('',*,*,#13150,.F.);
#17286=ORIENTED_EDGE('',*,*,#13151,.F.);
#17287=ORIENTED_EDGE('',*,*,#13152,.T.);
#17288=ORIENTED_EDGE('',*,*,#13148,.T.);
#17289=ORIENTED_EDGE('',*,*,#13153,.F.);
#17290=ORIENTED_EDGE('',*,*,#13154,.F.);
#17291=ORIENTED_EDGE('',*,*,#13155,.T.);
#17292=ORIENTED_EDGE('',*,*,#13151,.T.);
#17293=ORIENTED_EDGE('',*,*,#13156,.F.);
#17294=ORIENTED_EDGE('',*,*,#13157,.F.);
#17295=ORIENTED_EDGE('',*,*,#13158,.T.);
#17296=ORIENTED_EDGE('',*,*,#13154,.T.);
#17297=ORIENTED_EDGE('',*,*,#13159,.F.);
#17298=ORIENTED_EDGE('',*,*,#13160,.F.);
#17299=ORIENTED_EDGE('',*,*,#13161,.T.);
#17300=ORIENTED_EDGE('',*,*,#13157,.T.);
#17301=ORIENTED_EDGE('',*,*,#13162,.F.);
#17302=ORIENTED_EDGE('',*,*,#13163,.T.);
#17303=ORIENTED_EDGE('',*,*,#13164,.T.);
#17304=ORIENTED_EDGE('',*,*,#12785,.F.);
#17305=ORIENTED_EDGE('',*,*,#13165,.T.);
#17306=ORIENTED_EDGE('',*,*,#13166,.T.);
#17307=ORIENTED_EDGE('',*,*,#13163,.F.);
#17308=ORIENTED_EDGE('',*,*,#13167,.T.);
#17309=ORIENTED_EDGE('',*,*,#13168,.T.);
#17310=ORIENTED_EDGE('',*,*,#13167,.F.);
#17311=ORIENTED_EDGE('',*,*,#13168,.F.);
#17312=ORIENTED_EDGE('',*,*,#13169,.F.);
#17313=ORIENTED_EDGE('',*,*,#13170,.F.);
#17314=ORIENTED_EDGE('',*,*,#12972,.F.);
#17315=ORIENTED_EDGE('',*,*,#12969,.F.);
#17316=ORIENTED_EDGE('',*,*,#12966,.F.);
#17317=ORIENTED_EDGE('',*,*,#12963,.F.);
#17318=ORIENTED_EDGE('',*,*,#12960,.F.);
#17319=ORIENTED_EDGE('',*,*,#12957,.F.);
#17320=ORIENTED_EDGE('',*,*,#12954,.F.);
#17321=ORIENTED_EDGE('',*,*,#12951,.F.);
#17322=ORIENTED_EDGE('',*,*,#12948,.F.);
#17323=ORIENTED_EDGE('',*,*,#12945,.F.);
#17324=ORIENTED_EDGE('',*,*,#12942,.F.);
#17325=ORIENTED_EDGE('',*,*,#12939,.F.);
#17326=ORIENTED_EDGE('',*,*,#12936,.F.);
#17327=ORIENTED_EDGE('',*,*,#12933,.F.);
#17328=ORIENTED_EDGE('',*,*,#12930,.F.);
#17329=ORIENTED_EDGE('',*,*,#12927,.F.);
#17330=ORIENTED_EDGE('',*,*,#12924,.F.);
#17331=ORIENTED_EDGE('',*,*,#12921,.F.);
#17332=ORIENTED_EDGE('',*,*,#12918,.F.);
#17333=ORIENTED_EDGE('',*,*,#12915,.F.);
#17334=ORIENTED_EDGE('',*,*,#12912,.F.);
#17335=ORIENTED_EDGE('',*,*,#12909,.F.);
#17336=ORIENTED_EDGE('',*,*,#12906,.F.);
#17337=ORIENTED_EDGE('',*,*,#12903,.F.);
#17338=ORIENTED_EDGE('',*,*,#12900,.F.);
#17339=ORIENTED_EDGE('',*,*,#12897,.F.);
#17340=ORIENTED_EDGE('',*,*,#12894,.F.);
#17341=ORIENTED_EDGE('',*,*,#12891,.F.);
#17342=ORIENTED_EDGE('',*,*,#12888,.F.);
#17343=ORIENTED_EDGE('',*,*,#12885,.F.);
#17344=ORIENTED_EDGE('',*,*,#12882,.F.);
#17345=ORIENTED_EDGE('',*,*,#12879,.F.);
#17346=ORIENTED_EDGE('',*,*,#12876,.F.);
#17347=ORIENTED_EDGE('',*,*,#12873,.F.);
#17348=ORIENTED_EDGE('',*,*,#12870,.F.);
#17349=ORIENTED_EDGE('',*,*,#12867,.F.);
#17350=ORIENTED_EDGE('',*,*,#12864,.F.);
#17351=ORIENTED_EDGE('',*,*,#12861,.F.);
#17352=ORIENTED_EDGE('',*,*,#12858,.F.);
#17353=ORIENTED_EDGE('',*,*,#12855,.F.);
#17354=ORIENTED_EDGE('',*,*,#12852,.F.);
#17355=ORIENTED_EDGE('',*,*,#12849,.F.);
#17356=ORIENTED_EDGE('',*,*,#12846,.F.);
#17357=ORIENTED_EDGE('',*,*,#12843,.F.);
#17358=ORIENTED_EDGE('',*,*,#12840,.F.);
#17359=ORIENTED_EDGE('',*,*,#12837,.F.);
#17360=ORIENTED_EDGE('',*,*,#12834,.F.);
#17361=ORIENTED_EDGE('',*,*,#12831,.F.);
#17362=ORIENTED_EDGE('',*,*,#12828,.F.);
#17363=ORIENTED_EDGE('',*,*,#12825,.F.);
#17364=ORIENTED_EDGE('',*,*,#12822,.F.);
#17365=ORIENTED_EDGE('',*,*,#12819,.F.);
#17366=ORIENTED_EDGE('',*,*,#12816,.F.);
#17367=ORIENTED_EDGE('',*,*,#12813,.F.);
#17368=ORIENTED_EDGE('',*,*,#12810,.F.);
#17369=ORIENTED_EDGE('',*,*,#12807,.F.);
#17370=ORIENTED_EDGE('',*,*,#12804,.F.);
#17371=ORIENTED_EDGE('',*,*,#12801,.F.);
#17372=ORIENTED_EDGE('',*,*,#12798,.F.);
#17373=ORIENTED_EDGE('',*,*,#12795,.F.);
#17374=ORIENTED_EDGE('',*,*,#12792,.F.);
#17375=ORIENTED_EDGE('',*,*,#12789,.F.);
#17376=ORIENTED_EDGE('',*,*,#12786,.F.);
#17377=ORIENTED_EDGE('',*,*,#13164,.F.);
#17378=ORIENTED_EDGE('',*,*,#13171,.T.);
#17379=ORIENTED_EDGE('',*,*,#13162,.T.);
#17380=ORIENTED_EDGE('',*,*,#13159,.T.);
#17381=ORIENTED_EDGE('',*,*,#13156,.T.);
#17382=ORIENTED_EDGE('',*,*,#13153,.T.);
#17383=ORIENTED_EDGE('',*,*,#13150,.T.);
#17384=ORIENTED_EDGE('',*,*,#13147,.T.);
#17385=ORIENTED_EDGE('',*,*,#13144,.T.);
#17386=ORIENTED_EDGE('',*,*,#13141,.T.);
#17387=ORIENTED_EDGE('',*,*,#13138,.T.);
#17388=ORIENTED_EDGE('',*,*,#13135,.T.);
#17389=ORIENTED_EDGE('',*,*,#13132,.T.);
#17390=ORIENTED_EDGE('',*,*,#13129,.T.);
#17391=ORIENTED_EDGE('',*,*,#13126,.T.);
#17392=ORIENTED_EDGE('',*,*,#13123,.T.);
#17393=ORIENTED_EDGE('',*,*,#13120,.T.);
#17394=ORIENTED_EDGE('',*,*,#13117,.T.);
#17395=ORIENTED_EDGE('',*,*,#13114,.T.);
#17396=ORIENTED_EDGE('',*,*,#13111,.T.);
#17397=ORIENTED_EDGE('',*,*,#13108,.T.);
#17398=ORIENTED_EDGE('',*,*,#13105,.T.);
#17399=ORIENTED_EDGE('',*,*,#13102,.T.);
#17400=ORIENTED_EDGE('',*,*,#13099,.T.);
#17401=ORIENTED_EDGE('',*,*,#13096,.T.);
#17402=ORIENTED_EDGE('',*,*,#13093,.T.);
#17403=ORIENTED_EDGE('',*,*,#13090,.T.);
#17404=ORIENTED_EDGE('',*,*,#13087,.T.);
#17405=ORIENTED_EDGE('',*,*,#13084,.T.);
#17406=ORIENTED_EDGE('',*,*,#13081,.T.);
#17407=ORIENTED_EDGE('',*,*,#13078,.T.);
#17408=ORIENTED_EDGE('',*,*,#13075,.T.);
#17409=ORIENTED_EDGE('',*,*,#13072,.T.);
#17410=ORIENTED_EDGE('',*,*,#13069,.T.);
#17411=ORIENTED_EDGE('',*,*,#13066,.T.);
#17412=ORIENTED_EDGE('',*,*,#13063,.T.);
#17413=ORIENTED_EDGE('',*,*,#13060,.T.);
#17414=ORIENTED_EDGE('',*,*,#13057,.T.);
#17415=ORIENTED_EDGE('',*,*,#13054,.T.);
#17416=ORIENTED_EDGE('',*,*,#13051,.T.);
#17417=ORIENTED_EDGE('',*,*,#13048,.T.);
#17418=ORIENTED_EDGE('',*,*,#13045,.T.);
#17419=ORIENTED_EDGE('',*,*,#13042,.T.);
#17420=ORIENTED_EDGE('',*,*,#13039,.T.);
#17421=ORIENTED_EDGE('',*,*,#13036,.T.);
#17422=ORIENTED_EDGE('',*,*,#13033,.T.);
#17423=ORIENTED_EDGE('',*,*,#13030,.T.);
#17424=ORIENTED_EDGE('',*,*,#13027,.T.);
#17425=ORIENTED_EDGE('',*,*,#13024,.T.);
#17426=ORIENTED_EDGE('',*,*,#13021,.T.);
#17427=ORIENTED_EDGE('',*,*,#13018,.T.);
#17428=ORIENTED_EDGE('',*,*,#13015,.T.);
#17429=ORIENTED_EDGE('',*,*,#13012,.T.);
#17430=ORIENTED_EDGE('',*,*,#13009,.T.);
#17431=ORIENTED_EDGE('',*,*,#13006,.T.);
#17432=ORIENTED_EDGE('',*,*,#13003,.T.);
#17433=ORIENTED_EDGE('',*,*,#13000,.T.);
#17434=ORIENTED_EDGE('',*,*,#12997,.T.);
#17435=ORIENTED_EDGE('',*,*,#12994,.T.);
#17436=ORIENTED_EDGE('',*,*,#12991,.T.);
#17437=ORIENTED_EDGE('',*,*,#12988,.T.);
#17438=ORIENTED_EDGE('',*,*,#12985,.T.);
#17439=ORIENTED_EDGE('',*,*,#12982,.T.);
#17440=ORIENTED_EDGE('',*,*,#12979,.T.);
#17441=ORIENTED_EDGE('',*,*,#13160,.T.);
#17442=ORIENTED_EDGE('',*,*,#13171,.F.);
#17443=ORIENTED_EDGE('',*,*,#13166,.F.);
#17444=ORIENTED_EDGE('',*,*,#13172,.T.);
#17445=ORIENTED_EDGE('',*,*,#13173,.F.);
#17446=ORIENTED_EDGE('',*,*,#12974,.F.);
#17447=ORIENTED_EDGE('',*,*,#12977,.F.);
#17448=ORIENTED_EDGE('',*,*,#12981,.F.);
#17449=ORIENTED_EDGE('',*,*,#12984,.F.);
#17450=ORIENTED_EDGE('',*,*,#12987,.F.);
#17451=ORIENTED_EDGE('',*,*,#12990,.F.);
#17452=ORIENTED_EDGE('',*,*,#12993,.F.);
#17453=ORIENTED_EDGE('',*,*,#12996,.F.);
#17454=ORIENTED_EDGE('',*,*,#12999,.F.);
#17455=ORIENTED_EDGE('',*,*,#13002,.F.);
#17456=ORIENTED_EDGE('',*,*,#13005,.F.);
#17457=ORIENTED_EDGE('',*,*,#13008,.F.);
#17458=ORIENTED_EDGE('',*,*,#13011,.F.);
#17459=ORIENTED_EDGE('',*,*,#13014,.F.);
#17460=ORIENTED_EDGE('',*,*,#13017,.F.);
#17461=ORIENTED_EDGE('',*,*,#13020,.F.);
#17462=ORIENTED_EDGE('',*,*,#13023,.F.);
#17463=ORIENTED_EDGE('',*,*,#13026,.F.);
#17464=ORIENTED_EDGE('',*,*,#13029,.F.);
#17465=ORIENTED_EDGE('',*,*,#13032,.F.);
#17466=ORIENTED_EDGE('',*,*,#13035,.F.);
#17467=ORIENTED_EDGE('',*,*,#13038,.F.);
#17468=ORIENTED_EDGE('',*,*,#13041,.F.);
#17469=ORIENTED_EDGE('',*,*,#13044,.F.);
#17470=ORIENTED_EDGE('',*,*,#13047,.F.);
#17471=ORIENTED_EDGE('',*,*,#13050,.F.);
#17472=ORIENTED_EDGE('',*,*,#13053,.F.);
#17473=ORIENTED_EDGE('',*,*,#13056,.F.);
#17474=ORIENTED_EDGE('',*,*,#13059,.F.);
#17475=ORIENTED_EDGE('',*,*,#13062,.F.);
#17476=ORIENTED_EDGE('',*,*,#13065,.F.);
#17477=ORIENTED_EDGE('',*,*,#13068,.F.);
#17478=ORIENTED_EDGE('',*,*,#13071,.F.);
#17479=ORIENTED_EDGE('',*,*,#13074,.F.);
#17480=ORIENTED_EDGE('',*,*,#13077,.F.);
#17481=ORIENTED_EDGE('',*,*,#13080,.F.);
#17482=ORIENTED_EDGE('',*,*,#13083,.F.);
#17483=ORIENTED_EDGE('',*,*,#13086,.F.);
#17484=ORIENTED_EDGE('',*,*,#13089,.F.);
#17485=ORIENTED_EDGE('',*,*,#13092,.F.);
#17486=ORIENTED_EDGE('',*,*,#13095,.F.);
#17487=ORIENTED_EDGE('',*,*,#13098,.F.);
#17488=ORIENTED_EDGE('',*,*,#13101,.F.);
#17489=ORIENTED_EDGE('',*,*,#13104,.F.);
#17490=ORIENTED_EDGE('',*,*,#13107,.F.);
#17491=ORIENTED_EDGE('',*,*,#13110,.F.);
#17492=ORIENTED_EDGE('',*,*,#13113,.F.);
#17493=ORIENTED_EDGE('',*,*,#13116,.F.);
#17494=ORIENTED_EDGE('',*,*,#13119,.F.);
#17495=ORIENTED_EDGE('',*,*,#13122,.F.);
#17496=ORIENTED_EDGE('',*,*,#13125,.F.);
#17497=ORIENTED_EDGE('',*,*,#13128,.F.);
#17498=ORIENTED_EDGE('',*,*,#13131,.F.);
#17499=ORIENTED_EDGE('',*,*,#13134,.F.);
#17500=ORIENTED_EDGE('',*,*,#13137,.F.);
#17501=ORIENTED_EDGE('',*,*,#13140,.F.);
#17502=ORIENTED_EDGE('',*,*,#13143,.F.);
#17503=ORIENTED_EDGE('',*,*,#13146,.F.);
#17504=ORIENTED_EDGE('',*,*,#13149,.F.);
#17505=ORIENTED_EDGE('',*,*,#13152,.F.);
#17506=ORIENTED_EDGE('',*,*,#13155,.F.);
#17507=ORIENTED_EDGE('',*,*,#13158,.F.);
#17508=ORIENTED_EDGE('',*,*,#13161,.F.);
#17509=ORIENTED_EDGE('',*,*,#13172,.F.);
#17510=ORIENTED_EDGE('',*,*,#13165,.F.);
#17511=ORIENTED_EDGE('',*,*,#12784,.F.);
#17512=ORIENTED_EDGE('',*,*,#12788,.F.);
#17513=ORIENTED_EDGE('',*,*,#12791,.F.);
#17514=ORIENTED_EDGE('',*,*,#12794,.F.);
#17515=ORIENTED_EDGE('',*,*,#12797,.F.);
#17516=ORIENTED_EDGE('',*,*,#12800,.F.);
#17517=ORIENTED_EDGE('',*,*,#12803,.F.);
#17518=ORIENTED_EDGE('',*,*,#12806,.F.);
#17519=ORIENTED_EDGE('',*,*,#12809,.F.);
#17520=ORIENTED_EDGE('',*,*,#12812,.F.);
#17521=ORIENTED_EDGE('',*,*,#12815,.F.);
#17522=ORIENTED_EDGE('',*,*,#12818,.F.);
#17523=ORIENTED_EDGE('',*,*,#12821,.F.);
#17524=ORIENTED_EDGE('',*,*,#12824,.F.);
#17525=ORIENTED_EDGE('',*,*,#12827,.F.);
#17526=ORIENTED_EDGE('',*,*,#12830,.F.);
#17527=ORIENTED_EDGE('',*,*,#12833,.F.);
#17528=ORIENTED_EDGE('',*,*,#12836,.F.);
#17529=ORIENTED_EDGE('',*,*,#12839,.F.);
#17530=ORIENTED_EDGE('',*,*,#12842,.F.);
#17531=ORIENTED_EDGE('',*,*,#12845,.F.);
#17532=ORIENTED_EDGE('',*,*,#12848,.F.);
#17533=ORIENTED_EDGE('',*,*,#12851,.F.);
#17534=ORIENTED_EDGE('',*,*,#12854,.F.);
#17535=ORIENTED_EDGE('',*,*,#12857,.F.);
#17536=ORIENTED_EDGE('',*,*,#12860,.F.);
#17537=ORIENTED_EDGE('',*,*,#12863,.F.);
#17538=ORIENTED_EDGE('',*,*,#12866,.F.);
#17539=ORIENTED_EDGE('',*,*,#12869,.F.);
#17540=ORIENTED_EDGE('',*,*,#12872,.F.);
#17541=ORIENTED_EDGE('',*,*,#12875,.F.);
#17542=ORIENTED_EDGE('',*,*,#12878,.F.);
#17543=ORIENTED_EDGE('',*,*,#12881,.F.);
#17544=ORIENTED_EDGE('',*,*,#12884,.F.);
#17545=ORIENTED_EDGE('',*,*,#12887,.F.);
#17546=ORIENTED_EDGE('',*,*,#12890,.F.);
#17547=ORIENTED_EDGE('',*,*,#12893,.F.);
#17548=ORIENTED_EDGE('',*,*,#12896,.F.);
#17549=ORIENTED_EDGE('',*,*,#12899,.F.);
#17550=ORIENTED_EDGE('',*,*,#12902,.F.);
#17551=ORIENTED_EDGE('',*,*,#12905,.F.);
#17552=ORIENTED_EDGE('',*,*,#12908,.F.);
#17553=ORIENTED_EDGE('',*,*,#12911,.F.);
#17554=ORIENTED_EDGE('',*,*,#12914,.F.);
#17555=ORIENTED_EDGE('',*,*,#12917,.F.);
#17556=ORIENTED_EDGE('',*,*,#12920,.F.);
#17557=ORIENTED_EDGE('',*,*,#12923,.F.);
#17558=ORIENTED_EDGE('',*,*,#12926,.F.);
#17559=ORIENTED_EDGE('',*,*,#12929,.F.);
#17560=ORIENTED_EDGE('',*,*,#12932,.F.);
#17561=ORIENTED_EDGE('',*,*,#12935,.F.);
#17562=ORIENTED_EDGE('',*,*,#12938,.F.);
#17563=ORIENTED_EDGE('',*,*,#12941,.F.);
#17564=ORIENTED_EDGE('',*,*,#12944,.F.);
#17565=ORIENTED_EDGE('',*,*,#12947,.F.);
#17566=ORIENTED_EDGE('',*,*,#12950,.F.);
#17567=ORIENTED_EDGE('',*,*,#12953,.F.);
#17568=ORIENTED_EDGE('',*,*,#12956,.F.);
#17569=ORIENTED_EDGE('',*,*,#12959,.F.);
#17570=ORIENTED_EDGE('',*,*,#12962,.F.);
#17571=ORIENTED_EDGE('',*,*,#12965,.F.);
#17572=ORIENTED_EDGE('',*,*,#12968,.F.);
#17573=ORIENTED_EDGE('',*,*,#12971,.F.);
#17574=ORIENTED_EDGE('',*,*,#13174,.F.);
#17575=ORIENTED_EDGE('',*,*,#13175,.F.);
#17576=ORIENTED_EDGE('',*,*,#13176,.T.);
#17577=ORIENTED_EDGE('',*,*,#13177,.F.);
#17578=ORIENTED_EDGE('',*,*,#13178,.F.);
#17579=ORIENTED_EDGE('',*,*,#13179,.F.);
#17580=ORIENTED_EDGE('',*,*,#13178,.T.);
#17581=ORIENTED_EDGE('',*,*,#13180,.T.);
#17582=ORIENTED_EDGE('',*,*,#13181,.T.);
#17583=ORIENTED_EDGE('',*,*,#13180,.F.);
#17584=ORIENTED_EDGE('',*,*,#13177,.T.);
#17585=ORIENTED_EDGE('',*,*,#13182,.T.);
#17586=ORIENTED_EDGE('',*,*,#13183,.F.);
#17587=ORIENTED_EDGE('',*,*,#13184,.F.);
#17588=ORIENTED_EDGE('',*,*,#13181,.F.);
#17589=ORIENTED_EDGE('',*,*,#13183,.T.);
#17590=ORIENTED_EDGE('',*,*,#13185,.T.);
#17591=ORIENTED_EDGE('',*,*,#13186,.F.);
#17592=ORIENTED_EDGE('',*,*,#13185,.F.);
#17593=ORIENTED_EDGE('',*,*,#13182,.F.);
#17594=ORIENTED_EDGE('',*,*,#13176,.F.);
#17595=ORIENTED_EDGE('',*,*,#13187,.F.);
#17596=ORIENTED_EDGE('',*,*,#13188,.T.);
#17597=ORIENTED_EDGE('',*,*,#13189,.F.);
#17598=ORIENTED_EDGE('',*,*,#13188,.F.);
#17599=ORIENTED_EDGE('',*,*,#13184,.T.);
#17600=ORIENTED_EDGE('',*,*,#13186,.T.);
#17601=ORIENTED_EDGE('',*,*,#13175,.T.);
#17602=ORIENTED_EDGE('',*,*,#13179,.T.);
#17603=ORIENTED_EDGE('',*,*,#13187,.T.);
#17604=ORIENTED_EDGE('',*,*,#13190,.F.);
#17605=ORIENTED_EDGE('',*,*,#13191,.T.);
#17606=ORIENTED_EDGE('',*,*,#13169,.T.);
#17607=ORIENTED_EDGE('',*,*,#12978,.T.);
#17608=ORIENTED_EDGE('',*,*,#12975,.T.);
#17609=ORIENTED_EDGE('',*,*,#13173,.T.);
#17610=ORIENTED_EDGE('',*,*,#13192,.F.);
#17611=ORIENTED_EDGE('',*,*,#13193,.T.);
#17612=ORIENTED_EDGE('',*,*,#13190,.T.);
#17613=ORIENTED_EDGE('',*,*,#13193,.F.);
#17614=ORIENTED_EDGE('',*,*,#13192,.T.);
#17615=ORIENTED_EDGE('',*,*,#13189,.T.);
#17616=ORIENTED_EDGE('',*,*,#12970,.T.);
#17617=ORIENTED_EDGE('',*,*,#13170,.T.);
#17618=ORIENTED_EDGE('',*,*,#13191,.F.);
#17619=ORIENTED_EDGE('',*,*,#13174,.T.);
#17620=ORIENTED_EDGE('',*,*,#13194,.F.);
#17621=ORIENTED_EDGE('',*,*,#13195,.T.);
#17622=ORIENTED_EDGE('',*,*,#13196,.T.);
#17623=ORIENTED_EDGE('',*,*,#13195,.F.);
#17624=ORIENTED_EDGE('',*,*,#13197,.F.);
#17625=ORIENTED_EDGE('',*,*,#13198,.T.);
#17626=ORIENTED_EDGE('',*,*,#13199,.T.);
#17627=ORIENTED_EDGE('',*,*,#13198,.F.);
#17628=ORIENTED_EDGE('',*,*,#13197,.T.);
#17629=ORIENTED_EDGE('',*,*,#13194,.T.);
#17630=ORIENTED_EDGE('',*,*,#13199,.F.);
#17631=ORIENTED_EDGE('',*,*,#13196,.F.);
#17632=ORIENTED_EDGE('',*,*,#13200,.F.);
#17633=ORIENTED_EDGE('',*,*,#13201,.T.);
#17634=ORIENTED_EDGE('',*,*,#13202,.F.);
#17635=ORIENTED_EDGE('',*,*,#13203,.F.);
#17636=ORIENTED_EDGE('',*,*,#13204,.F.);
#17637=ORIENTED_EDGE('',*,*,#13201,.F.);
#17638=ORIENTED_EDGE('',*,*,#13205,.F.);
#17639=ORIENTED_EDGE('',*,*,#13206,.T.);
#17640=ORIENTED_EDGE('',*,*,#13207,.F.);
#17641=ORIENTED_EDGE('',*,*,#13208,.F.);
#17642=ORIENTED_EDGE('',*,*,#13206,.F.);
#17643=ORIENTED_EDGE('',*,*,#13209,.F.);
#17644=ORIENTED_EDGE('',*,*,#13203,.T.);
#17645=ORIENTED_EDGE('',*,*,#13210,.F.);
#17646=ORIENTED_EDGE('',*,*,#13211,.T.);
#17647=ORIENTED_EDGE('',*,*,#13212,.T.);
#17648=ORIENTED_EDGE('',*,*,#13211,.F.);
#17649=ORIENTED_EDGE('',*,*,#13204,.T.);
#17650=ORIENTED_EDGE('',*,*,#13209,.T.);
#17651=ORIENTED_EDGE('',*,*,#13202,.T.);
#17652=ORIENTED_EDGE('',*,*,#13205,.T.);
#17653=ORIENTED_EDGE('',*,*,#13200,.T.);
#17654=ORIENTED_EDGE('',*,*,#13213,.F.);
#17655=ORIENTED_EDGE('',*,*,#13214,.T.);
#17656=ORIENTED_EDGE('',*,*,#13215,.T.);
#17657=ORIENTED_EDGE('',*,*,#13214,.F.);
#17658=ORIENTED_EDGE('',*,*,#13207,.T.);
#17659=ORIENTED_EDGE('',*,*,#13208,.T.);
#17660=ORIENTED_EDGE('',*,*,#13213,.T.);
#17661=ORIENTED_EDGE('',*,*,#13210,.T.);
#17662=ORIENTED_EDGE('',*,*,#13215,.F.);
#17663=ORIENTED_EDGE('',*,*,#13212,.F.);
#17664=ORIENTED_EDGE('',*,*,#13216,.F.);
#17665=ORIENTED_EDGE('',*,*,#13217,.T.);
#17666=ORIENTED_EDGE('',*,*,#13218,.F.);
#17667=ORIENTED_EDGE('',*,*,#13217,.F.);
#17668=ORIENTED_EDGE('',*,*,#13219,.F.);
#17669=ORIENTED_EDGE('',*,*,#13220,.T.);
#17670=ORIENTED_EDGE('',*,*,#13221,.F.);
#17671=ORIENTED_EDGE('',*,*,#13222,.F.);
#17672=ORIENTED_EDGE('',*,*,#13223,.F.);
#17673=ORIENTED_EDGE('',*,*,#13220,.F.);
#17674=ORIENTED_EDGE('',*,*,#13224,.F.);
#17675=ORIENTED_EDGE('',*,*,#13225,.T.);
#17676=ORIENTED_EDGE('',*,*,#13226,.F.);
#17677=ORIENTED_EDGE('',*,*,#13227,.F.);
#17678=ORIENTED_EDGE('',*,*,#13225,.F.);
#17679=ORIENTED_EDGE('',*,*,#13228,.F.);
#17680=ORIENTED_EDGE('',*,*,#13222,.T.);
#17681=ORIENTED_EDGE('',*,*,#13229,.F.);
#17682=ORIENTED_EDGE('',*,*,#13230,.F.);
#17683=ORIENTED_EDGE('',*,*,#13231,.F.);
#17684=ORIENTED_EDGE('',*,*,#13232,.F.);
#17685=ORIENTED_EDGE('',*,*,#13233,.F.);
#17686=ORIENTED_EDGE('',*,*,#13234,.F.);
#17687=ORIENTED_EDGE('',*,*,#13235,.F.);
#17688=ORIENTED_EDGE('',*,*,#13236,.F.);
#17689=ORIENTED_EDGE('',*,*,#13237,.F.);
#17690=ORIENTED_EDGE('',*,*,#13230,.T.);
#17691=ORIENTED_EDGE('',*,*,#13238,.F.);
#17692=ORIENTED_EDGE('',*,*,#13239,.F.);
#17693=ORIENTED_EDGE('',*,*,#13240,.F.);
#17694=ORIENTED_EDGE('',*,*,#13241,.F.);
#17695=ORIENTED_EDGE('',*,*,#13242,.F.);
#17696=ORIENTED_EDGE('',*,*,#13236,.T.);
#17697=ORIENTED_EDGE('',*,*,#13243,.T.);
#17698=ORIENTED_EDGE('',*,*,#13218,.T.);
#17699=ORIENTED_EDGE('',*,*,#13238,.T.);
#17700=ORIENTED_EDGE('',*,*,#13235,.T.);
#17701=ORIENTED_EDGE('',*,*,#13229,.T.);
#17702=ORIENTED_EDGE('',*,*,#13244,.T.);
#17703=ORIENTED_EDGE('',*,*,#13245,.F.);
#17704=ORIENTED_EDGE('',*,*,#13216,.T.);
#17705=ORIENTED_EDGE('',*,*,#13242,.T.);
#17706=ORIENTED_EDGE('',*,*,#13246,.T.);
#17707=ORIENTED_EDGE('',*,*,#13231,.T.);
#17708=ORIENTED_EDGE('',*,*,#13237,.T.);
#17709=ORIENTED_EDGE('',*,*,#13243,.F.);
#17710=ORIENTED_EDGE('',*,*,#13247,.T.);
#17711=ORIENTED_EDGE('',*,*,#13245,.T.);
#17712=ORIENTED_EDGE('',*,*,#13247,.F.);
#17713=ORIENTED_EDGE('',*,*,#13239,.T.);
#17714=ORIENTED_EDGE('',*,*,#13244,.F.);
#17715=ORIENTED_EDGE('',*,*,#13234,.T.);
#17716=ORIENTED_EDGE('',*,*,#13248,.T.);
#17717=ORIENTED_EDGE('',*,*,#13223,.T.);
#17718=ORIENTED_EDGE('',*,*,#13228,.T.);
#17719=ORIENTED_EDGE('',*,*,#13221,.T.);
#17720=ORIENTED_EDGE('',*,*,#13224,.T.);
#17721=ORIENTED_EDGE('',*,*,#13219,.T.);
#17722=ORIENTED_EDGE('',*,*,#13241,.T.);
#17723=ORIENTED_EDGE('',*,*,#13249,.T.);
#17724=ORIENTED_EDGE('',*,*,#13232,.T.);
#17725=ORIENTED_EDGE('',*,*,#13246,.F.);
#17726=ORIENTED_EDGE('',*,*,#13226,.T.);
#17727=ORIENTED_EDGE('',*,*,#13227,.T.);
#17728=ORIENTED_EDGE('',*,*,#13240,.T.);
#17729=ORIENTED_EDGE('',*,*,#13248,.F.);
#17730=ORIENTED_EDGE('',*,*,#13233,.T.);
#17731=ORIENTED_EDGE('',*,*,#13249,.F.);
#17732=ORIENTED_EDGE('',*,*,#13250,.F.);
#17733=ORIENTED_EDGE('',*,*,#13251,.T.);
#17734=ORIENTED_EDGE('',*,*,#13252,.T.);
#17735=ORIENTED_EDGE('',*,*,#13251,.F.);
#17736=ORIENTED_EDGE('',*,*,#13253,.F.);
#17737=ORIENTED_EDGE('',*,*,#13254,.T.);
#17738=ORIENTED_EDGE('',*,*,#13255,.T.);
#17739=ORIENTED_EDGE('',*,*,#13254,.F.);
#17740=ORIENTED_EDGE('',*,*,#13253,.T.);
#17741=ORIENTED_EDGE('',*,*,#13250,.T.);
#17742=ORIENTED_EDGE('',*,*,#13255,.F.);
#17743=ORIENTED_EDGE('',*,*,#13252,.F.);
#17744=ORIENTED_EDGE('',*,*,#13256,.F.);
#17745=ORIENTED_EDGE('',*,*,#13257,.T.);
#17746=ORIENTED_EDGE('',*,*,#13258,.T.);
#17747=ORIENTED_EDGE('',*,*,#13257,.F.);
#17748=ORIENTED_EDGE('',*,*,#13259,.F.);
#17749=ORIENTED_EDGE('',*,*,#13260,.T.);
#17750=ORIENTED_EDGE('',*,*,#13261,.T.);
#17751=ORIENTED_EDGE('',*,*,#13260,.F.);
#17752=ORIENTED_EDGE('',*,*,#13259,.T.);
#17753=ORIENTED_EDGE('',*,*,#13256,.T.);
#17754=ORIENTED_EDGE('',*,*,#13261,.F.);
#17755=ORIENTED_EDGE('',*,*,#13258,.F.);
#17756=ORIENTED_EDGE('',*,*,#13262,.F.);
#17757=ORIENTED_EDGE('',*,*,#13263,.F.);
#17758=ORIENTED_EDGE('',*,*,#13264,.F.);
#17759=ORIENTED_EDGE('',*,*,#13265,.F.);
#17760=ORIENTED_EDGE('',*,*,#13266,.F.);
#17761=ORIENTED_EDGE('',*,*,#13267,.F.);
#17762=ORIENTED_EDGE('',*,*,#13268,.F.);
#17763=ORIENTED_EDGE('',*,*,#13269,.F.);
#17764=ORIENTED_EDGE('',*,*,#13266,.T.);
#17765=ORIENTED_EDGE('',*,*,#13270,.T.);
#17766=ORIENTED_EDGE('',*,*,#13271,.T.);
#17767=ORIENTED_EDGE('',*,*,#13272,.T.);
#17768=ORIENTED_EDGE('',*,*,#13265,.T.);
#17769=ORIENTED_EDGE('',*,*,#13273,.F.);
#17770=ORIENTED_EDGE('',*,*,#13274,.T.);
#17771=ORIENTED_EDGE('',*,*,#13270,.F.);
#17772=ORIENTED_EDGE('',*,*,#13264,.T.);
#17773=ORIENTED_EDGE('',*,*,#13275,.T.);
#17774=ORIENTED_EDGE('',*,*,#13276,.T.);
#17775=ORIENTED_EDGE('',*,*,#13273,.T.);
#17776=ORIENTED_EDGE('',*,*,#13263,.T.);
#17777=ORIENTED_EDGE('',*,*,#13277,.F.);
#17778=ORIENTED_EDGE('',*,*,#13278,.T.);
#17779=ORIENTED_EDGE('',*,*,#13275,.F.);
#17780=ORIENTED_EDGE('',*,*,#13279,.F.);
#17781=ORIENTED_EDGE('',*,*,#13280,.F.);
#17782=ORIENTED_EDGE('',*,*,#13271,.F.);
#17783=ORIENTED_EDGE('',*,*,#13274,.F.);
#17784=ORIENTED_EDGE('',*,*,#13276,.F.);
#17785=ORIENTED_EDGE('',*,*,#13278,.F.);
#17786=ORIENTED_EDGE('',*,*,#13281,.F.);
#17787=ORIENTED_EDGE('',*,*,#13282,.F.);
#17788=ORIENTED_EDGE('',*,*,#13267,.T.);
#17789=ORIENTED_EDGE('',*,*,#13272,.F.);
#17790=ORIENTED_EDGE('',*,*,#13280,.T.);
#17791=ORIENTED_EDGE('',*,*,#13283,.F.);
#17792=ORIENTED_EDGE('',*,*,#13262,.T.);
#17793=ORIENTED_EDGE('',*,*,#13284,.T.);
#17794=ORIENTED_EDGE('',*,*,#13281,.T.);
#17795=ORIENTED_EDGE('',*,*,#13277,.T.);
#17796=ORIENTED_EDGE('',*,*,#13268,.T.);
#17797=ORIENTED_EDGE('',*,*,#13283,.T.);
#17798=ORIENTED_EDGE('',*,*,#13279,.T.);
#17799=ORIENTED_EDGE('',*,*,#13285,.T.);
#17800=ORIENTED_EDGE('',*,*,#13269,.T.);
#17801=ORIENTED_EDGE('',*,*,#13285,.F.);
#17802=ORIENTED_EDGE('',*,*,#13282,.T.);
#17803=ORIENTED_EDGE('',*,*,#13284,.F.);
#17804=ORIENTED_EDGE('',*,*,#13286,.F.);
#17805=ORIENTED_EDGE('',*,*,#13287,.T.);
#17806=ORIENTED_EDGE('',*,*,#13288,.T.);
#17807=ORIENTED_EDGE('',*,*,#13289,.F.);
#17808=ORIENTED_EDGE('',*,*,#13290,.F.);
#17809=ORIENTED_EDGE('',*,*,#13291,.T.);
#17810=ORIENTED_EDGE('',*,*,#13292,.T.);
#17811=ORIENTED_EDGE('',*,*,#13287,.F.);
#17812=ORIENTED_EDGE('',*,*,#13293,.F.);
#17813=ORIENTED_EDGE('',*,*,#13294,.T.);
#17814=ORIENTED_EDGE('',*,*,#13295,.T.);
#17815=ORIENTED_EDGE('',*,*,#13291,.F.);
#17816=ORIENTED_EDGE('',*,*,#13296,.F.);
#17817=ORIENTED_EDGE('',*,*,#13297,.T.);
#17818=ORIENTED_EDGE('',*,*,#13298,.T.);
#17819=ORIENTED_EDGE('',*,*,#13294,.F.);
#17820=ORIENTED_EDGE('',*,*,#13299,.F.);
#17821=ORIENTED_EDGE('',*,*,#13300,.T.);
#17822=ORIENTED_EDGE('',*,*,#13301,.T.);
#17823=ORIENTED_EDGE('',*,*,#13297,.F.);
#17824=ORIENTED_EDGE('',*,*,#13302,.F.);
#17825=ORIENTED_EDGE('',*,*,#13289,.T.);
#17826=ORIENTED_EDGE('',*,*,#13303,.T.);
#17827=ORIENTED_EDGE('',*,*,#13300,.F.);
#17828=ORIENTED_EDGE('',*,*,#13303,.F.);
#17829=ORIENTED_EDGE('',*,*,#13288,.F.);
#17830=ORIENTED_EDGE('',*,*,#13292,.F.);
#17831=ORIENTED_EDGE('',*,*,#13295,.F.);
#17832=ORIENTED_EDGE('',*,*,#13298,.F.);
#17833=ORIENTED_EDGE('',*,*,#13301,.F.);
#17834=ORIENTED_EDGE('',*,*,#13304,.F.);
#17835=ORIENTED_EDGE('',*,*,#13286,.T.);
#17836=ORIENTED_EDGE('',*,*,#13302,.T.);
#17837=ORIENTED_EDGE('',*,*,#13299,.T.);
#17838=ORIENTED_EDGE('',*,*,#13296,.T.);
#17839=ORIENTED_EDGE('',*,*,#13293,.T.);
#17840=ORIENTED_EDGE('',*,*,#13290,.T.);
#17841=ORIENTED_EDGE('',*,*,#13305,.F.);
#17842=ORIENTED_EDGE('',*,*,#13306,.T.);
#17843=ORIENTED_EDGE('',*,*,#13304,.T.);
#17844=ORIENTED_EDGE('',*,*,#13306,.F.);
#17845=ORIENTED_EDGE('',*,*,#13307,.F.);
#17846=ORIENTED_EDGE('',*,*,#13308,.T.);
#17847=ORIENTED_EDGE('',*,*,#13305,.T.);
#17848=ORIENTED_EDGE('',*,*,#13308,.F.);
#17849=ORIENTED_EDGE('',*,*,#13309,.F.);
#17850=ORIENTED_EDGE('',*,*,#13310,.T.);
#17851=ORIENTED_EDGE('',*,*,#13307,.T.);
#17852=ORIENTED_EDGE('',*,*,#13310,.F.);
#17853=ORIENTED_EDGE('',*,*,#13309,.T.);
#17854=ORIENTED_EDGE('',*,*,#13311,.F.);
#17855=ORIENTED_EDGE('',*,*,#13312,.T.);
#17856=ORIENTED_EDGE('',*,*,#13313,.T.);
#17857=ORIENTED_EDGE('',*,*,#13312,.F.);
#17858=ORIENTED_EDGE('',*,*,#13314,.F.);
#17859=ORIENTED_EDGE('',*,*,#13315,.T.);
#17860=ORIENTED_EDGE('',*,*,#13316,.T.);
#17861=ORIENTED_EDGE('',*,*,#13315,.F.);
#17862=ORIENTED_EDGE('',*,*,#13314,.T.);
#17863=ORIENTED_EDGE('',*,*,#13311,.T.);
#17864=ORIENTED_EDGE('',*,*,#13316,.F.);
#17865=ORIENTED_EDGE('',*,*,#13313,.F.);
#17866=ORIENTED_EDGE('',*,*,#13317,.F.);
#17867=ORIENTED_EDGE('',*,*,#13318,.F.);
#17868=ORIENTED_EDGE('',*,*,#13319,.T.);
#17869=ORIENTED_EDGE('',*,*,#13317,.T.);
#17870=ORIENTED_EDGE('',*,*,#13319,.F.);
#17871=ORIENTED_EDGE('',*,*,#13320,.F.);
#17872=ORIENTED_EDGE('',*,*,#13321,.T.);
#17873=ORIENTED_EDGE('',*,*,#13318,.T.);
#17874=ORIENTED_EDGE('',*,*,#13321,.F.);
#17875=ORIENTED_EDGE('',*,*,#13322,.F.);
#17876=ORIENTED_EDGE('',*,*,#13323,.T.);
#17877=ORIENTED_EDGE('',*,*,#13320,.T.);
#17878=ORIENTED_EDGE('',*,*,#13323,.F.);
#17879=ORIENTED_EDGE('',*,*,#13322,.T.);
#17880=ORIENTED_EDGE('',*,*,#13324,.F.);
#17881=ORIENTED_EDGE('',*,*,#13325,.F.);
#17882=ORIENTED_EDGE('',*,*,#13326,.T.);
#17883=ORIENTED_EDGE('',*,*,#13324,.T.);
#17884=ORIENTED_EDGE('',*,*,#13326,.F.);
#17885=ORIENTED_EDGE('',*,*,#13327,.F.);
#17886=ORIENTED_EDGE('',*,*,#13328,.T.);
#17887=ORIENTED_EDGE('',*,*,#13325,.T.);
#17888=ORIENTED_EDGE('',*,*,#13328,.F.);
#17889=ORIENTED_EDGE('',*,*,#13329,.F.);
#17890=ORIENTED_EDGE('',*,*,#13330,.T.);
#17891=ORIENTED_EDGE('',*,*,#13327,.T.);
#17892=ORIENTED_EDGE('',*,*,#13330,.F.);
#17893=ORIENTED_EDGE('',*,*,#13329,.T.);
#17894=ORIENTED_EDGE('',*,*,#13331,.T.);
#17895=ORIENTED_EDGE('',*,*,#13332,.T.);
#17896=ORIENTED_EDGE('',*,*,#13333,.T.);
#17897=ORIENTED_EDGE('',*,*,#13334,.F.);
#17898=ORIENTED_EDGE('',*,*,#13335,.T.);
#17899=ORIENTED_EDGE('',*,*,#13336,.T.);
#17900=ORIENTED_EDGE('',*,*,#13337,.T.);
#17901=ORIENTED_EDGE('',*,*,#13332,.F.);
#17902=ORIENTED_EDGE('',*,*,#13338,.T.);
#17903=ORIENTED_EDGE('',*,*,#13339,.T.);
#17904=ORIENTED_EDGE('',*,*,#13340,.T.);
#17905=ORIENTED_EDGE('',*,*,#13336,.F.);
#17906=ORIENTED_EDGE('',*,*,#13341,.T.);
#17907=ORIENTED_EDGE('',*,*,#13342,.T.);
#17908=ORIENTED_EDGE('',*,*,#13343,.T.);
#17909=ORIENTED_EDGE('',*,*,#13339,.F.);
#17910=ORIENTED_EDGE('',*,*,#13344,.T.);
#17911=ORIENTED_EDGE('',*,*,#13345,.T.);
#17912=ORIENTED_EDGE('',*,*,#13346,.T.);
#17913=ORIENTED_EDGE('',*,*,#13342,.F.);
#17914=ORIENTED_EDGE('',*,*,#13347,.T.);
#17915=ORIENTED_EDGE('',*,*,#13334,.T.);
#17916=ORIENTED_EDGE('',*,*,#13348,.T.);
#17917=ORIENTED_EDGE('',*,*,#13345,.F.);
#17918=ORIENTED_EDGE('',*,*,#13347,.F.);
#17919=ORIENTED_EDGE('',*,*,#13344,.F.);
#17920=ORIENTED_EDGE('',*,*,#13341,.F.);
#17921=ORIENTED_EDGE('',*,*,#13338,.F.);
#17922=ORIENTED_EDGE('',*,*,#13335,.F.);
#17923=ORIENTED_EDGE('',*,*,#13331,.F.);
#17924=ORIENTED_EDGE('',*,*,#13348,.F.);
#17925=ORIENTED_EDGE('',*,*,#13333,.F.);
#17926=ORIENTED_EDGE('',*,*,#13337,.F.);
#17927=ORIENTED_EDGE('',*,*,#13340,.F.);
#17928=ORIENTED_EDGE('',*,*,#13343,.F.);
#17929=ORIENTED_EDGE('',*,*,#13346,.F.);
#17930=ORIENTED_EDGE('',*,*,#13349,.F.);
#17931=ORIENTED_EDGE('',*,*,#13350,.T.);
#17932=ORIENTED_EDGE('',*,*,#13351,.T.);
#17933=ORIENTED_EDGE('',*,*,#13350,.F.);
#17934=ORIENTED_EDGE('',*,*,#13351,.F.);
#17935=ORIENTED_EDGE('',*,*,#13352,.F.);
#17936=ORIENTED_EDGE('',*,*,#13353,.T.);
#17937=ORIENTED_EDGE('',*,*,#13354,.T.);
#17938=ORIENTED_EDGE('',*,*,#13353,.F.);
#17939=ORIENTED_EDGE('',*,*,#13354,.F.);
#17940=ORIENTED_EDGE('',*,*,#13355,.F.);
#17941=ORIENTED_EDGE('',*,*,#13356,.T.);
#17942=ORIENTED_EDGE('',*,*,#13357,.T.);
#17943=ORIENTED_EDGE('',*,*,#13356,.F.);
#17944=ORIENTED_EDGE('',*,*,#13357,.F.);
#17945=ORIENTED_EDGE('',*,*,#13358,.F.);
#17946=ORIENTED_EDGE('',*,*,#13359,.T.);
#17947=ORIENTED_EDGE('',*,*,#13360,.T.);
#17948=ORIENTED_EDGE('',*,*,#13359,.F.);
#17949=ORIENTED_EDGE('',*,*,#13360,.F.);
#17950=ORIENTED_EDGE('',*,*,#13361,.F.);
#17951=ORIENTED_EDGE('',*,*,#13362,.T.);
#17952=ORIENTED_EDGE('',*,*,#13363,.T.);
#17953=ORIENTED_EDGE('',*,*,#13362,.F.);
#17954=ORIENTED_EDGE('',*,*,#13363,.F.);
#17955=ORIENTED_EDGE('',*,*,#13364,.F.);
#17956=ORIENTED_EDGE('',*,*,#13365,.T.);
#17957=ORIENTED_EDGE('',*,*,#13366,.T.);
#17958=ORIENTED_EDGE('',*,*,#13365,.F.);
#17959=ORIENTED_EDGE('',*,*,#13366,.F.);
#17960=ORIENTED_EDGE('',*,*,#13367,.F.);
#17961=ORIENTED_EDGE('',*,*,#13368,.T.);
#17962=ORIENTED_EDGE('',*,*,#13369,.T.);
#17963=ORIENTED_EDGE('',*,*,#13368,.F.);
#17964=ORIENTED_EDGE('',*,*,#13369,.F.);
#17965=ORIENTED_EDGE('',*,*,#13370,.F.);
#17966=ORIENTED_EDGE('',*,*,#13371,.T.);
#17967=ORIENTED_EDGE('',*,*,#13372,.T.);
#17968=ORIENTED_EDGE('',*,*,#13371,.F.);
#17969=ORIENTED_EDGE('',*,*,#13372,.F.);
#17970=ORIENTED_EDGE('',*,*,#13373,.F.);
#17971=ORIENTED_EDGE('',*,*,#13374,.T.);
#17972=ORIENTED_EDGE('',*,*,#13375,.F.);
#17973=ORIENTED_EDGE('',*,*,#13374,.F.);
#17974=ORIENTED_EDGE('',*,*,#13373,.T.);
#17975=ORIENTED_EDGE('',*,*,#13376,.F.);
#17976=ORIENTED_EDGE('',*,*,#13377,.F.);
#17977=ORIENTED_EDGE('',*,*,#13378,.T.);
#17978=ORIENTED_EDGE('',*,*,#13379,.F.);
#17979=ORIENTED_EDGE('',*,*,#13378,.F.);
#17980=ORIENTED_EDGE('',*,*,#13377,.T.);
#17981=ORIENTED_EDGE('',*,*,#13380,.F.);
#17982=ORIENTED_EDGE('',*,*,#13381,.F.);
#17983=ORIENTED_EDGE('',*,*,#13382,.T.);
#17984=ORIENTED_EDGE('',*,*,#13383,.F.);
#17985=ORIENTED_EDGE('',*,*,#13382,.F.);
#17986=ORIENTED_EDGE('',*,*,#13381,.T.);
#17987=ORIENTED_EDGE('',*,*,#13384,.F.);
#17988=ORIENTED_EDGE('',*,*,#13385,.F.);
#17989=ORIENTED_EDGE('',*,*,#13386,.T.);
#17990=ORIENTED_EDGE('',*,*,#13387,.F.);
#17991=ORIENTED_EDGE('',*,*,#13386,.F.);
#17992=ORIENTED_EDGE('',*,*,#13385,.T.);
#17993=ORIENTED_EDGE('',*,*,#13388,.F.);
#17994=ORIENTED_EDGE('',*,*,#13389,.F.);
#17995=ORIENTED_EDGE('',*,*,#13390,.T.);
#17996=ORIENTED_EDGE('',*,*,#13376,.T.);
#17997=ORIENTED_EDGE('',*,*,#13390,.F.);
#17998=ORIENTED_EDGE('',*,*,#13391,.F.);
#17999=ORIENTED_EDGE('',*,*,#13392,.T.);
#18000=ORIENTED_EDGE('',*,*,#13380,.T.);
#18001=ORIENTED_EDGE('',*,*,#13392,.F.);
#18002=ORIENTED_EDGE('',*,*,#13393,.F.);
#18003=ORIENTED_EDGE('',*,*,#13394,.T.);
#18004=ORIENTED_EDGE('',*,*,#13384,.T.);
#18005=ORIENTED_EDGE('',*,*,#13394,.F.);
#18006=ORIENTED_EDGE('',*,*,#13395,.F.);
#18007=ORIENTED_EDGE('',*,*,#13396,.T.);
#18008=ORIENTED_EDGE('',*,*,#13388,.T.);
#18009=ORIENTED_EDGE('',*,*,#13396,.F.);
#18010=ORIENTED_EDGE('',*,*,#13397,.F.);
#18011=ORIENTED_EDGE('',*,*,#13398,.T.);
#18012=ORIENTED_EDGE('',*,*,#13399,.F.);
#18013=ORIENTED_EDGE('',*,*,#13398,.F.);
#18014=ORIENTED_EDGE('',*,*,#13400,.F.);
#18015=ORIENTED_EDGE('',*,*,#13401,.T.);
#18016=ORIENTED_EDGE('',*,*,#13402,.F.);
#18017=ORIENTED_EDGE('',*,*,#13401,.F.);
#18018=ORIENTED_EDGE('',*,*,#13403,.F.);
#18019=ORIENTED_EDGE('',*,*,#13404,.T.);
#18020=ORIENTED_EDGE('',*,*,#13405,.F.);
#18021=ORIENTED_EDGE('',*,*,#13404,.F.);
#18022=ORIENTED_EDGE('',*,*,#13406,.F.);
#18023=ORIENTED_EDGE('',*,*,#13407,.T.);
#18024=ORIENTED_EDGE('',*,*,#13408,.F.);
#18025=ORIENTED_EDGE('',*,*,#13407,.F.);
#18026=ORIENTED_EDGE('',*,*,#13409,.F.);
#18027=ORIENTED_EDGE('',*,*,#13410,.T.);
#18028=ORIENTED_EDGE('',*,*,#13411,.F.);
#18029=ORIENTED_EDGE('',*,*,#13410,.F.);
#18030=ORIENTED_EDGE('',*,*,#13412,.F.);
#18031=ORIENTED_EDGE('',*,*,#13413,.T.);
#18032=ORIENTED_EDGE('',*,*,#13414,.F.);
#18033=ORIENTED_EDGE('',*,*,#13413,.F.);
#18034=ORIENTED_EDGE('',*,*,#13415,.F.);
#18035=ORIENTED_EDGE('',*,*,#13416,.T.);
#18036=ORIENTED_EDGE('',*,*,#13417,.F.);
#18037=ORIENTED_EDGE('',*,*,#13416,.F.);
#18038=ORIENTED_EDGE('',*,*,#13418,.F.);
#18039=ORIENTED_EDGE('',*,*,#13419,.T.);
#18040=ORIENTED_EDGE('',*,*,#13420,.F.);
#18041=ORIENTED_EDGE('',*,*,#13419,.F.);
#18042=ORIENTED_EDGE('',*,*,#13421,.F.);
#18043=ORIENTED_EDGE('',*,*,#13422,.T.);
#18044=ORIENTED_EDGE('',*,*,#13423,.F.);
#18045=ORIENTED_EDGE('',*,*,#13422,.F.);
#18046=ORIENTED_EDGE('',*,*,#13424,.F.);
#18047=ORIENTED_EDGE('',*,*,#13425,.T.);
#18048=ORIENTED_EDGE('',*,*,#13426,.F.);
#18049=ORIENTED_EDGE('',*,*,#13425,.F.);
#18050=ORIENTED_EDGE('',*,*,#13427,.T.);
#18051=ORIENTED_EDGE('',*,*,#13428,.T.);
#18052=ORIENTED_EDGE('',*,*,#13429,.F.);
#18053=ORIENTED_EDGE('',*,*,#13430,.F.);
#18054=ORIENTED_EDGE('',*,*,#13431,.T.);
#18055=ORIENTED_EDGE('',*,*,#13430,.T.);
#18056=ORIENTED_EDGE('',*,*,#13432,.F.);
#18057=ORIENTED_EDGE('',*,*,#13433,.F.);
#18058=ORIENTED_EDGE('',*,*,#13434,.T.);
#18059=ORIENTED_EDGE('',*,*,#13433,.T.);
#18060=ORIENTED_EDGE('',*,*,#13435,.F.);
#18061=ORIENTED_EDGE('',*,*,#13436,.F.);
#18062=ORIENTED_EDGE('',*,*,#13437,.T.);
#18063=ORIENTED_EDGE('',*,*,#13436,.T.);
#18064=ORIENTED_EDGE('',*,*,#13438,.F.);
#18065=ORIENTED_EDGE('',*,*,#13428,.F.);
#18066=ORIENTED_EDGE('',*,*,#13438,.T.);
#18067=ORIENTED_EDGE('',*,*,#13435,.T.);
#18068=ORIENTED_EDGE('',*,*,#13432,.T.);
#18069=ORIENTED_EDGE('',*,*,#13429,.T.);
#18070=ORIENTED_EDGE('',*,*,#13402,.T.);
#18071=ORIENTED_EDGE('',*,*,#13426,.T.);
#18072=ORIENTED_EDGE('',*,*,#13423,.T.);
#18073=ORIENTED_EDGE('',*,*,#13420,.T.);
#18074=ORIENTED_EDGE('',*,*,#13417,.T.);
#18075=ORIENTED_EDGE('',*,*,#13414,.T.);
#18076=ORIENTED_EDGE('',*,*,#13411,.T.);
#18077=ORIENTED_EDGE('',*,*,#13408,.T.);
#18078=ORIENTED_EDGE('',*,*,#13405,.T.);
#18079=ORIENTED_EDGE('',*,*,#13399,.T.);
#18080=ORIENTED_EDGE('',*,*,#13387,.T.);
#18081=ORIENTED_EDGE('',*,*,#13383,.T.);
#18082=ORIENTED_EDGE('',*,*,#13379,.T.);
#18083=ORIENTED_EDGE('',*,*,#13375,.T.);
#18084=ORIENTED_EDGE('',*,*,#13437,.F.);
#18085=ORIENTED_EDGE('',*,*,#13427,.F.);
#18086=ORIENTED_EDGE('',*,*,#13431,.F.);
#18087=ORIENTED_EDGE('',*,*,#13434,.F.);
#18088=ORIENTED_EDGE('',*,*,#13389,.T.);
#18089=ORIENTED_EDGE('',*,*,#13391,.T.);
#18090=ORIENTED_EDGE('',*,*,#13393,.T.);
#18091=ORIENTED_EDGE('',*,*,#13395,.T.);
#18092=ORIENTED_EDGE('',*,*,#13400,.T.);
#18093=ORIENTED_EDGE('',*,*,#13424,.T.);
#18094=ORIENTED_EDGE('',*,*,#13421,.T.);
#18095=ORIENTED_EDGE('',*,*,#13418,.T.);
#18096=ORIENTED_EDGE('',*,*,#13415,.T.);
#18097=ORIENTED_EDGE('',*,*,#13412,.T.);
#18098=ORIENTED_EDGE('',*,*,#13409,.T.);
#18099=ORIENTED_EDGE('',*,*,#13406,.T.);
#18100=ORIENTED_EDGE('',*,*,#13403,.T.);
#18101=ORIENTED_EDGE('',*,*,#13397,.T.);
#18102=ORIENTED_EDGE('',*,*,#13370,.T.);
#18103=ORIENTED_EDGE('',*,*,#13367,.T.);
#18104=ORIENTED_EDGE('',*,*,#13364,.T.);
#18105=ORIENTED_EDGE('',*,*,#13361,.T.);
#18106=ORIENTED_EDGE('',*,*,#13358,.T.);
#18107=ORIENTED_EDGE('',*,*,#13355,.T.);
#18108=ORIENTED_EDGE('',*,*,#13352,.T.);
#18109=ORIENTED_EDGE('',*,*,#13349,.T.);
#18110=ORIENTED_EDGE('',*,*,#13439,.F.);
#18111=ORIENTED_EDGE('',*,*,#13440,.F.);
#18112=ORIENTED_EDGE('',*,*,#13441,.T.);
#18113=ORIENTED_EDGE('',*,*,#13442,.F.);
#18114=ORIENTED_EDGE('',*,*,#13443,.F.);
#18115=ORIENTED_EDGE('',*,*,#13444,.F.);
#18116=ORIENTED_EDGE('',*,*,#13445,.T.);
#18117=ORIENTED_EDGE('',*,*,#13446,.F.);
#18118=ORIENTED_EDGE('',*,*,#13447,.F.);
#18119=ORIENTED_EDGE('',*,*,#13448,.T.);
#18120=ORIENTED_EDGE('',*,*,#13449,.F.);
#18121=ORIENTED_EDGE('',*,*,#13448,.F.);
#18122=ORIENTED_EDGE('',*,*,#13450,.F.);
#18123=ORIENTED_EDGE('',*,*,#13451,.T.);
#18124=ORIENTED_EDGE('',*,*,#13452,.F.);
#18125=ORIENTED_EDGE('',*,*,#13451,.F.);
#18126=ORIENTED_EDGE('',*,*,#13453,.F.);
#18127=ORIENTED_EDGE('',*,*,#13454,.T.);
#18128=ORIENTED_EDGE('',*,*,#13455,.F.);
#18129=ORIENTED_EDGE('',*,*,#13454,.F.);
#18130=ORIENTED_EDGE('',*,*,#13456,.F.);
#18131=ORIENTED_EDGE('',*,*,#13457,.T.);
#18132=ORIENTED_EDGE('',*,*,#13458,.F.);
#18133=ORIENTED_EDGE('',*,*,#13457,.F.);
#18134=ORIENTED_EDGE('',*,*,#13459,.F.);
#18135=ORIENTED_EDGE('',*,*,#13460,.T.);
#18136=ORIENTED_EDGE('',*,*,#13461,.F.);
#18137=ORIENTED_EDGE('',*,*,#13460,.F.);
#18138=ORIENTED_EDGE('',*,*,#13459,.T.);
#18139=ORIENTED_EDGE('',*,*,#13462,.F.);
#18140=ORIENTED_EDGE('',*,*,#13443,.T.);
#18141=ORIENTED_EDGE('',*,*,#13463,.F.);
#18142=ORIENTED_EDGE('',*,*,#13464,.F.);
#18143=ORIENTED_EDGE('',*,*,#13465,.F.);
#18144=ORIENTED_EDGE('',*,*,#13444,.T.);
#18145=ORIENTED_EDGE('',*,*,#13465,.T.);
#18146=ORIENTED_EDGE('',*,*,#13466,.F.);
#18147=ORIENTED_EDGE('',*,*,#13467,.F.);
#18148=ORIENTED_EDGE('',*,*,#13468,.T.);
#18149=ORIENTED_EDGE('',*,*,#13469,.F.);
#18150=ORIENTED_EDGE('',*,*,#13468,.F.);
#18151=ORIENTED_EDGE('',*,*,#13467,.T.);
#18152=ORIENTED_EDGE('',*,*,#13470,.F.);
#18153=ORIENTED_EDGE('',*,*,#13439,.T.);
#18154=ORIENTED_EDGE('',*,*,#13471,.F.);
#18155=ORIENTED_EDGE('',*,*,#13472,.F.);
#18156=ORIENTED_EDGE('',*,*,#13473,.F.);
#18157=ORIENTED_EDGE('',*,*,#13440,.T.);
#18158=ORIENTED_EDGE('',*,*,#13473,.T.);
#18159=ORIENTED_EDGE('',*,*,#13474,.F.);
#18160=ORIENTED_EDGE('',*,*,#13475,.T.);
#18161=ORIENTED_EDGE('',*,*,#13476,.T.);
#18162=ORIENTED_EDGE('',*,*,#13477,.T.);
#18163=ORIENTED_EDGE('',*,*,#13478,.T.);
#18164=ORIENTED_EDGE('',*,*,#13471,.T.);
#18165=ORIENTED_EDGE('',*,*,#13442,.T.);
#18166=ORIENTED_EDGE('',*,*,#13479,.T.);
#18167=ORIENTED_EDGE('',*,*,#13463,.T.);
#18168=ORIENTED_EDGE('',*,*,#13446,.T.);
#18169=ORIENTED_EDGE('',*,*,#13480,.T.);
#18170=ORIENTED_EDGE('',*,*,#13461,.T.);
#18171=ORIENTED_EDGE('',*,*,#13469,.T.);
#18172=ORIENTED_EDGE('',*,*,#13458,.T.);
#18173=ORIENTED_EDGE('',*,*,#13455,.T.);
#18174=ORIENTED_EDGE('',*,*,#13452,.T.);
#18175=ORIENTED_EDGE('',*,*,#13449,.T.);
#18176=ORIENTED_EDGE('',*,*,#13481,.F.);
#18177=ORIENTED_EDGE('',*,*,#13482,.T.);
#18178=ORIENTED_EDGE('',*,*,#13462,.T.);
#18179=ORIENTED_EDGE('',*,*,#13482,.F.);
#18180=ORIENTED_EDGE('',*,*,#13483,.F.);
#18181=ORIENTED_EDGE('',*,*,#13484,.T.);
#18182=ORIENTED_EDGE('',*,*,#13466,.T.);
#18183=ORIENTED_EDGE('',*,*,#13484,.F.);
#18184=ORIENTED_EDGE('',*,*,#13485,.F.);
#18185=ORIENTED_EDGE('',*,*,#13486,.T.);
#18186=ORIENTED_EDGE('',*,*,#13470,.T.);
#18187=ORIENTED_EDGE('',*,*,#13486,.F.);
#18188=ORIENTED_EDGE('',*,*,#13487,.F.);
#18189=ORIENTED_EDGE('',*,*,#13488,.T.);
#18190=ORIENTED_EDGE('',*,*,#13474,.T.);
#18191=ORIENTED_EDGE('',*,*,#13488,.F.);
#18192=ORIENTED_EDGE('',*,*,#13489,.T.);
#18193=ORIENTED_EDGE('',*,*,#13490,.T.);
#18194=ORIENTED_EDGE('',*,*,#13480,.F.);
#18195=ORIENTED_EDGE('',*,*,#13445,.F.);
#18196=ORIENTED_EDGE('',*,*,#13464,.T.);
#18197=ORIENTED_EDGE('',*,*,#13479,.F.);
#18198=ORIENTED_EDGE('',*,*,#13441,.F.);
#18199=ORIENTED_EDGE('',*,*,#13472,.T.);
#18200=ORIENTED_EDGE('',*,*,#13478,.F.);
#18201=ORIENTED_EDGE('',*,*,#13491,.F.);
#18202=ORIENTED_EDGE('',*,*,#13492,.T.);
#18203=ORIENTED_EDGE('',*,*,#13491,.T.);
#18204=ORIENTED_EDGE('',*,*,#13477,.F.);
#18205=ORIENTED_EDGE('',*,*,#13493,.F.);
#18206=ORIENTED_EDGE('',*,*,#13494,.T.);
#18207=ORIENTED_EDGE('',*,*,#13493,.T.);
#18208=ORIENTED_EDGE('',*,*,#13476,.F.);
#18209=ORIENTED_EDGE('',*,*,#13495,.F.);
#18210=ORIENTED_EDGE('',*,*,#13496,.T.);
#18211=ORIENTED_EDGE('',*,*,#13495,.T.);
#18212=ORIENTED_EDGE('',*,*,#13475,.F.);
#18213=ORIENTED_EDGE('',*,*,#13490,.F.);
#18214=ORIENTED_EDGE('',*,*,#13496,.F.);
#18215=ORIENTED_EDGE('',*,*,#13489,.F.);
#18216=ORIENTED_EDGE('',*,*,#13492,.F.);
#18217=ORIENTED_EDGE('',*,*,#13494,.F.);
#18218=ORIENTED_EDGE('',*,*,#13487,.T.);
#18219=ORIENTED_EDGE('',*,*,#13485,.T.);
#18220=ORIENTED_EDGE('',*,*,#13483,.T.);
#18221=ORIENTED_EDGE('',*,*,#13481,.T.);
#18222=ORIENTED_EDGE('',*,*,#13456,.T.);
#18223=ORIENTED_EDGE('',*,*,#13453,.T.);
#18224=ORIENTED_EDGE('',*,*,#13450,.T.);
#18225=ORIENTED_EDGE('',*,*,#13447,.T.);
#18226=ORIENTED_EDGE('',*,*,#13497,.F.);
#18227=ORIENTED_EDGE('',*,*,#13498,.T.);
#18228=ORIENTED_EDGE('',*,*,#13499,.F.);
#18229=ORIENTED_EDGE('',*,*,#13498,.F.);
#18230=ORIENTED_EDGE('',*,*,#13500,.F.);
#18231=ORIENTED_EDGE('',*,*,#13501,.T.);
#18232=ORIENTED_EDGE('',*,*,#13502,.F.);
#18233=ORIENTED_EDGE('',*,*,#13501,.F.);
#18234=ORIENTED_EDGE('',*,*,#13503,.F.);
#18235=ORIENTED_EDGE('',*,*,#13504,.T.);
#18236=ORIENTED_EDGE('',*,*,#13505,.F.);
#18237=ORIENTED_EDGE('',*,*,#13504,.F.);
#18238=ORIENTED_EDGE('',*,*,#13506,.F.);
#18239=ORIENTED_EDGE('',*,*,#13507,.T.);
#18240=ORIENTED_EDGE('',*,*,#13508,.T.);
#18241=ORIENTED_EDGE('',*,*,#13507,.F.);
#18242=ORIENTED_EDGE('',*,*,#13508,.F.);
#18243=ORIENTED_EDGE('',*,*,#13509,.F.);
#18244=ORIENTED_EDGE('',*,*,#13509,.T.);
#18245=ORIENTED_EDGE('',*,*,#13510,.T.);
#18246=ORIENTED_EDGE('',*,*,#13511,.F.);
#18247=ORIENTED_EDGE('',*,*,#13510,.F.);
#18248=ORIENTED_EDGE('',*,*,#13512,.F.);
#18249=ORIENTED_EDGE('',*,*,#13513,.T.);
#18250=ORIENTED_EDGE('',*,*,#13514,.T.);
#18251=ORIENTED_EDGE('',*,*,#13513,.F.);
#18252=ORIENTED_EDGE('',*,*,#13514,.F.);
#18253=ORIENTED_EDGE('',*,*,#13515,.F.);
#18254=ORIENTED_EDGE('',*,*,#13516,.T.);
#18255=ORIENTED_EDGE('',*,*,#13517,.T.);
#18256=ORIENTED_EDGE('',*,*,#13516,.F.);
#18257=ORIENTED_EDGE('',*,*,#13517,.F.);
#18258=ORIENTED_EDGE('',*,*,#13518,.T.);
#18259=ORIENTED_EDGE('',*,*,#13519,.T.);
#18260=ORIENTED_EDGE('',*,*,#13520,.F.);
#18261=ORIENTED_EDGE('',*,*,#13521,.F.);
#18262=ORIENTED_EDGE('',*,*,#13522,.T.);
#18263=ORIENTED_EDGE('',*,*,#13521,.T.);
#18264=ORIENTED_EDGE('',*,*,#13523,.F.);
#18265=ORIENTED_EDGE('',*,*,#13524,.F.);
#18266=ORIENTED_EDGE('',*,*,#13499,.T.);
#18267=ORIENTED_EDGE('',*,*,#13502,.T.);
#18268=ORIENTED_EDGE('',*,*,#13505,.T.);
#18269=ORIENTED_EDGE('',*,*,#13511,.T.);
#18270=ORIENTED_EDGE('',*,*,#13525,.T.);
#18271=ORIENTED_EDGE('',*,*,#13524,.T.);
#18272=ORIENTED_EDGE('',*,*,#13526,.F.);
#18273=ORIENTED_EDGE('',*,*,#13527,.F.);
#18274=ORIENTED_EDGE('',*,*,#13528,.T.);
#18275=ORIENTED_EDGE('',*,*,#13527,.T.);
#18276=ORIENTED_EDGE('',*,*,#13529,.F.);
#18277=ORIENTED_EDGE('',*,*,#13519,.F.);
#18278=ORIENTED_EDGE('',*,*,#13497,.T.);
#18279=ORIENTED_EDGE('',*,*,#13500,.T.);
#18280=ORIENTED_EDGE('',*,*,#13503,.T.);
#18281=ORIENTED_EDGE('',*,*,#13506,.T.);
#18282=ORIENTED_EDGE('',*,*,#13529,.T.);
#18283=ORIENTED_EDGE('',*,*,#13526,.T.);
#18284=ORIENTED_EDGE('',*,*,#13523,.T.);
#18285=ORIENTED_EDGE('',*,*,#13520,.T.);
#18286=ORIENTED_EDGE('',*,*,#13528,.F.);
#18287=ORIENTED_EDGE('',*,*,#13518,.F.);
#18288=ORIENTED_EDGE('',*,*,#13522,.F.);
#18289=ORIENTED_EDGE('',*,*,#13525,.F.);
#18290=ORIENTED_EDGE('',*,*,#13512,.T.);
#18291=ORIENTED_EDGE('',*,*,#13515,.T.);
#18292=ORIENTED_EDGE('',*,*,#13530,.F.);
#18293=ORIENTED_EDGE('',*,*,#13531,.T.);
#18294=ORIENTED_EDGE('',*,*,#13532,.F.);
#18295=ORIENTED_EDGE('',*,*,#13531,.F.);
#18296=ORIENTED_EDGE('',*,*,#13533,.F.);
#18297=ORIENTED_EDGE('',*,*,#13534,.T.);
#18298=ORIENTED_EDGE('',*,*,#13535,.F.);
#18299=ORIENTED_EDGE('',*,*,#13534,.F.);
#18300=ORIENTED_EDGE('',*,*,#13536,.F.);
#18301=ORIENTED_EDGE('',*,*,#13537,.T.);
#18302=ORIENTED_EDGE('',*,*,#13538,.F.);
#18303=ORIENTED_EDGE('',*,*,#13537,.F.);
#18304=ORIENTED_EDGE('',*,*,#13539,.F.);
#18305=ORIENTED_EDGE('',*,*,#13540,.T.);
#18306=ORIENTED_EDGE('',*,*,#13541,.F.);
#18307=ORIENTED_EDGE('',*,*,#13540,.F.);
#18308=ORIENTED_EDGE('',*,*,#13539,.T.);
#18309=ORIENTED_EDGE('',*,*,#13542,.T.);
#18310=ORIENTED_EDGE('',*,*,#13542,.F.);
#18311=ORIENTED_EDGE('',*,*,#13543,.T.);
#18312=ORIENTED_EDGE('',*,*,#13544,.T.);
#18313=ORIENTED_EDGE('',*,*,#13543,.F.);
#18314=ORIENTED_EDGE('',*,*,#13545,.F.);
#18315=ORIENTED_EDGE('',*,*,#13546,.T.);
#18316=ORIENTED_EDGE('',*,*,#13547,.T.);
#18317=ORIENTED_EDGE('',*,*,#13546,.F.);
#18318=ORIENTED_EDGE('',*,*,#13545,.T.);
#18319=ORIENTED_EDGE('',*,*,#13532,.T.);
#18320=ORIENTED_EDGE('',*,*,#13535,.T.);
#18321=ORIENTED_EDGE('',*,*,#13538,.T.);
#18322=ORIENTED_EDGE('',*,*,#13541,.T.);
#18323=ORIENTED_EDGE('',*,*,#13547,.F.);
#18324=ORIENTED_EDGE('',*,*,#13530,.T.);
#18325=ORIENTED_EDGE('',*,*,#13533,.T.);
#18326=ORIENTED_EDGE('',*,*,#13536,.T.);
#18327=ORIENTED_EDGE('',*,*,#13544,.F.);
#18328=ORIENTED_EDGE('',*,*,#13548,.F.);
#18329=ORIENTED_EDGE('',*,*,#13549,.T.);
#18330=ORIENTED_EDGE('',*,*,#13550,.F.);
#18331=ORIENTED_EDGE('',*,*,#13549,.F.);
#18332=ORIENTED_EDGE('',*,*,#13551,.F.);
#18333=ORIENTED_EDGE('',*,*,#13552,.T.);
#18334=ORIENTED_EDGE('',*,*,#13553,.F.);
#18335=ORIENTED_EDGE('',*,*,#13552,.F.);
#18336=ORIENTED_EDGE('',*,*,#13554,.F.);
#18337=ORIENTED_EDGE('',*,*,#13555,.T.);
#18338=ORIENTED_EDGE('',*,*,#13556,.F.);
#18339=ORIENTED_EDGE('',*,*,#13555,.F.);
#18340=ORIENTED_EDGE('',*,*,#13557,.F.);
#18341=ORIENTED_EDGE('',*,*,#13558,.T.);
#18342=ORIENTED_EDGE('',*,*,#13559,.F.);
#18343=ORIENTED_EDGE('',*,*,#13558,.F.);
#18344=ORIENTED_EDGE('',*,*,#13557,.T.);
#18345=ORIENTED_EDGE('',*,*,#13560,.F.);
#18346=ORIENTED_EDGE('',*,*,#13561,.F.);
#18347=ORIENTED_EDGE('',*,*,#13562,.T.);
#18348=ORIENTED_EDGE('',*,*,#13560,.T.);
#18349=ORIENTED_EDGE('',*,*,#13562,.F.);
#18350=ORIENTED_EDGE('',*,*,#13563,.F.);
#18351=ORIENTED_EDGE('',*,*,#13564,.T.);
#18352=ORIENTED_EDGE('',*,*,#13565,.T.);
#18353=ORIENTED_EDGE('',*,*,#13564,.F.);
#18354=ORIENTED_EDGE('',*,*,#13565,.F.);
#18355=ORIENTED_EDGE('',*,*,#13566,.F.);
#18356=ORIENTED_EDGE('',*,*,#13567,.T.);
#18357=ORIENTED_EDGE('',*,*,#13568,.T.);
#18358=ORIENTED_EDGE('',*,*,#13567,.F.);
#18359=ORIENTED_EDGE('',*,*,#13568,.F.);
#18360=ORIENTED_EDGE('',*,*,#13569,.T.);
#18361=ORIENTED_EDGE('',*,*,#13570,.T.);
#18362=ORIENTED_EDGE('',*,*,#13571,.F.);
#18363=ORIENTED_EDGE('',*,*,#13572,.F.);
#18364=ORIENTED_EDGE('',*,*,#13573,.T.);
#18365=ORIENTED_EDGE('',*,*,#13572,.T.);
#18366=ORIENTED_EDGE('',*,*,#13574,.F.);
#18367=ORIENTED_EDGE('',*,*,#13575,.F.);
#18368=ORIENTED_EDGE('',*,*,#13550,.T.);
#18369=ORIENTED_EDGE('',*,*,#13553,.T.);
#18370=ORIENTED_EDGE('',*,*,#13556,.T.);
#18371=ORIENTED_EDGE('',*,*,#13559,.T.);
#18372=ORIENTED_EDGE('',*,*,#13576,.T.);
#18373=ORIENTED_EDGE('',*,*,#13575,.T.);
#18374=ORIENTED_EDGE('',*,*,#13577,.F.);
#18375=ORIENTED_EDGE('',*,*,#13578,.F.);
#18376=ORIENTED_EDGE('',*,*,#13579,.T.);
#18377=ORIENTED_EDGE('',*,*,#13578,.T.);
#18378=ORIENTED_EDGE('',*,*,#13580,.F.);
#18379=ORIENTED_EDGE('',*,*,#13570,.F.);
#18380=ORIENTED_EDGE('',*,*,#13548,.T.);
#18381=ORIENTED_EDGE('',*,*,#13551,.T.);
#18382=ORIENTED_EDGE('',*,*,#13554,.T.);
#18383=ORIENTED_EDGE('',*,*,#13561,.T.);
#18384=ORIENTED_EDGE('',*,*,#13580,.T.);
#18385=ORIENTED_EDGE('',*,*,#13577,.T.);
#18386=ORIENTED_EDGE('',*,*,#13574,.T.);
#18387=ORIENTED_EDGE('',*,*,#13571,.T.);
#18388=ORIENTED_EDGE('',*,*,#13579,.F.);
#18389=ORIENTED_EDGE('',*,*,#13569,.F.);
#18390=ORIENTED_EDGE('',*,*,#13573,.F.);
#18391=ORIENTED_EDGE('',*,*,#13576,.F.);
#18392=ORIENTED_EDGE('',*,*,#13563,.T.);
#18393=ORIENTED_EDGE('',*,*,#13566,.T.);
#18394=ORIENTED_EDGE('',*,*,#13581,.F.);
#18395=ORIENTED_EDGE('',*,*,#13582,.T.);
#18396=ORIENTED_EDGE('',*,*,#13583,.F.);
#18397=ORIENTED_EDGE('',*,*,#13582,.F.);
#18398=ORIENTED_EDGE('',*,*,#13584,.F.);
#18399=ORIENTED_EDGE('',*,*,#13585,.T.);
#18400=ORIENTED_EDGE('',*,*,#13586,.F.);
#18401=ORIENTED_EDGE('',*,*,#13585,.F.);
#18402=ORIENTED_EDGE('',*,*,#13587,.F.);
#18403=ORIENTED_EDGE('',*,*,#13588,.T.);
#18404=ORIENTED_EDGE('',*,*,#13589,.F.);
#18405=ORIENTED_EDGE('',*,*,#13588,.F.);
#18406=ORIENTED_EDGE('',*,*,#13590,.F.);
#18407=ORIENTED_EDGE('',*,*,#13591,.F.);
#18408=ORIENTED_EDGE('',*,*,#13592,.F.);
#18409=ORIENTED_EDGE('',*,*,#13593,.F.);
#18410=ORIENTED_EDGE('',*,*,#13591,.T.);
#18411=ORIENTED_EDGE('',*,*,#13594,.F.);
#18412=ORIENTED_EDGE('',*,*,#13581,.T.);
#18413=ORIENTED_EDGE('',*,*,#13584,.T.);
#18414=ORIENTED_EDGE('',*,*,#13587,.T.);
#18415=ORIENTED_EDGE('',*,*,#13595,.T.);
#18416=ORIENTED_EDGE('',*,*,#13592,.T.);
#18417=ORIENTED_EDGE('',*,*,#13594,.T.);
#18418=ORIENTED_EDGE('',*,*,#13590,.T.);
#18419=ORIENTED_EDGE('',*,*,#13596,.F.);
#18420=ORIENTED_EDGE('',*,*,#13595,.F.);
#18421=ORIENTED_EDGE('',*,*,#13597,.T.);
#18422=ORIENTED_EDGE('',*,*,#13598,.T.);
#18423=ORIENTED_EDGE('',*,*,#13597,.F.);
#18424=ORIENTED_EDGE('',*,*,#13598,.F.);
#18425=ORIENTED_EDGE('',*,*,#13599,.F.);
#18426=ORIENTED_EDGE('',*,*,#13600,.F.);
#18427=ORIENTED_EDGE('',*,*,#13601,.T.);
#18428=ORIENTED_EDGE('',*,*,#13599,.T.);
#18429=ORIENTED_EDGE('',*,*,#13601,.F.);
#18430=ORIENTED_EDGE('',*,*,#13593,.T.);
#18431=ORIENTED_EDGE('',*,*,#13596,.T.);
#18432=ORIENTED_EDGE('',*,*,#13583,.T.);
#18433=ORIENTED_EDGE('',*,*,#13586,.T.);
#18434=ORIENTED_EDGE('',*,*,#13589,.T.);
#18435=ORIENTED_EDGE('',*,*,#13600,.T.);
#18436=ORIENTED_EDGE('',*,*,#13602,.F.);
#18437=ORIENTED_EDGE('',*,*,#13603,.T.);
#18438=ORIENTED_EDGE('',*,*,#13604,.F.);
#18439=ORIENTED_EDGE('',*,*,#13603,.F.);
#18440=ORIENTED_EDGE('',*,*,#13602,.T.);
#18441=ORIENTED_EDGE('',*,*,#13605,.F.);
#18442=ORIENTED_EDGE('',*,*,#13606,.F.);
#18443=ORIENTED_EDGE('',*,*,#13607,.T.);
#18444=ORIENTED_EDGE('',*,*,#13605,.T.);
#18445=ORIENTED_EDGE('',*,*,#13607,.F.);
#18446=ORIENTED_EDGE('',*,*,#13608,.T.);
#18447=ORIENTED_EDGE('',*,*,#13609,.T.);
#18448=ORIENTED_EDGE('',*,*,#13610,.F.);
#18449=ORIENTED_EDGE('',*,*,#13611,.F.);
#18450=ORIENTED_EDGE('',*,*,#13612,.T.);
#18451=ORIENTED_EDGE('',*,*,#13611,.T.);
#18452=ORIENTED_EDGE('',*,*,#13613,.F.);
#18453=ORIENTED_EDGE('',*,*,#13614,.F.);
#18454=ORIENTED_EDGE('',*,*,#13615,.T.);
#18455=ORIENTED_EDGE('',*,*,#13614,.T.);
#18456=ORIENTED_EDGE('',*,*,#13616,.F.);
#18457=ORIENTED_EDGE('',*,*,#13617,.F.);
#18458=ORIENTED_EDGE('',*,*,#13618,.T.);
#18459=ORIENTED_EDGE('',*,*,#13617,.T.);
#18460=ORIENTED_EDGE('',*,*,#13619,.F.);
#18461=ORIENTED_EDGE('',*,*,#13609,.F.);
#18462=ORIENTED_EDGE('',*,*,#13619,.T.);
#18463=ORIENTED_EDGE('',*,*,#13616,.T.);
#18464=ORIENTED_EDGE('',*,*,#13613,.T.);
#18465=ORIENTED_EDGE('',*,*,#13610,.T.);
#18466=ORIENTED_EDGE('',*,*,#13604,.T.);
#18467=ORIENTED_EDGE('',*,*,#13618,.F.);
#18468=ORIENTED_EDGE('',*,*,#13608,.F.);
#18469=ORIENTED_EDGE('',*,*,#13612,.F.);
#18470=ORIENTED_EDGE('',*,*,#13615,.F.);
#18471=ORIENTED_EDGE('',*,*,#13606,.T.);
#18472=ORIENTED_EDGE('',*,*,#13620,.F.);
#18473=ORIENTED_EDGE('',*,*,#13621,.T.);
#18474=ORIENTED_EDGE('',*,*,#13622,.F.);
#18475=ORIENTED_EDGE('',*,*,#13621,.F.);
#18476=ORIENTED_EDGE('',*,*,#13620,.T.);
#18477=ORIENTED_EDGE('',*,*,#13623,.F.);
#18478=ORIENTED_EDGE('',*,*,#13624,.F.);
#18479=ORIENTED_EDGE('',*,*,#13625,.T.);
#18480=ORIENTED_EDGE('',*,*,#13623,.T.);
#18481=ORIENTED_EDGE('',*,*,#13625,.F.);
#18482=ORIENTED_EDGE('',*,*,#13626,.T.);
#18483=ORIENTED_EDGE('',*,*,#13627,.T.);
#18484=ORIENTED_EDGE('',*,*,#13628,.F.);
#18485=ORIENTED_EDGE('',*,*,#13629,.F.);
#18486=ORIENTED_EDGE('',*,*,#13630,.T.);
#18487=ORIENTED_EDGE('',*,*,#13629,.T.);
#18488=ORIENTED_EDGE('',*,*,#13631,.F.);
#18489=ORIENTED_EDGE('',*,*,#13632,.F.);
#18490=ORIENTED_EDGE('',*,*,#13633,.T.);
#18491=ORIENTED_EDGE('',*,*,#13632,.T.);
#18492=ORIENTED_EDGE('',*,*,#13634,.F.);
#18493=ORIENTED_EDGE('',*,*,#13635,.F.);
#18494=ORIENTED_EDGE('',*,*,#13636,.T.);
#18495=ORIENTED_EDGE('',*,*,#13635,.T.);
#18496=ORIENTED_EDGE('',*,*,#13637,.F.);
#18497=ORIENTED_EDGE('',*,*,#13627,.F.);
#18498=ORIENTED_EDGE('',*,*,#13637,.T.);
#18499=ORIENTED_EDGE('',*,*,#13634,.T.);
#18500=ORIENTED_EDGE('',*,*,#13631,.T.);
#18501=ORIENTED_EDGE('',*,*,#13628,.T.);
#18502=ORIENTED_EDGE('',*,*,#13622,.T.);
#18503=ORIENTED_EDGE('',*,*,#13636,.F.);
#18504=ORIENTED_EDGE('',*,*,#13626,.F.);
#18505=ORIENTED_EDGE('',*,*,#13630,.F.);
#18506=ORIENTED_EDGE('',*,*,#13633,.F.);
#18507=ORIENTED_EDGE('',*,*,#13624,.T.);
#18508=ORIENTED_EDGE('',*,*,#13638,.F.);
#18509=ORIENTED_EDGE('',*,*,#13639,.T.);
#18510=ORIENTED_EDGE('',*,*,#13640,.F.);
#18511=ORIENTED_EDGE('',*,*,#13639,.F.);
#18512=ORIENTED_EDGE('',*,*,#13638,.T.);
#18513=ORIENTED_EDGE('',*,*,#13641,.F.);
#18514=ORIENTED_EDGE('',*,*,#13642,.F.);
#18515=ORIENTED_EDGE('',*,*,#13643,.T.);
#18516=ORIENTED_EDGE('',*,*,#13644,.F.);
#18517=ORIENTED_EDGE('',*,*,#13643,.F.);
#18518=ORIENTED_EDGE('',*,*,#13642,.T.);
#18519=ORIENTED_EDGE('',*,*,#13645,.F.);
#18520=ORIENTED_EDGE('',*,*,#13646,.F.);
#18521=ORIENTED_EDGE('',*,*,#13647,.T.);
#18522=ORIENTED_EDGE('',*,*,#13648,.F.);
#18523=ORIENTED_EDGE('',*,*,#13647,.F.);
#18524=ORIENTED_EDGE('',*,*,#13646,.T.);
#18525=ORIENTED_EDGE('',*,*,#13649,.F.);
#18526=ORIENTED_EDGE('',*,*,#13650,.F.);
#18527=ORIENTED_EDGE('',*,*,#13651,.T.);
#18528=ORIENTED_EDGE('',*,*,#13652,.F.);
#18529=ORIENTED_EDGE('',*,*,#13651,.F.);
#18530=ORIENTED_EDGE('',*,*,#13650,.T.);
#18531=ORIENTED_EDGE('',*,*,#13653,.F.);
#18532=ORIENTED_EDGE('',*,*,#13654,.F.);
#18533=ORIENTED_EDGE('',*,*,#13655,.T.);
#18534=ORIENTED_EDGE('',*,*,#13641,.T.);
#18535=ORIENTED_EDGE('',*,*,#13655,.F.);
#18536=ORIENTED_EDGE('',*,*,#13656,.F.);
#18537=ORIENTED_EDGE('',*,*,#13657,.T.);
#18538=ORIENTED_EDGE('',*,*,#13645,.T.);
#18539=ORIENTED_EDGE('',*,*,#13657,.F.);
#18540=ORIENTED_EDGE('',*,*,#13658,.F.);
#18541=ORIENTED_EDGE('',*,*,#13659,.T.);
#18542=ORIENTED_EDGE('',*,*,#13649,.T.);
#18543=ORIENTED_EDGE('',*,*,#13659,.F.);
#18544=ORIENTED_EDGE('',*,*,#13660,.F.);
#18545=ORIENTED_EDGE('',*,*,#13661,.T.);
#18546=ORIENTED_EDGE('',*,*,#13653,.T.);
#18547=ORIENTED_EDGE('',*,*,#13661,.F.);
#18548=ORIENTED_EDGE('',*,*,#13662,.T.);
#18549=ORIENTED_EDGE('',*,*,#13663,.T.);
#18550=ORIENTED_EDGE('',*,*,#13664,.F.);
#18551=ORIENTED_EDGE('',*,*,#13665,.F.);
#18552=ORIENTED_EDGE('',*,*,#13666,.T.);
#18553=ORIENTED_EDGE('',*,*,#13665,.T.);
#18554=ORIENTED_EDGE('',*,*,#13667,.F.);
#18555=ORIENTED_EDGE('',*,*,#13668,.F.);
#18556=ORIENTED_EDGE('',*,*,#13669,.T.);
#18557=ORIENTED_EDGE('',*,*,#13668,.T.);
#18558=ORIENTED_EDGE('',*,*,#13670,.F.);
#18559=ORIENTED_EDGE('',*,*,#13671,.F.);
#18560=ORIENTED_EDGE('',*,*,#13672,.T.);
#18561=ORIENTED_EDGE('',*,*,#13671,.T.);
#18562=ORIENTED_EDGE('',*,*,#13673,.F.);
#18563=ORIENTED_EDGE('',*,*,#13674,.F.);
#18564=ORIENTED_EDGE('',*,*,#13675,.T.);
#18565=ORIENTED_EDGE('',*,*,#13674,.T.);
#18566=ORIENTED_EDGE('',*,*,#13676,.F.);
#18567=ORIENTED_EDGE('',*,*,#13677,.F.);
#18568=ORIENTED_EDGE('',*,*,#13652,.T.);
#18569=ORIENTED_EDGE('',*,*,#13648,.T.);
#18570=ORIENTED_EDGE('',*,*,#13644,.T.);
#18571=ORIENTED_EDGE('',*,*,#13640,.T.);
#18572=ORIENTED_EDGE('',*,*,#13678,.T.);
#18573=ORIENTED_EDGE('',*,*,#13677,.T.);
#18574=ORIENTED_EDGE('',*,*,#13679,.F.);
#18575=ORIENTED_EDGE('',*,*,#13680,.F.);
#18576=ORIENTED_EDGE('',*,*,#13681,.T.);
#18577=ORIENTED_EDGE('',*,*,#13680,.T.);
#18578=ORIENTED_EDGE('',*,*,#13682,.F.);
#18579=ORIENTED_EDGE('',*,*,#13683,.F.);
#18580=ORIENTED_EDGE('',*,*,#13684,.T.);
#18581=ORIENTED_EDGE('',*,*,#13683,.T.);
#18582=ORIENTED_EDGE('',*,*,#13685,.F.);
#18583=ORIENTED_EDGE('',*,*,#13686,.F.);
#18584=ORIENTED_EDGE('',*,*,#13687,.T.);
#18585=ORIENTED_EDGE('',*,*,#13686,.T.);
#18586=ORIENTED_EDGE('',*,*,#13688,.F.);
#18587=ORIENTED_EDGE('',*,*,#13689,.F.);
#18588=ORIENTED_EDGE('',*,*,#13690,.T.);
#18589=ORIENTED_EDGE('',*,*,#13689,.T.);
#18590=ORIENTED_EDGE('',*,*,#13691,.F.);
#18591=ORIENTED_EDGE('',*,*,#13692,.F.);
#18592=ORIENTED_EDGE('',*,*,#13693,.T.);
#18593=ORIENTED_EDGE('',*,*,#13692,.T.);
#18594=ORIENTED_EDGE('',*,*,#13694,.F.);
#18595=ORIENTED_EDGE('',*,*,#13695,.F.);
#18596=ORIENTED_EDGE('',*,*,#13654,.T.);
#18597=ORIENTED_EDGE('',*,*,#13656,.T.);
#18598=ORIENTED_EDGE('',*,*,#13658,.T.);
#18599=ORIENTED_EDGE('',*,*,#13660,.T.);
#18600=ORIENTED_EDGE('',*,*,#13696,.T.);
#18601=ORIENTED_EDGE('',*,*,#13695,.T.);
#18602=ORIENTED_EDGE('',*,*,#13697,.F.);
#18603=ORIENTED_EDGE('',*,*,#13663,.F.);
#18604=ORIENTED_EDGE('',*,*,#13697,.T.);
#18605=ORIENTED_EDGE('',*,*,#13694,.T.);
#18606=ORIENTED_EDGE('',*,*,#13691,.T.);
#18607=ORIENTED_EDGE('',*,*,#13688,.T.);
#18608=ORIENTED_EDGE('',*,*,#13685,.T.);
#18609=ORIENTED_EDGE('',*,*,#13682,.T.);
#18610=ORIENTED_EDGE('',*,*,#13679,.T.);
#18611=ORIENTED_EDGE('',*,*,#13676,.T.);
#18612=ORIENTED_EDGE('',*,*,#13673,.T.);
#18613=ORIENTED_EDGE('',*,*,#13670,.T.);
#18614=ORIENTED_EDGE('',*,*,#13667,.T.);
#18615=ORIENTED_EDGE('',*,*,#13664,.T.);
#18616=ORIENTED_EDGE('',*,*,#13696,.F.);
#18617=ORIENTED_EDGE('',*,*,#13662,.F.);
#18618=ORIENTED_EDGE('',*,*,#13666,.F.);
#18619=ORIENTED_EDGE('',*,*,#13669,.F.);
#18620=ORIENTED_EDGE('',*,*,#13672,.F.);
#18621=ORIENTED_EDGE('',*,*,#13675,.F.);
#18622=ORIENTED_EDGE('',*,*,#13678,.F.);
#18623=ORIENTED_EDGE('',*,*,#13681,.F.);
#18624=ORIENTED_EDGE('',*,*,#13684,.F.);
#18625=ORIENTED_EDGE('',*,*,#13687,.F.);
#18626=ORIENTED_EDGE('',*,*,#13690,.F.);
#18627=ORIENTED_EDGE('',*,*,#13693,.F.);
#18628=ORIENTED_EDGE('',*,*,#13698,.F.);
#18629=ORIENTED_EDGE('',*,*,#13699,.F.);
#18630=ORIENTED_EDGE('',*,*,#13700,.T.);
#18631=ORIENTED_EDGE('',*,*,#13701,.F.);
#18632=ORIENTED_EDGE('',*,*,#13702,.F.);
#18633=ORIENTED_EDGE('',*,*,#13700,.F.);
#18634=ORIENTED_EDGE('',*,*,#13701,.T.);
#18635=ORIENTED_EDGE('',*,*,#13702,.T.);
#18636=ORIENTED_EDGE('',*,*,#13703,.T.);
#18637=ORIENTED_EDGE('',*,*,#13704,.T.);
#18638=ORIENTED_EDGE('',*,*,#13703,.F.);
#18639=ORIENTED_EDGE('',*,*,#13705,.T.);
#18640=ORIENTED_EDGE('',*,*,#13706,.T.);
#18641=ORIENTED_EDGE('',*,*,#13707,.F.);
#18642=ORIENTED_EDGE('',*,*,#13706,.F.);
#18643=ORIENTED_EDGE('',*,*,#13707,.T.);
#18644=ORIENTED_EDGE('',*,*,#13708,.T.);
#18645=ORIENTED_EDGE('',*,*,#13709,.F.);
#18646=ORIENTED_EDGE('',*,*,#13708,.F.);
#18647=ORIENTED_EDGE('',*,*,#13704,.F.);
#18648=ORIENTED_EDGE('',*,*,#13709,.T.);
#18649=ORIENTED_EDGE('',*,*,#13710,.F.);
#18650=ORIENTED_EDGE('',*,*,#13711,.T.);
#18651=ORIENTED_EDGE('',*,*,#13698,.T.);
#18652=ORIENTED_EDGE('',*,*,#13699,.T.);
#18653=ORIENTED_EDGE('',*,*,#13711,.F.);
#18654=ORIENTED_EDGE('',*,*,#13710,.T.);
#18655=ORIENTED_EDGE('',*,*,#13712,.F.);
#18656=ORIENTED_EDGE('',*,*,#13712,.T.);
#18657=ORIENTED_EDGE('',*,*,#13713,.T.);
#18658=ORIENTED_EDGE('',*,*,#13705,.F.);
#18659=ORIENTED_EDGE('',*,*,#13713,.F.);
#18660=ORIENTED_EDGE('',*,*,#13714,.F.);
#18661=ORIENTED_EDGE('',*,*,#13715,.F.);
#18662=ORIENTED_EDGE('',*,*,#13716,.T.);
#18663=ORIENTED_EDGE('',*,*,#13717,.F.);
#18664=ORIENTED_EDGE('',*,*,#13718,.F.);
#18665=ORIENTED_EDGE('',*,*,#13716,.F.);
#18666=ORIENTED_EDGE('',*,*,#13719,.T.);
#18667=ORIENTED_EDGE('',*,*,#13720,.T.);
#18668=ORIENTED_EDGE('',*,*,#13717,.T.);
#18669=ORIENTED_EDGE('',*,*,#13718,.T.);
#18670=ORIENTED_EDGE('',*,*,#13720,.F.);
#18671=ORIENTED_EDGE('',*,*,#13721,.F.);
#18672=ORIENTED_EDGE('',*,*,#13722,.T.);
#18673=ORIENTED_EDGE('',*,*,#13723,.F.);
#18674=ORIENTED_EDGE('',*,*,#13724,.T.);
#18675=ORIENTED_EDGE('',*,*,#13721,.T.);
#18676=ORIENTED_EDGE('',*,*,#13724,.F.);
#18677=ORIENTED_EDGE('',*,*,#13725,.F.);
#18678=ORIENTED_EDGE('',*,*,#13726,.T.);
#18679=ORIENTED_EDGE('',*,*,#13723,.T.);
#18680=ORIENTED_EDGE('',*,*,#13726,.F.);
#18681=ORIENTED_EDGE('',*,*,#13727,.F.);
#18682=ORIENTED_EDGE('',*,*,#13728,.T.);
#18683=ORIENTED_EDGE('',*,*,#13725,.T.);
#18684=ORIENTED_EDGE('',*,*,#13728,.F.);
#18685=ORIENTED_EDGE('',*,*,#13727,.T.);
#18686=ORIENTED_EDGE('',*,*,#13719,.F.);
#18687=ORIENTED_EDGE('',*,*,#13714,.T.);
#18688=ORIENTED_EDGE('',*,*,#13715,.T.);
#18689=ORIENTED_EDGE('',*,*,#13729,.T.);
#18690=ORIENTED_EDGE('',*,*,#13722,.F.);
#18691=ORIENTED_EDGE('',*,*,#13729,.F.);
#18692=ORIENTED_EDGE('',*,*,#13730,.T.);
#18693=ORIENTED_EDGE('',*,*,#13730,.F.);
#18694=ORIENTED_EDGE('',*,*,#13731,.T.);
#18695=ORIENTED_EDGE('',*,*,#13731,.F.);
#18696=ORIENTED_EDGE('',*,*,#13732,.T.);
#18697=ORIENTED_EDGE('',*,*,#13732,.F.);
#18698=ORIENTED_EDGE('',*,*,#13733,.T.);
#18699=ORIENTED_EDGE('',*,*,#13733,.F.);
#18700=ORIENTED_EDGE('',*,*,#13734,.T.);
#18701=ORIENTED_EDGE('',*,*,#13734,.F.);
#18702=ORIENTED_EDGE('',*,*,#13735,.T.);
#18703=ORIENTED_EDGE('',*,*,#13735,.F.);
#18704=ORIENTED_EDGE('',*,*,#13736,.T.);
#18705=ORIENTED_EDGE('',*,*,#13736,.F.);
#18706=ORIENTED_EDGE('',*,*,#13737,.F.);
#18707=ORIENTED_EDGE('',*,*,#13738,.F.);
#18708=ORIENTED_EDGE('',*,*,#13739,.F.);
#18709=ORIENTED_EDGE('',*,*,#13740,.F.);
#18710=ORIENTED_EDGE('',*,*,#13739,.T.);
#18711=ORIENTED_EDGE('',*,*,#13741,.F.);
#18712=ORIENTED_EDGE('',*,*,#13742,.T.);
#18713=ORIENTED_EDGE('',*,*,#13743,.F.);
#18714=ORIENTED_EDGE('',*,*,#13744,.T.);
#18715=ORIENTED_EDGE('',*,*,#13745,.F.);
#18716=ORIENTED_EDGE('',*,*,#13746,.T.);
#18717=ORIENTED_EDGE('',*,*,#13747,.F.);
#18718=ORIENTED_EDGE('',*,*,#13746,.F.);
#18719=ORIENTED_EDGE('',*,*,#13748,.F.);
#18720=ORIENTED_EDGE('',*,*,#13749,.T.);
#18721=ORIENTED_EDGE('',*,*,#13750,.F.);
#18722=ORIENTED_EDGE('',*,*,#13751,.T.);
#18723=ORIENTED_EDGE('',*,*,#13752,.F.);
#18724=ORIENTED_EDGE('',*,*,#13753,.T.);
#18725=ORIENTED_EDGE('',*,*,#13754,.F.);
#18726=ORIENTED_EDGE('',*,*,#13755,.T.);
#18727=ORIENTED_EDGE('',*,*,#13756,.F.);
#18728=ORIENTED_EDGE('',*,*,#13738,.T.);
#18729=ORIENTED_EDGE('',*,*,#13757,.T.);
#18730=ORIENTED_EDGE('',*,*,#13758,.T.);
#18731=ORIENTED_EDGE('',*,*,#13741,.T.);
#18732=ORIENTED_EDGE('',*,*,#13759,.F.);
#18733=ORIENTED_EDGE('',*,*,#13760,.F.);
#18734=ORIENTED_EDGE('',*,*,#13742,.F.);
#18735=ORIENTED_EDGE('',*,*,#13758,.F.);
#18736=ORIENTED_EDGE('',*,*,#13760,.T.);
#18737=ORIENTED_EDGE('',*,*,#13761,.T.);
#18738=ORIENTED_EDGE('',*,*,#13762,.T.);
#18739=ORIENTED_EDGE('',*,*,#13743,.T.);
#18740=ORIENTED_EDGE('',*,*,#13763,.F.);
#18741=ORIENTED_EDGE('',*,*,#13764,.F.);
#18742=ORIENTED_EDGE('',*,*,#13744,.F.);
#18743=ORIENTED_EDGE('',*,*,#13762,.F.);
#18744=ORIENTED_EDGE('',*,*,#13764,.T.);
#18745=ORIENTED_EDGE('',*,*,#13765,.T.);
#18746=ORIENTED_EDGE('',*,*,#13766,.T.);
#18747=ORIENTED_EDGE('',*,*,#13767,.T.);
#18748=ORIENTED_EDGE('',*,*,#13748,.T.);
#18749=ORIENTED_EDGE('',*,*,#13745,.T.);
#18750=ORIENTED_EDGE('',*,*,#13768,.F.);
#18751=ORIENTED_EDGE('',*,*,#13769,.F.);
#18752=ORIENTED_EDGE('',*,*,#13749,.F.);
#18753=ORIENTED_EDGE('',*,*,#13767,.F.);
#18754=ORIENTED_EDGE('',*,*,#13769,.T.);
#18755=ORIENTED_EDGE('',*,*,#13770,.T.);
#18756=ORIENTED_EDGE('',*,*,#13771,.T.);
#18757=ORIENTED_EDGE('',*,*,#13750,.T.);
#18758=ORIENTED_EDGE('',*,*,#13772,.F.);
#18759=ORIENTED_EDGE('',*,*,#13773,.F.);
#18760=ORIENTED_EDGE('',*,*,#13751,.F.);
#18761=ORIENTED_EDGE('',*,*,#13771,.F.);
#18762=ORIENTED_EDGE('',*,*,#13773,.T.);
#18763=ORIENTED_EDGE('',*,*,#13774,.T.);
#18764=ORIENTED_EDGE('',*,*,#13775,.T.);
#18765=ORIENTED_EDGE('',*,*,#13752,.T.);
#18766=ORIENTED_EDGE('',*,*,#13753,.F.);
#18767=ORIENTED_EDGE('',*,*,#13775,.F.);
#18768=ORIENTED_EDGE('',*,*,#13776,.F.);
#18769=ORIENTED_EDGE('',*,*,#13777,.F.);
#18770=ORIENTED_EDGE('',*,*,#13778,.F.);
#18771=ORIENTED_EDGE('',*,*,#13779,.T.);
#18772=ORIENTED_EDGE('',*,*,#13765,.F.);
#18773=ORIENTED_EDGE('',*,*,#13763,.T.);
#18774=ORIENTED_EDGE('',*,*,#13761,.F.);
#18775=ORIENTED_EDGE('',*,*,#13759,.T.);
#18776=ORIENTED_EDGE('',*,*,#13757,.F.);
#18777=ORIENTED_EDGE('',*,*,#13737,.T.);
#18778=ORIENTED_EDGE('',*,*,#13780,.F.);
#18779=ORIENTED_EDGE('',*,*,#13781,.T.);
#18780=ORIENTED_EDGE('',*,*,#13782,.F.);
#18781=ORIENTED_EDGE('',*,*,#13776,.T.);
#18782=ORIENTED_EDGE('',*,*,#13774,.F.);
#18783=ORIENTED_EDGE('',*,*,#13772,.T.);
#18784=ORIENTED_EDGE('',*,*,#13770,.F.);
#18785=ORIENTED_EDGE('',*,*,#13768,.T.);
#18786=ORIENTED_EDGE('',*,*,#13766,.F.);
#18787=ORIENTED_EDGE('',*,*,#13779,.F.);
#18788=ORIENTED_EDGE('',*,*,#13740,.T.);
#18789=ORIENTED_EDGE('',*,*,#13756,.T.);
#18790=ORIENTED_EDGE('',*,*,#13783,.T.);
#18791=ORIENTED_EDGE('',*,*,#13780,.T.);
#18792=ORIENTED_EDGE('',*,*,#13755,.F.);
#18793=ORIENTED_EDGE('',*,*,#13784,.F.);
#18794=ORIENTED_EDGE('',*,*,#13781,.F.);
#18795=ORIENTED_EDGE('',*,*,#13783,.F.);
#18796=ORIENTED_EDGE('',*,*,#13747,.T.);
#18797=ORIENTED_EDGE('',*,*,#13778,.T.);
#18798=ORIENTED_EDGE('',*,*,#13777,.T.);
#18799=ORIENTED_EDGE('',*,*,#13782,.T.);
#18800=ORIENTED_EDGE('',*,*,#13784,.T.);
#18801=ORIENTED_EDGE('',*,*,#13754,.T.);
#18802=ORIENTED_EDGE('',*,*,#13785,.F.);
#18803=ORIENTED_EDGE('',*,*,#13786,.T.);
#18804=ORIENTED_EDGE('',*,*,#13787,.F.);
#18805=ORIENTED_EDGE('',*,*,#13788,.T.);
#18806=ORIENTED_EDGE('',*,*,#13785,.T.);
#18807=ORIENTED_EDGE('',*,*,#13788,.F.);
#18808=ORIENTED_EDGE('',*,*,#13787,.T.);
#18809=ORIENTED_EDGE('',*,*,#13789,.F.);
#18810=ORIENTED_EDGE('',*,*,#13789,.T.);
#18811=ORIENTED_EDGE('',*,*,#13790,.T.);
#18812=ORIENTED_EDGE('',*,*,#13786,.F.);
#18813=ORIENTED_EDGE('',*,*,#13790,.F.);
#18814=ORIENTED_EDGE('',*,*,#13791,.F.);
#18815=ORIENTED_EDGE('',*,*,#13792,.T.);
#18816=ORIENTED_EDGE('',*,*,#13793,.F.);
#18817=ORIENTED_EDGE('',*,*,#13794,.T.);
#18818=ORIENTED_EDGE('',*,*,#13791,.T.);
#18819=ORIENTED_EDGE('',*,*,#13794,.F.);
#18820=ORIENTED_EDGE('',*,*,#13793,.T.);
#18821=ORIENTED_EDGE('',*,*,#13795,.F.);
#18822=ORIENTED_EDGE('',*,*,#13795,.T.);
#18823=ORIENTED_EDGE('',*,*,#13796,.T.);
#18824=ORIENTED_EDGE('',*,*,#13792,.F.);
#18825=ORIENTED_EDGE('',*,*,#13796,.F.);
#18826=ORIENTED_EDGE('',*,*,#13797,.F.);
#18827=ORIENTED_EDGE('',*,*,#13798,.F.);
#18828=ORIENTED_EDGE('',*,*,#13799,.T.);
#18829=ORIENTED_EDGE('',*,*,#13800,.F.);
#18830=ORIENTED_EDGE('',*,*,#13801,.F.);
#18831=ORIENTED_EDGE('',*,*,#13799,.F.);
#18832=ORIENTED_EDGE('',*,*,#13800,.T.);
#18833=ORIENTED_EDGE('',*,*,#13801,.T.);
#18834=ORIENTED_EDGE('',*,*,#13802,.T.);
#18835=ORIENTED_EDGE('',*,*,#13803,.T.);
#18836=ORIENTED_EDGE('',*,*,#13802,.F.);
#18837=ORIENTED_EDGE('',*,*,#13804,.T.);
#18838=ORIENTED_EDGE('',*,*,#13805,.T.);
#18839=ORIENTED_EDGE('',*,*,#13806,.F.);
#18840=ORIENTED_EDGE('',*,*,#13805,.F.);
#18841=ORIENTED_EDGE('',*,*,#13806,.T.);
#18842=ORIENTED_EDGE('',*,*,#13807,.T.);
#18843=ORIENTED_EDGE('',*,*,#13808,.F.);
#18844=ORIENTED_EDGE('',*,*,#13807,.F.);
#18845=ORIENTED_EDGE('',*,*,#13803,.F.);
#18846=ORIENTED_EDGE('',*,*,#13808,.T.);
#18847=ORIENTED_EDGE('',*,*,#13809,.F.);
#18848=ORIENTED_EDGE('',*,*,#13810,.T.);
#18849=ORIENTED_EDGE('',*,*,#13797,.T.);
#18850=ORIENTED_EDGE('',*,*,#13798,.T.);
#18851=ORIENTED_EDGE('',*,*,#13810,.F.);
#18852=ORIENTED_EDGE('',*,*,#13809,.T.);
#18853=ORIENTED_EDGE('',*,*,#13811,.F.);
#18854=ORIENTED_EDGE('',*,*,#13811,.T.);
#18855=ORIENTED_EDGE('',*,*,#13812,.T.);
#18856=ORIENTED_EDGE('',*,*,#13804,.F.);
#18857=ORIENTED_EDGE('',*,*,#13812,.F.);
#18858=ORIENTED_EDGE('',*,*,#13813,.F.);
#18859=ORIENTED_EDGE('',*,*,#13814,.F.);
#18860=ORIENTED_EDGE('',*,*,#13815,.T.);
#18861=ORIENTED_EDGE('',*,*,#13816,.F.);
#18862=ORIENTED_EDGE('',*,*,#13817,.F.);
#18863=ORIENTED_EDGE('',*,*,#13815,.F.);
#18864=ORIENTED_EDGE('',*,*,#13818,.T.);
#18865=ORIENTED_EDGE('',*,*,#13819,.T.);
#18866=ORIENTED_EDGE('',*,*,#13816,.T.);
#18867=ORIENTED_EDGE('',*,*,#13817,.T.);
#18868=ORIENTED_EDGE('',*,*,#13819,.F.);
#18869=ORIENTED_EDGE('',*,*,#13820,.F.);
#18870=ORIENTED_EDGE('',*,*,#13821,.T.);
#18871=ORIENTED_EDGE('',*,*,#13822,.F.);
#18872=ORIENTED_EDGE('',*,*,#13823,.T.);
#18873=ORIENTED_EDGE('',*,*,#13820,.T.);
#18874=ORIENTED_EDGE('',*,*,#13823,.F.);
#18875=ORIENTED_EDGE('',*,*,#13824,.F.);
#18876=ORIENTED_EDGE('',*,*,#13825,.T.);
#18877=ORIENTED_EDGE('',*,*,#13822,.T.);
#18878=ORIENTED_EDGE('',*,*,#13825,.F.);
#18879=ORIENTED_EDGE('',*,*,#13826,.F.);
#18880=ORIENTED_EDGE('',*,*,#13827,.T.);
#18881=ORIENTED_EDGE('',*,*,#13824,.T.);
#18882=ORIENTED_EDGE('',*,*,#13827,.F.);
#18883=ORIENTED_EDGE('',*,*,#13826,.T.);
#18884=ORIENTED_EDGE('',*,*,#13818,.F.);
#18885=ORIENTED_EDGE('',*,*,#13813,.T.);
#18886=ORIENTED_EDGE('',*,*,#13814,.T.);
#18887=ORIENTED_EDGE('',*,*,#13828,.T.);
#18888=ORIENTED_EDGE('',*,*,#13821,.F.);
#18889=ORIENTED_EDGE('',*,*,#13828,.F.);
#18890=ORIENTED_EDGE('',*,*,#13829,.T.);
#18891=ORIENTED_EDGE('',*,*,#13829,.F.);
#18892=ORIENTED_EDGE('',*,*,#13830,.T.);
#18893=ORIENTED_EDGE('',*,*,#13830,.F.);
#18894=ORIENTED_EDGE('',*,*,#13831,.T.);
#18895=ORIENTED_EDGE('',*,*,#13831,.F.);
#18896=ORIENTED_EDGE('',*,*,#13832,.T.);
#18897=ORIENTED_EDGE('',*,*,#13832,.F.);
#18898=ORIENTED_EDGE('',*,*,#13833,.T.);
#18899=ORIENTED_EDGE('',*,*,#13833,.F.);
#18900=ORIENTED_EDGE('',*,*,#13834,.T.);
#18901=ORIENTED_EDGE('',*,*,#13834,.F.);
#18902=ORIENTED_EDGE('',*,*,#13835,.T.);
#18903=ORIENTED_EDGE('',*,*,#13835,.F.);
#18904=ORIENTED_EDGE('',*,*,#13836,.T.);
#18905=ORIENTED_EDGE('',*,*,#13836,.F.);
#18906=ORIENTED_EDGE('',*,*,#13837,.F.);
#18907=ORIENTED_EDGE('',*,*,#13838,.F.);
#18908=ORIENTED_EDGE('',*,*,#13839,.F.);
#18909=ORIENTED_EDGE('',*,*,#13840,.F.);
#18910=ORIENTED_EDGE('',*,*,#13839,.T.);
#18911=ORIENTED_EDGE('',*,*,#13841,.F.);
#18912=ORIENTED_EDGE('',*,*,#13842,.T.);
#18913=ORIENTED_EDGE('',*,*,#13843,.F.);
#18914=ORIENTED_EDGE('',*,*,#13844,.T.);
#18915=ORIENTED_EDGE('',*,*,#13845,.F.);
#18916=ORIENTED_EDGE('',*,*,#13846,.T.);
#18917=ORIENTED_EDGE('',*,*,#13847,.T.);
#18918=ORIENTED_EDGE('',*,*,#13848,.F.);
#18919=ORIENTED_EDGE('',*,*,#13847,.F.);
#18920=ORIENTED_EDGE('',*,*,#13849,.T.);
#18921=ORIENTED_EDGE('',*,*,#13850,.F.);
#18922=ORIENTED_EDGE('',*,*,#13851,.T.);
#18923=ORIENTED_EDGE('',*,*,#13852,.F.);
#18924=ORIENTED_EDGE('',*,*,#13853,.T.);
#18925=ORIENTED_EDGE('',*,*,#13854,.F.);
#18926=ORIENTED_EDGE('',*,*,#13855,.T.);
#18927=ORIENTED_EDGE('',*,*,#13856,.F.);
#18928=ORIENTED_EDGE('',*,*,#13857,.T.);
#18929=ORIENTED_EDGE('',*,*,#13858,.F.);
#18930=ORIENTED_EDGE('',*,*,#13838,.T.);
#18931=ORIENTED_EDGE('',*,*,#13859,.T.);
#18932=ORIENTED_EDGE('',*,*,#13860,.T.);
#18933=ORIENTED_EDGE('',*,*,#13841,.T.);
#18934=ORIENTED_EDGE('',*,*,#13861,.F.);
#18935=ORIENTED_EDGE('',*,*,#13862,.F.);
#18936=ORIENTED_EDGE('',*,*,#13842,.F.);
#18937=ORIENTED_EDGE('',*,*,#13860,.F.);
#18938=ORIENTED_EDGE('',*,*,#13862,.T.);
#18939=ORIENTED_EDGE('',*,*,#13863,.T.);
#18940=ORIENTED_EDGE('',*,*,#13864,.T.);
#18941=ORIENTED_EDGE('',*,*,#13843,.T.);
#18942=ORIENTED_EDGE('',*,*,#13865,.F.);
#18943=ORIENTED_EDGE('',*,*,#13866,.F.);
#18944=ORIENTED_EDGE('',*,*,#13844,.F.);
#18945=ORIENTED_EDGE('',*,*,#13864,.F.);
#18946=ORIENTED_EDGE('',*,*,#13866,.T.);
#18947=ORIENTED_EDGE('',*,*,#13867,.T.);
#18948=ORIENTED_EDGE('',*,*,#13868,.T.);
#18949=ORIENTED_EDGE('',*,*,#13845,.T.);
#18950=ORIENTED_EDGE('',*,*,#13869,.F.);
#18951=ORIENTED_EDGE('',*,*,#13870,.F.);
#18952=ORIENTED_EDGE('',*,*,#13849,.F.);
#18953=ORIENTED_EDGE('',*,*,#13846,.F.);
#18954=ORIENTED_EDGE('',*,*,#13868,.F.);
#18955=ORIENTED_EDGE('',*,*,#13871,.F.);
#18956=ORIENTED_EDGE('',*,*,#13870,.T.);
#18957=ORIENTED_EDGE('',*,*,#13872,.T.);
#18958=ORIENTED_EDGE('',*,*,#13873,.T.);
#18959=ORIENTED_EDGE('',*,*,#13850,.T.);
#18960=ORIENTED_EDGE('',*,*,#13874,.F.);
#18961=ORIENTED_EDGE('',*,*,#13875,.F.);
#18962=ORIENTED_EDGE('',*,*,#13851,.F.);
#18963=ORIENTED_EDGE('',*,*,#13873,.F.);
#18964=ORIENTED_EDGE('',*,*,#13875,.T.);
#18965=ORIENTED_EDGE('',*,*,#13876,.T.);
#18966=ORIENTED_EDGE('',*,*,#13877,.T.);
#18967=ORIENTED_EDGE('',*,*,#13852,.T.);
#18968=ORIENTED_EDGE('',*,*,#13878,.F.);
#18969=ORIENTED_EDGE('',*,*,#13879,.F.);
#18970=ORIENTED_EDGE('',*,*,#13853,.F.);
#18971=ORIENTED_EDGE('',*,*,#13877,.F.);
#18972=ORIENTED_EDGE('',*,*,#13879,.T.);
#18973=ORIENTED_EDGE('',*,*,#13880,.T.);
#18974=ORIENTED_EDGE('',*,*,#13881,.T.);
#18975=ORIENTED_EDGE('',*,*,#13854,.T.);
#18976=ORIENTED_EDGE('',*,*,#13855,.F.);
#18977=ORIENTED_EDGE('',*,*,#13881,.F.);
#18978=ORIENTED_EDGE('',*,*,#13882,.F.);
#18979=ORIENTED_EDGE('',*,*,#13883,.F.);
#18980=ORIENTED_EDGE('',*,*,#13884,.F.);
#18981=ORIENTED_EDGE('',*,*,#13885,.T.);
#18982=ORIENTED_EDGE('',*,*,#13871,.T.);
#18983=ORIENTED_EDGE('',*,*,#13867,.F.);
#18984=ORIENTED_EDGE('',*,*,#13865,.T.);
#18985=ORIENTED_EDGE('',*,*,#13863,.F.);
#18986=ORIENTED_EDGE('',*,*,#13861,.T.);
#18987=ORIENTED_EDGE('',*,*,#13859,.F.);
#18988=ORIENTED_EDGE('',*,*,#13837,.T.);
#18989=ORIENTED_EDGE('',*,*,#13886,.F.);
#18990=ORIENTED_EDGE('',*,*,#13887,.T.);
#18991=ORIENTED_EDGE('',*,*,#13888,.F.);
#18992=ORIENTED_EDGE('',*,*,#13882,.T.);
#18993=ORIENTED_EDGE('',*,*,#13880,.F.);
#18994=ORIENTED_EDGE('',*,*,#13878,.T.);
#18995=ORIENTED_EDGE('',*,*,#13876,.F.);
#18996=ORIENTED_EDGE('',*,*,#13874,.T.);
#18997=ORIENTED_EDGE('',*,*,#13872,.F.);
#18998=ORIENTED_EDGE('',*,*,#13869,.T.);
#18999=ORIENTED_EDGE('',*,*,#13885,.F.);
#19000=ORIENTED_EDGE('',*,*,#13840,.T.);
#19001=ORIENTED_EDGE('',*,*,#13858,.T.);
#19002=ORIENTED_EDGE('',*,*,#13889,.T.);
#19003=ORIENTED_EDGE('',*,*,#13886,.T.);
#19004=ORIENTED_EDGE('',*,*,#13857,.F.);
#19005=ORIENTED_EDGE('',*,*,#13890,.F.);
#19006=ORIENTED_EDGE('',*,*,#13887,.F.);
#19007=ORIENTED_EDGE('',*,*,#13889,.F.);
#19008=ORIENTED_EDGE('',*,*,#13848,.T.);
#19009=ORIENTED_EDGE('',*,*,#13884,.T.);
#19010=ORIENTED_EDGE('',*,*,#13883,.T.);
#19011=ORIENTED_EDGE('',*,*,#13888,.T.);
#19012=ORIENTED_EDGE('',*,*,#13890,.T.);
#19013=ORIENTED_EDGE('',*,*,#13856,.T.);
#19014=ORIENTED_EDGE('',*,*,#13891,.F.);
#19015=ORIENTED_EDGE('',*,*,#13892,.T.);
#19016=ORIENTED_EDGE('',*,*,#13893,.F.);
#19017=ORIENTED_EDGE('',*,*,#13894,.T.);
#19018=ORIENTED_EDGE('',*,*,#13891,.T.);
#19019=ORIENTED_EDGE('',*,*,#13894,.F.);
#19020=ORIENTED_EDGE('',*,*,#13893,.T.);
#19021=ORIENTED_EDGE('',*,*,#13895,.F.);
#19022=ORIENTED_EDGE('',*,*,#13895,.T.);
#19023=ORIENTED_EDGE('',*,*,#13896,.T.);
#19024=ORIENTED_EDGE('',*,*,#13892,.F.);
#19025=ORIENTED_EDGE('',*,*,#13896,.F.);
#19026=ORIENTED_EDGE('',*,*,#13897,.F.);
#19027=ORIENTED_EDGE('',*,*,#13898,.T.);
#19028=ORIENTED_EDGE('',*,*,#13899,.F.);
#19029=ORIENTED_EDGE('',*,*,#13900,.T.);
#19030=ORIENTED_EDGE('',*,*,#13897,.T.);
#19031=ORIENTED_EDGE('',*,*,#13900,.F.);
#19032=ORIENTED_EDGE('',*,*,#13899,.T.);
#19033=ORIENTED_EDGE('',*,*,#13901,.F.);
#19034=ORIENTED_EDGE('',*,*,#13901,.T.);
#19035=ORIENTED_EDGE('',*,*,#13902,.T.);
#19036=ORIENTED_EDGE('',*,*,#13898,.F.);
#19037=ORIENTED_EDGE('',*,*,#13902,.F.);
#19038=ORIENTED_EDGE('',*,*,#13903,.T.);
#19039=ORIENTED_EDGE('',*,*,#13904,.T.);
#19040=ORIENTED_EDGE('',*,*,#13905,.T.);
#19041=ORIENTED_EDGE('',*,*,#13906,.F.);
#19042=ORIENTED_EDGE('',*,*,#13907,.T.);
#19043=ORIENTED_EDGE('',*,*,#13908,.T.);
#19044=ORIENTED_EDGE('',*,*,#13909,.T.);
#19045=ORIENTED_EDGE('',*,*,#13904,.F.);
#19046=ORIENTED_EDGE('',*,*,#13910,.T.);
#19047=ORIENTED_EDGE('',*,*,#13911,.T.);
#19048=ORIENTED_EDGE('',*,*,#13912,.T.);
#19049=ORIENTED_EDGE('',*,*,#13908,.F.);
#19050=ORIENTED_EDGE('',*,*,#13913,.T.);
#19051=ORIENTED_EDGE('',*,*,#13914,.T.);
#19052=ORIENTED_EDGE('',*,*,#13915,.T.);
#19053=ORIENTED_EDGE('',*,*,#13911,.F.);
#19054=ORIENTED_EDGE('',*,*,#13916,.T.);
#19055=ORIENTED_EDGE('',*,*,#13917,.T.);
#19056=ORIENTED_EDGE('',*,*,#13918,.T.);
#19057=ORIENTED_EDGE('',*,*,#13914,.F.);
#19058=ORIENTED_EDGE('',*,*,#13919,.T.);
#19059=ORIENTED_EDGE('',*,*,#13906,.T.);
#19060=ORIENTED_EDGE('',*,*,#13920,.T.);
#19061=ORIENTED_EDGE('',*,*,#13917,.F.);
#19062=ORIENTED_EDGE('',*,*,#13919,.F.);
#19063=ORIENTED_EDGE('',*,*,#13916,.F.);
#19064=ORIENTED_EDGE('',*,*,#13913,.F.);
#19065=ORIENTED_EDGE('',*,*,#13910,.F.);
#19066=ORIENTED_EDGE('',*,*,#13907,.F.);
#19067=ORIENTED_EDGE('',*,*,#13903,.F.);
#19068=ORIENTED_EDGE('',*,*,#13920,.F.);
#19069=ORIENTED_EDGE('',*,*,#13905,.F.);
#19070=ORIENTED_EDGE('',*,*,#13909,.F.);
#19071=ORIENTED_EDGE('',*,*,#13912,.F.);
#19072=ORIENTED_EDGE('',*,*,#13915,.F.);
#19073=ORIENTED_EDGE('',*,*,#13918,.F.);
#19074=ORIENTED_EDGE('',*,*,#13921,.F.);
#19075=ORIENTED_EDGE('',*,*,#13922,.F.);
#19076=ORIENTED_EDGE('',*,*,#13923,.F.);
#19077=ORIENTED_EDGE('',*,*,#13924,.T.);
#19078=ORIENTED_EDGE('',*,*,#13922,.T.);
#19079=ORIENTED_EDGE('',*,*,#13924,.F.);
#19080=ORIENTED_EDGE('',*,*,#13925,.F.);
#19081=ORIENTED_EDGE('',*,*,#13926,.T.);
#19082=ORIENTED_EDGE('',*,*,#13923,.T.);
#19083=ORIENTED_EDGE('',*,*,#13926,.F.);
#19084=ORIENTED_EDGE('',*,*,#13927,.F.);
#19085=ORIENTED_EDGE('',*,*,#13928,.T.);
#19086=ORIENTED_EDGE('',*,*,#13925,.T.);
#19087=ORIENTED_EDGE('',*,*,#13928,.F.);
#19088=ORIENTED_EDGE('',*,*,#13927,.T.);
#19089=ORIENTED_EDGE('',*,*,#13929,.F.);
#19090=ORIENTED_EDGE('',*,*,#13930,.F.);
#19091=ORIENTED_EDGE('',*,*,#13931,.T.);
#19092=ORIENTED_EDGE('',*,*,#13929,.T.);
#19093=ORIENTED_EDGE('',*,*,#13931,.F.);
#19094=ORIENTED_EDGE('',*,*,#13921,.T.);
#19095=ORIENTED_EDGE('',*,*,#13932,.T.);
#19096=ORIENTED_EDGE('',*,*,#13930,.T.);
#19097=ORIENTED_EDGE('',*,*,#13932,.F.);
#19098=ORIENTED_EDGE('',*,*,#13933,.F.);
#19099=ORIENTED_EDGE('',*,*,#13934,.T.);
#19100=ORIENTED_EDGE('',*,*,#13935,.F.);
#19101=ORIENTED_EDGE('',*,*,#13934,.F.);
#19102=ORIENTED_EDGE('',*,*,#13936,.F.);
#19103=ORIENTED_EDGE('',*,*,#13937,.T.);
#19104=ORIENTED_EDGE('',*,*,#13938,.F.);
#19105=ORIENTED_EDGE('',*,*,#13937,.F.);
#19106=ORIENTED_EDGE('',*,*,#13939,.F.);
#19107=ORIENTED_EDGE('',*,*,#13940,.T.);
#19108=ORIENTED_EDGE('',*,*,#13941,.F.);
#19109=ORIENTED_EDGE('',*,*,#13940,.F.);
#19110=ORIENTED_EDGE('',*,*,#13942,.F.);
#19111=ORIENTED_EDGE('',*,*,#13943,.T.);
#19112=ORIENTED_EDGE('',*,*,#13944,.F.);
#19113=ORIENTED_EDGE('',*,*,#13943,.F.);
#19114=ORIENTED_EDGE('',*,*,#13945,.T.);
#19115=ORIENTED_EDGE('',*,*,#13946,.T.);
#19116=ORIENTED_EDGE('',*,*,#13947,.F.);
#19117=ORIENTED_EDGE('',*,*,#13948,.F.);
#19118=ORIENTED_EDGE('',*,*,#13949,.T.);
#19119=ORIENTED_EDGE('',*,*,#13948,.T.);
#19120=ORIENTED_EDGE('',*,*,#13950,.F.);
#19121=ORIENTED_EDGE('',*,*,#13951,.F.);
#19122=ORIENTED_EDGE('',*,*,#13952,.T.);
#19123=ORIENTED_EDGE('',*,*,#13951,.T.);
#19124=ORIENTED_EDGE('',*,*,#13953,.F.);
#19125=ORIENTED_EDGE('',*,*,#13954,.F.);
#19126=ORIENTED_EDGE('',*,*,#13955,.T.);
#19127=ORIENTED_EDGE('',*,*,#13954,.T.);
#19128=ORIENTED_EDGE('',*,*,#13956,.F.);
#19129=ORIENTED_EDGE('',*,*,#13946,.F.);
#19130=ORIENTED_EDGE('',*,*,#13956,.T.);
#19131=ORIENTED_EDGE('',*,*,#13953,.T.);
#19132=ORIENTED_EDGE('',*,*,#13950,.T.);
#19133=ORIENTED_EDGE('',*,*,#13947,.T.);
#19134=ORIENTED_EDGE('',*,*,#13935,.T.);
#19135=ORIENTED_EDGE('',*,*,#13938,.T.);
#19136=ORIENTED_EDGE('',*,*,#13941,.T.);
#19137=ORIENTED_EDGE('',*,*,#13944,.T.);
#19138=ORIENTED_EDGE('',*,*,#13955,.F.);
#19139=ORIENTED_EDGE('',*,*,#13945,.F.);
#19140=ORIENTED_EDGE('',*,*,#13949,.F.);
#19141=ORIENTED_EDGE('',*,*,#13952,.F.);
#19142=ORIENTED_EDGE('',*,*,#13933,.T.);
#19143=ORIENTED_EDGE('',*,*,#13936,.T.);
#19144=ORIENTED_EDGE('',*,*,#13939,.T.);
#19145=ORIENTED_EDGE('',*,*,#13942,.T.);
#19146=ORIENTED_EDGE('',*,*,#13957,.F.);
#19147=ORIENTED_EDGE('',*,*,#13958,.T.);
#19148=ORIENTED_EDGE('',*,*,#13959,.F.);
#19149=ORIENTED_EDGE('',*,*,#13958,.F.);
#19150=ORIENTED_EDGE('',*,*,#13960,.F.);
#19151=ORIENTED_EDGE('',*,*,#13961,.T.);
#19152=ORIENTED_EDGE('',*,*,#13962,.F.);
#19153=ORIENTED_EDGE('',*,*,#13961,.F.);
#19154=ORIENTED_EDGE('',*,*,#13963,.F.);
#19155=ORIENTED_EDGE('',*,*,#13964,.T.);
#19156=ORIENTED_EDGE('',*,*,#13965,.F.);
#19157=ORIENTED_EDGE('',*,*,#13964,.F.);
#19158=ORIENTED_EDGE('',*,*,#13966,.F.);
#19159=ORIENTED_EDGE('',*,*,#13967,.T.);
#19160=ORIENTED_EDGE('',*,*,#13968,.F.);
#19161=ORIENTED_EDGE('',*,*,#13967,.F.);
#19162=ORIENTED_EDGE('',*,*,#13969,.F.);
#19163=ORIENTED_EDGE('',*,*,#13970,.T.);
#19164=ORIENTED_EDGE('',*,*,#13971,.F.);
#19165=ORIENTED_EDGE('',*,*,#13970,.F.);
#19166=ORIENTED_EDGE('',*,*,#13972,.F.);
#19167=ORIENTED_EDGE('',*,*,#13973,.T.);
#19168=ORIENTED_EDGE('',*,*,#13974,.F.);
#19169=ORIENTED_EDGE('',*,*,#13973,.F.);
#19170=ORIENTED_EDGE('',*,*,#13975,.F.);
#19171=ORIENTED_EDGE('',*,*,#13976,.T.);
#19172=ORIENTED_EDGE('',*,*,#13977,.F.);
#19173=ORIENTED_EDGE('',*,*,#13976,.F.);
#19174=ORIENTED_EDGE('',*,*,#13978,.F.);
#19175=ORIENTED_EDGE('',*,*,#13979,.T.);
#19176=ORIENTED_EDGE('',*,*,#13980,.F.);
#19177=ORIENTED_EDGE('',*,*,#13979,.F.);
#19178=ORIENTED_EDGE('',*,*,#13981,.T.);
#19179=ORIENTED_EDGE('',*,*,#13982,.T.);
#19180=ORIENTED_EDGE('',*,*,#13983,.F.);
#19181=ORIENTED_EDGE('',*,*,#13984,.F.);
#19182=ORIENTED_EDGE('',*,*,#13985,.T.);
#19183=ORIENTED_EDGE('',*,*,#13984,.T.);
#19184=ORIENTED_EDGE('',*,*,#13986,.F.);
#19185=ORIENTED_EDGE('',*,*,#13987,.F.);
#19186=ORIENTED_EDGE('',*,*,#13988,.T.);
#19187=ORIENTED_EDGE('',*,*,#13987,.T.);
#19188=ORIENTED_EDGE('',*,*,#13989,.F.);
#19189=ORIENTED_EDGE('',*,*,#13990,.F.);
#19190=ORIENTED_EDGE('',*,*,#13991,.T.);
#19191=ORIENTED_EDGE('',*,*,#13990,.T.);
#19192=ORIENTED_EDGE('',*,*,#13992,.F.);
#19193=ORIENTED_EDGE('',*,*,#13982,.F.);
#19194=ORIENTED_EDGE('',*,*,#13992,.T.);
#19195=ORIENTED_EDGE('',*,*,#13989,.T.);
#19196=ORIENTED_EDGE('',*,*,#13986,.T.);
#19197=ORIENTED_EDGE('',*,*,#13983,.T.);
#19198=ORIENTED_EDGE('',*,*,#13980,.T.);
#19199=ORIENTED_EDGE('',*,*,#13977,.T.);
#19200=ORIENTED_EDGE('',*,*,#13974,.T.);
#19201=ORIENTED_EDGE('',*,*,#13971,.T.);
#19202=ORIENTED_EDGE('',*,*,#13968,.T.);
#19203=ORIENTED_EDGE('',*,*,#13965,.T.);
#19204=ORIENTED_EDGE('',*,*,#13962,.T.);
#19205=ORIENTED_EDGE('',*,*,#13959,.T.);
#19206=ORIENTED_EDGE('',*,*,#13991,.F.);
#19207=ORIENTED_EDGE('',*,*,#13981,.F.);
#19208=ORIENTED_EDGE('',*,*,#13985,.F.);
#19209=ORIENTED_EDGE('',*,*,#13988,.F.);
#19210=ORIENTED_EDGE('',*,*,#13978,.T.);
#19211=ORIENTED_EDGE('',*,*,#13975,.T.);
#19212=ORIENTED_EDGE('',*,*,#13972,.T.);
#19213=ORIENTED_EDGE('',*,*,#13969,.T.);
#19214=ORIENTED_EDGE('',*,*,#13966,.T.);
#19215=ORIENTED_EDGE('',*,*,#13963,.T.);
#19216=ORIENTED_EDGE('',*,*,#13960,.T.);
#19217=ORIENTED_EDGE('',*,*,#13957,.T.);
#19218=ORIENTED_EDGE('',*,*,#13993,.F.);
#19219=ORIENTED_EDGE('',*,*,#13994,.T.);
#19220=ORIENTED_EDGE('',*,*,#13995,.F.);
#19221=ORIENTED_EDGE('',*,*,#13994,.F.);
#19222=ORIENTED_EDGE('',*,*,#13993,.T.);
#19223=ORIENTED_EDGE('',*,*,#13996,.F.);
#19224=ORIENTED_EDGE('',*,*,#13997,.T.);
#19225=ORIENTED_EDGE('',*,*,#13998,.F.);
#19226=ORIENTED_EDGE('',*,*,#13997,.F.);
#19227=ORIENTED_EDGE('',*,*,#13996,.T.);
#19228=ORIENTED_EDGE('',*,*,#13999,.F.);
#19229=ORIENTED_EDGE('',*,*,#14000,.T.);
#19230=ORIENTED_EDGE('',*,*,#14001,.F.);
#19231=ORIENTED_EDGE('',*,*,#14000,.F.);
#19232=ORIENTED_EDGE('',*,*,#13999,.T.);
#19233=ORIENTED_EDGE('',*,*,#14002,.F.);
#19234=ORIENTED_EDGE('',*,*,#14003,.T.);
#19235=ORIENTED_EDGE('',*,*,#14004,.F.);
#19236=ORIENTED_EDGE('',*,*,#14003,.F.);
#19237=ORIENTED_EDGE('',*,*,#14002,.T.);
#19238=ORIENTED_EDGE('',*,*,#14005,.F.);
#19239=ORIENTED_EDGE('',*,*,#14006,.T.);
#19240=ORIENTED_EDGE('',*,*,#14007,.F.);
#19241=ORIENTED_EDGE('',*,*,#14006,.F.);
#19242=ORIENTED_EDGE('',*,*,#14005,.T.);
#19243=ORIENTED_EDGE('',*,*,#14008,.F.);
#19244=ORIENTED_EDGE('',*,*,#14009,.T.);
#19245=ORIENTED_EDGE('',*,*,#14010,.F.);
#19246=ORIENTED_EDGE('',*,*,#14009,.F.);
#19247=ORIENTED_EDGE('',*,*,#14008,.T.);
#19248=ORIENTED_EDGE('',*,*,#14011,.F.);
#19249=ORIENTED_EDGE('',*,*,#14012,.T.);
#19250=ORIENTED_EDGE('',*,*,#14013,.F.);
#19251=ORIENTED_EDGE('',*,*,#14012,.F.);
#19252=ORIENTED_EDGE('',*,*,#14011,.T.);
#19253=ORIENTED_EDGE('',*,*,#14014,.F.);
#19254=ORIENTED_EDGE('',*,*,#14015,.T.);
#19255=ORIENTED_EDGE('',*,*,#14016,.F.);
#19256=ORIENTED_EDGE('',*,*,#14015,.F.);
#19257=ORIENTED_EDGE('',*,*,#14017,.T.);
#19258=ORIENTED_EDGE('',*,*,#14018,.T.);
#19259=ORIENTED_EDGE('',*,*,#14019,.F.);
#19260=ORIENTED_EDGE('',*,*,#14020,.F.);
#19261=ORIENTED_EDGE('',*,*,#14021,.T.);
#19262=ORIENTED_EDGE('',*,*,#14020,.T.);
#19263=ORIENTED_EDGE('',*,*,#14022,.F.);
#19264=ORIENTED_EDGE('',*,*,#14023,.F.);
#19265=ORIENTED_EDGE('',*,*,#14007,.T.);
#19266=ORIENTED_EDGE('',*,*,#14010,.T.);
#19267=ORIENTED_EDGE('',*,*,#14013,.T.);
#19268=ORIENTED_EDGE('',*,*,#14016,.T.);
#19269=ORIENTED_EDGE('',*,*,#14024,.T.);
#19270=ORIENTED_EDGE('',*,*,#14023,.T.);
#19271=ORIENTED_EDGE('',*,*,#14025,.F.);
#19272=ORIENTED_EDGE('',*,*,#14026,.F.);
#19273=ORIENTED_EDGE('',*,*,#14027,.T.);
#19274=ORIENTED_EDGE('',*,*,#14026,.T.);
#19275=ORIENTED_EDGE('',*,*,#14028,.F.);
#19276=ORIENTED_EDGE('',*,*,#14018,.F.);
#19277=ORIENTED_EDGE('',*,*,#14014,.T.);
#19278=ORIENTED_EDGE('',*,*,#14028,.T.);
#19279=ORIENTED_EDGE('',*,*,#14025,.T.);
#19280=ORIENTED_EDGE('',*,*,#14022,.T.);
#19281=ORIENTED_EDGE('',*,*,#14019,.T.);
#19282=ORIENTED_EDGE('',*,*,#13995,.T.);
#19283=ORIENTED_EDGE('',*,*,#13998,.T.);
#19284=ORIENTED_EDGE('',*,*,#14001,.T.);
#19285=ORIENTED_EDGE('',*,*,#14004,.T.);
#19286=ORIENTED_EDGE('',*,*,#14027,.F.);
#19287=ORIENTED_EDGE('',*,*,#14017,.F.);
#19288=ORIENTED_EDGE('',*,*,#14021,.F.);
#19289=ORIENTED_EDGE('',*,*,#14024,.F.);
#19290=ORIENTED_EDGE('',*,*,#14029,.F.);
#19291=ORIENTED_EDGE('',*,*,#14030,.T.);
#19292=ORIENTED_EDGE('',*,*,#14031,.F.);
#19293=ORIENTED_EDGE('',*,*,#14032,.F.);
#19294=ORIENTED_EDGE('',*,*,#14033,.T.);
#19295=ORIENTED_EDGE('',*,*,#14034,.F.);
#19296=ORIENTED_EDGE('',*,*,#14033,.F.);
#19297=ORIENTED_EDGE('',*,*,#14035,.F.);
#19298=ORIENTED_EDGE('',*,*,#14036,.F.);
#19299=ORIENTED_EDGE('',*,*,#14030,.F.);
#19300=ORIENTED_EDGE('',*,*,#14037,.F.);
#19301=ORIENTED_EDGE('',*,*,#14038,.T.);
#19302=ORIENTED_EDGE('',*,*,#14039,.F.);
#19303=ORIENTED_EDGE('',*,*,#14040,.F.);
#19304=ORIENTED_EDGE('',*,*,#14041,.T.);
#19305=ORIENTED_EDGE('',*,*,#14042,.F.);
#19306=ORIENTED_EDGE('',*,*,#14041,.F.);
#19307=ORIENTED_EDGE('',*,*,#14043,.F.);
#19308=ORIENTED_EDGE('',*,*,#14044,.F.);
#19309=ORIENTED_EDGE('',*,*,#14038,.F.);
#19310=ORIENTED_EDGE('',*,*,#14045,.F.);
#19311=ORIENTED_EDGE('',*,*,#14046,.T.);
#19312=ORIENTED_EDGE('',*,*,#14047,.F.);
#19313=ORIENTED_EDGE('',*,*,#14048,.F.);
#19314=ORIENTED_EDGE('',*,*,#14049,.T.);
#19315=ORIENTED_EDGE('',*,*,#14050,.F.);
#19316=ORIENTED_EDGE('',*,*,#14049,.F.);
#19317=ORIENTED_EDGE('',*,*,#14051,.F.);
#19318=ORIENTED_EDGE('',*,*,#14052,.F.);
#19319=ORIENTED_EDGE('',*,*,#14046,.F.);
#19320=ORIENTED_EDGE('',*,*,#14053,.F.);
#19321=ORIENTED_EDGE('',*,*,#14054,.T.);
#19322=ORIENTED_EDGE('',*,*,#14055,.F.);
#19323=ORIENTED_EDGE('',*,*,#14056,.F.);
#19324=ORIENTED_EDGE('',*,*,#14057,.T.);
#19325=ORIENTED_EDGE('',*,*,#14058,.F.);
#19326=ORIENTED_EDGE('',*,*,#14057,.F.);
#19327=ORIENTED_EDGE('',*,*,#14059,.F.);
#19328=ORIENTED_EDGE('',*,*,#14060,.F.);
#19329=ORIENTED_EDGE('',*,*,#14054,.F.);
#19330=ORIENTED_EDGE('',*,*,#14031,.T.);
#19331=ORIENTED_EDGE('',*,*,#14029,.T.);
#19332=ORIENTED_EDGE('',*,*,#14036,.T.);
#19333=ORIENTED_EDGE('',*,*,#14061,.T.);
#19334=ORIENTED_EDGE('',*,*,#14047,.T.);
#19335=ORIENTED_EDGE('',*,*,#14045,.T.);
#19336=ORIENTED_EDGE('',*,*,#14052,.T.);
#19337=ORIENTED_EDGE('',*,*,#14062,.T.);
#19338=ORIENTED_EDGE('',*,*,#14063,.F.);
#19339=ORIENTED_EDGE('',*,*,#14064,.T.);
#19340=ORIENTED_EDGE('',*,*,#14065,.F.);
#19341=ORIENTED_EDGE('',*,*,#14066,.T.);
#19342=ORIENTED_EDGE('',*,*,#14039,.T.);
#19343=ORIENTED_EDGE('',*,*,#14037,.T.);
#19344=ORIENTED_EDGE('',*,*,#14044,.T.);
#19345=ORIENTED_EDGE('',*,*,#14067,.T.);
#19346=ORIENTED_EDGE('',*,*,#14055,.T.);
#19347=ORIENTED_EDGE('',*,*,#14053,.T.);
#19348=ORIENTED_EDGE('',*,*,#14060,.T.);
#19349=ORIENTED_EDGE('',*,*,#14068,.T.);
#19350=ORIENTED_EDGE('',*,*,#14069,.F.);
#19351=ORIENTED_EDGE('',*,*,#14070,.F.);
#19352=ORIENTED_EDGE('',*,*,#14071,.F.);
#19353=ORIENTED_EDGE('',*,*,#14072,.T.);
#19354=ORIENTED_EDGE('',*,*,#14063,.T.);
#19355=ORIENTED_EDGE('',*,*,#14073,.T.);
#19356=ORIENTED_EDGE('',*,*,#14074,.T.);
#19357=ORIENTED_EDGE('',*,*,#14075,.T.);
#19358=ORIENTED_EDGE('',*,*,#14076,.T.);
#19359=ORIENTED_EDGE('',*,*,#14077,.T.);
#19360=ORIENTED_EDGE('',*,*,#14071,.T.);
#19361=ORIENTED_EDGE('',*,*,#14078,.T.);
#19362=ORIENTED_EDGE('',*,*,#14079,.T.);
#19363=ORIENTED_EDGE('',*,*,#14080,.T.);
#19364=ORIENTED_EDGE('',*,*,#14081,.T.);
#19365=ORIENTED_EDGE('',*,*,#14082,.T.);
#19366=ORIENTED_EDGE('',*,*,#14035,.T.);
#19367=ORIENTED_EDGE('',*,*,#14032,.T.);
#19368=ORIENTED_EDGE('',*,*,#14066,.F.);
#19369=ORIENTED_EDGE('',*,*,#14083,.F.);
#19370=ORIENTED_EDGE('',*,*,#14084,.F.);
#19371=ORIENTED_EDGE('',*,*,#14073,.F.);
#19372=ORIENTED_EDGE('',*,*,#14062,.F.);
#19373=ORIENTED_EDGE('',*,*,#14051,.T.);
#19374=ORIENTED_EDGE('',*,*,#14048,.T.);
#19375=ORIENTED_EDGE('',*,*,#14061,.F.);
#19376=ORIENTED_EDGE('',*,*,#14084,.T.);
#19377=ORIENTED_EDGE('',*,*,#14085,.F.);
#19378=ORIENTED_EDGE('',*,*,#14086,.F.);
#19379=ORIENTED_EDGE('',*,*,#14074,.F.);
#19380=ORIENTED_EDGE('',*,*,#14086,.T.);
#19381=ORIENTED_EDGE('',*,*,#14087,.F.);
#19382=ORIENTED_EDGE('',*,*,#14088,.F.);
#19383=ORIENTED_EDGE('',*,*,#14075,.F.);
#19384=ORIENTED_EDGE('',*,*,#14034,.T.);
#19385=ORIENTED_EDGE('',*,*,#14042,.T.);
#19386=ORIENTED_EDGE('',*,*,#14050,.T.);
#19387=ORIENTED_EDGE('',*,*,#14058,.T.);
#19388=ORIENTED_EDGE('',*,*,#14088,.T.);
#19389=ORIENTED_EDGE('',*,*,#14089,.F.);
#19390=ORIENTED_EDGE('',*,*,#14090,.F.);
#19391=ORIENTED_EDGE('',*,*,#14076,.F.);
#19392=ORIENTED_EDGE('',*,*,#14043,.T.);
#19393=ORIENTED_EDGE('',*,*,#14040,.T.);
#19394=ORIENTED_EDGE('',*,*,#14072,.F.);
#19395=ORIENTED_EDGE('',*,*,#14077,.F.);
#19396=ORIENTED_EDGE('',*,*,#14090,.T.);
#19397=ORIENTED_EDGE('',*,*,#14091,.F.);
#19398=ORIENTED_EDGE('',*,*,#14068,.F.);
#19399=ORIENTED_EDGE('',*,*,#14059,.T.);
#19400=ORIENTED_EDGE('',*,*,#14056,.T.);
#19401=ORIENTED_EDGE('',*,*,#14067,.F.);
#19402=ORIENTED_EDGE('',*,*,#14070,.T.);
#19403=ORIENTED_EDGE('',*,*,#14092,.F.);
#19404=ORIENTED_EDGE('',*,*,#14093,.F.);
#19405=ORIENTED_EDGE('',*,*,#14078,.F.);
#19406=ORIENTED_EDGE('',*,*,#14093,.T.);
#19407=ORIENTED_EDGE('',*,*,#14094,.F.);
#19408=ORIENTED_EDGE('',*,*,#14095,.F.);
#19409=ORIENTED_EDGE('',*,*,#14079,.F.);
#19410=ORIENTED_EDGE('',*,*,#14095,.T.);
#19411=ORIENTED_EDGE('',*,*,#14096,.F.);
#19412=ORIENTED_EDGE('',*,*,#14097,.F.);
#19413=ORIENTED_EDGE('',*,*,#14080,.F.);
#19414=ORIENTED_EDGE('',*,*,#14097,.T.);
#19415=ORIENTED_EDGE('',*,*,#14098,.F.);
#19416=ORIENTED_EDGE('',*,*,#14099,.F.);
#19417=ORIENTED_EDGE('',*,*,#14081,.F.);
#19418=ORIENTED_EDGE('',*,*,#14099,.T.);
#19419=ORIENTED_EDGE('',*,*,#14100,.F.);
#19420=ORIENTED_EDGE('',*,*,#14064,.F.);
#19421=ORIENTED_EDGE('',*,*,#14082,.F.);
#19422=ORIENTED_EDGE('',*,*,#14065,.T.);
#19423=ORIENTED_EDGE('',*,*,#14100,.T.);
#19424=ORIENTED_EDGE('',*,*,#14098,.T.);
#19425=ORIENTED_EDGE('',*,*,#14096,.T.);
#19426=ORIENTED_EDGE('',*,*,#14094,.T.);
#19427=ORIENTED_EDGE('',*,*,#14092,.T.);
#19428=ORIENTED_EDGE('',*,*,#14069,.T.);
#19429=ORIENTED_EDGE('',*,*,#14091,.T.);
#19430=ORIENTED_EDGE('',*,*,#14089,.T.);
#19431=ORIENTED_EDGE('',*,*,#14087,.T.);
#19432=ORIENTED_EDGE('',*,*,#14085,.T.);
#19433=ORIENTED_EDGE('',*,*,#14083,.T.);
#19434=ORIENTED_EDGE('',*,*,#14101,.T.);
#19435=ORIENTED_EDGE('',*,*,#14102,.T.);
#19436=ORIENTED_EDGE('',*,*,#14103,.F.);
#19437=ORIENTED_EDGE('',*,*,#14104,.F.);
#19438=ORIENTED_EDGE('',*,*,#14105,.T.);
#19439=ORIENTED_EDGE('',*,*,#14104,.T.);
#19440=ORIENTED_EDGE('',*,*,#14106,.F.);
#19441=ORIENTED_EDGE('',*,*,#14107,.F.);
#19442=ORIENTED_EDGE('',*,*,#14108,.T.);
#19443=ORIENTED_EDGE('',*,*,#14107,.T.);
#19444=ORIENTED_EDGE('',*,*,#14109,.F.);
#19445=ORIENTED_EDGE('',*,*,#14110,.F.);
#19446=ORIENTED_EDGE('',*,*,#14111,.T.);
#19447=ORIENTED_EDGE('',*,*,#14110,.T.);
#19448=ORIENTED_EDGE('',*,*,#14112,.F.);
#19449=ORIENTED_EDGE('',*,*,#14113,.F.);
#19450=ORIENTED_EDGE('',*,*,#14114,.T.);
#19451=ORIENTED_EDGE('',*,*,#14113,.T.);
#19452=ORIENTED_EDGE('',*,*,#14115,.F.);
#19453=ORIENTED_EDGE('',*,*,#14116,.F.);
#19454=ORIENTED_EDGE('',*,*,#14117,.T.);
#19455=ORIENTED_EDGE('',*,*,#14116,.T.);
#19456=ORIENTED_EDGE('',*,*,#14118,.F.);
#19457=ORIENTED_EDGE('',*,*,#14119,.F.);
#19458=ORIENTED_EDGE('',*,*,#14120,.T.);
#19459=ORIENTED_EDGE('',*,*,#14119,.T.);
#19460=ORIENTED_EDGE('',*,*,#14121,.F.);
#19461=ORIENTED_EDGE('',*,*,#14122,.F.);
#19462=ORIENTED_EDGE('',*,*,#14123,.T.);
#19463=ORIENTED_EDGE('',*,*,#14122,.T.);
#19464=ORIENTED_EDGE('',*,*,#14124,.F.);
#19465=ORIENTED_EDGE('',*,*,#14102,.F.);
#19466=ORIENTED_EDGE('',*,*,#14124,.T.);
#19467=ORIENTED_EDGE('',*,*,#14121,.T.);
#19468=ORIENTED_EDGE('',*,*,#14118,.T.);
#19469=ORIENTED_EDGE('',*,*,#14115,.T.);
#19470=ORIENTED_EDGE('',*,*,#14112,.T.);
#19471=ORIENTED_EDGE('',*,*,#14109,.T.);
#19472=ORIENTED_EDGE('',*,*,#14106,.T.);
#19473=ORIENTED_EDGE('',*,*,#14103,.T.);
#19474=ORIENTED_EDGE('',*,*,#14123,.F.);
#19475=ORIENTED_EDGE('',*,*,#14101,.F.);
#19476=ORIENTED_EDGE('',*,*,#14105,.F.);
#19477=ORIENTED_EDGE('',*,*,#14108,.F.);
#19478=ORIENTED_EDGE('',*,*,#14111,.F.);
#19479=ORIENTED_EDGE('',*,*,#14114,.F.);
#19480=ORIENTED_EDGE('',*,*,#14117,.F.);
#19481=ORIENTED_EDGE('',*,*,#14120,.F.);
#19482=ORIENTED_EDGE('',*,*,#14125,.F.);
#19483=ORIENTED_EDGE('',*,*,#14126,.T.);
#19484=ORIENTED_EDGE('',*,*,#14127,.F.);
#19485=ORIENTED_EDGE('',*,*,#14128,.F.);
#19486=ORIENTED_EDGE('',*,*,#14129,.F.);
#19487=ORIENTED_EDGE('',*,*,#14128,.T.);
#19488=ORIENTED_EDGE('',*,*,#14130,.F.);
#19489=ORIENTED_EDGE('',*,*,#14131,.F.);
#19490=ORIENTED_EDGE('',*,*,#14132,.F.);
#19491=ORIENTED_EDGE('',*,*,#14131,.T.);
#19492=ORIENTED_EDGE('',*,*,#14133,.F.);
#19493=ORIENTED_EDGE('',*,*,#14134,.F.);
#19494=ORIENTED_EDGE('',*,*,#14135,.F.);
#19495=ORIENTED_EDGE('',*,*,#14134,.T.);
#19496=ORIENTED_EDGE('',*,*,#14136,.F.);
#19497=ORIENTED_EDGE('',*,*,#14137,.F.);
#19498=ORIENTED_EDGE('',*,*,#14138,.F.);
#19499=ORIENTED_EDGE('',*,*,#14137,.T.);
#19500=ORIENTED_EDGE('',*,*,#14139,.F.);
#19501=ORIENTED_EDGE('',*,*,#14140,.F.);
#19502=ORIENTED_EDGE('',*,*,#14141,.F.);
#19503=ORIENTED_EDGE('',*,*,#14140,.T.);
#19504=ORIENTED_EDGE('',*,*,#14142,.F.);
#19505=ORIENTED_EDGE('',*,*,#14143,.F.);
#19506=ORIENTED_EDGE('',*,*,#14144,.F.);
#19507=ORIENTED_EDGE('',*,*,#14143,.T.);
#19508=ORIENTED_EDGE('',*,*,#14145,.F.);
#19509=ORIENTED_EDGE('',*,*,#14146,.F.);
#19510=ORIENTED_EDGE('',*,*,#14147,.F.);
#19511=ORIENTED_EDGE('',*,*,#14146,.T.);
#19512=ORIENTED_EDGE('',*,*,#14148,.F.);
#19513=ORIENTED_EDGE('',*,*,#14126,.F.);
#19514=ORIENTED_EDGE('',*,*,#14147,.T.);
#19515=ORIENTED_EDGE('',*,*,#14125,.T.);
#19516=ORIENTED_EDGE('',*,*,#14129,.T.);
#19517=ORIENTED_EDGE('',*,*,#14132,.T.);
#19518=ORIENTED_EDGE('',*,*,#14135,.T.);
#19519=ORIENTED_EDGE('',*,*,#14138,.T.);
#19520=ORIENTED_EDGE('',*,*,#14141,.T.);
#19521=ORIENTED_EDGE('',*,*,#14144,.T.);
#19522=ORIENTED_EDGE('',*,*,#14148,.T.);
#19523=ORIENTED_EDGE('',*,*,#14145,.T.);
#19524=ORIENTED_EDGE('',*,*,#14142,.T.);
#19525=ORIENTED_EDGE('',*,*,#14139,.T.);
#19526=ORIENTED_EDGE('',*,*,#14136,.T.);
#19527=ORIENTED_EDGE('',*,*,#14133,.T.);
#19528=ORIENTED_EDGE('',*,*,#14130,.T.);
#19529=ORIENTED_EDGE('',*,*,#14127,.T.);
#19530=ORIENTED_EDGE('',*,*,#14149,.T.);
#19531=ORIENTED_EDGE('',*,*,#14150,.T.);
#19532=ORIENTED_EDGE('',*,*,#14151,.T.);
#19533=ORIENTED_EDGE('',*,*,#14150,.F.);
#19534=ORIENTED_EDGE('',*,*,#14151,.F.);
#19535=ORIENTED_EDGE('',*,*,#14152,.T.);
#19536=ORIENTED_EDGE('',*,*,#14153,.T.);
#19537=ORIENTED_EDGE('',*,*,#14152,.F.);
#19538=ORIENTED_EDGE('',*,*,#14154,.T.);
#19539=ORIENTED_EDGE('',*,*,#14149,.F.);
#19540=ORIENTED_EDGE('',*,*,#14154,.F.);
#19541=ORIENTED_EDGE('',*,*,#14155,.T.);
#19542=ORIENTED_EDGE('',*,*,#14156,.T.);
#19543=ORIENTED_EDGE('',*,*,#14155,.F.);
#19544=ORIENTED_EDGE('',*,*,#14156,.F.);
#19545=ORIENTED_EDGE('',*,*,#14153,.F.);
#19546=ORIENTED_EDGE('',*,*,#14157,.T.);
#19547=ORIENTED_EDGE('',*,*,#14158,.T.);
#19548=ORIENTED_EDGE('',*,*,#14159,.T.);
#19549=ORIENTED_EDGE('',*,*,#14160,.F.);
#19550=ORIENTED_EDGE('',*,*,#14161,.T.);
#19551=ORIENTED_EDGE('',*,*,#14162,.T.);
#19552=ORIENTED_EDGE('',*,*,#14163,.T.);
#19553=ORIENTED_EDGE('',*,*,#14158,.F.);
#19554=ORIENTED_EDGE('',*,*,#14164,.T.);
#19555=ORIENTED_EDGE('',*,*,#14165,.T.);
#19556=ORIENTED_EDGE('',*,*,#14166,.T.);
#19557=ORIENTED_EDGE('',*,*,#14162,.F.);
#19558=ORIENTED_EDGE('',*,*,#14167,.T.);
#19559=ORIENTED_EDGE('',*,*,#14168,.T.);
#19560=ORIENTED_EDGE('',*,*,#14169,.T.);
#19561=ORIENTED_EDGE('',*,*,#14165,.F.);
#19562=ORIENTED_EDGE('',*,*,#14170,.T.);
#19563=ORIENTED_EDGE('',*,*,#14171,.T.);
#19564=ORIENTED_EDGE('',*,*,#14172,.T.);
#19565=ORIENTED_EDGE('',*,*,#14168,.F.);
#19566=ORIENTED_EDGE('',*,*,#14173,.T.);
#19567=ORIENTED_EDGE('',*,*,#14160,.T.);
#19568=ORIENTED_EDGE('',*,*,#14174,.T.);
#19569=ORIENTED_EDGE('',*,*,#14171,.F.);
#19570=ORIENTED_EDGE('',*,*,#14173,.F.);
#19571=ORIENTED_EDGE('',*,*,#14170,.F.);
#19572=ORIENTED_EDGE('',*,*,#14167,.F.);
#19573=ORIENTED_EDGE('',*,*,#14164,.F.);
#19574=ORIENTED_EDGE('',*,*,#14161,.F.);
#19575=ORIENTED_EDGE('',*,*,#14157,.F.);
#19576=ORIENTED_EDGE('',*,*,#14174,.F.);
#19577=ORIENTED_EDGE('',*,*,#14159,.F.);
#19578=ORIENTED_EDGE('',*,*,#14163,.F.);
#19579=ORIENTED_EDGE('',*,*,#14166,.F.);
#19580=ORIENTED_EDGE('',*,*,#14169,.F.);
#19581=ORIENTED_EDGE('',*,*,#14172,.F.);
#19582=ORIENTED_EDGE('',*,*,#14175,.T.);
#19583=ORIENTED_EDGE('',*,*,#14176,.F.);
#19584=ORIENTED_EDGE('',*,*,#14175,.F.);
#19585=ORIENTED_EDGE('',*,*,#14177,.T.);
#19586=ORIENTED_EDGE('',*,*,#14178,.T.);
#19587=ORIENTED_EDGE('',*,*,#14177,.F.);
#19588=ORIENTED_EDGE('',*,*,#14178,.F.);
#19589=ORIENTED_EDGE('',*,*,#14179,.F.);
#19590=ORIENTED_EDGE('',*,*,#14180,.F.);
#19591=ORIENTED_EDGE('',*,*,#14181,.T.);
#19592=ORIENTED_EDGE('',*,*,#14179,.T.);
#19593=ORIENTED_EDGE('',*,*,#14181,.F.);
#19594=ORIENTED_EDGE('',*,*,#14182,.F.);
#19595=ORIENTED_EDGE('',*,*,#14183,.T.);
#19596=ORIENTED_EDGE('',*,*,#14180,.T.);
#19597=ORIENTED_EDGE('',*,*,#14183,.F.);
#19598=ORIENTED_EDGE('',*,*,#14184,.F.);
#19599=ORIENTED_EDGE('',*,*,#14185,.T.);
#19600=ORIENTED_EDGE('',*,*,#14182,.T.);
#19601=ORIENTED_EDGE('',*,*,#14185,.F.);
#19602=ORIENTED_EDGE('',*,*,#14184,.T.);
#19603=ORIENTED_EDGE('',*,*,#14186,.F.);
#19604=ORIENTED_EDGE('',*,*,#14187,.F.);
#19605=ORIENTED_EDGE('',*,*,#14188,.T.);
#19606=ORIENTED_EDGE('',*,*,#14186,.T.);
#19607=ORIENTED_EDGE('',*,*,#14188,.F.);
#19608=ORIENTED_EDGE('',*,*,#14176,.T.);
#19609=ORIENTED_EDGE('',*,*,#14189,.T.);
#19610=ORIENTED_EDGE('',*,*,#14187,.T.);
#19611=ORIENTED_EDGE('',*,*,#14189,.F.);
#19612=ORIENTED_EDGE('',*,*,#14190,.T.);
#19613=ORIENTED_EDGE('',*,*,#14191,.T.);
#19614=ORIENTED_EDGE('',*,*,#14192,.T.);
#19615=ORIENTED_EDGE('',*,*,#14193,.T.);
#19616=ORIENTED_EDGE('',*,*,#14194,.T.);
#19617=ORIENTED_EDGE('',*,*,#14195,.T.);
#19618=ORIENTED_EDGE('',*,*,#14190,.F.);
#19619=ORIENTED_EDGE('',*,*,#14196,.T.);
#19620=ORIENTED_EDGE('',*,*,#14197,.T.);
#19621=ORIENTED_EDGE('',*,*,#14198,.T.);
#19622=ORIENTED_EDGE('',*,*,#14194,.F.);
#19623=ORIENTED_EDGE('',*,*,#14199,.T.);
#19624=ORIENTED_EDGE('',*,*,#14200,.T.);
#19625=ORIENTED_EDGE('',*,*,#14201,.T.);
#19626=ORIENTED_EDGE('',*,*,#14197,.F.);
#19627=ORIENTED_EDGE('',*,*,#14202,.T.);
#19628=ORIENTED_EDGE('',*,*,#14203,.T.);
#19629=ORIENTED_EDGE('',*,*,#14204,.T.);
#19630=ORIENTED_EDGE('',*,*,#14200,.F.);
#19631=ORIENTED_EDGE('',*,*,#14205,.T.);
#19632=ORIENTED_EDGE('',*,*,#14206,.T.);
#19633=ORIENTED_EDGE('',*,*,#14207,.T.);
#19634=ORIENTED_EDGE('',*,*,#14203,.F.);
#19635=ORIENTED_EDGE('',*,*,#14208,.T.);
#19636=ORIENTED_EDGE('',*,*,#14209,.T.);
#19637=ORIENTED_EDGE('',*,*,#14210,.T.);
#19638=ORIENTED_EDGE('',*,*,#14206,.F.);
#19639=ORIENTED_EDGE('',*,*,#14211,.T.);
#19640=ORIENTED_EDGE('',*,*,#14212,.T.);
#19641=ORIENTED_EDGE('',*,*,#14213,.T.);
#19642=ORIENTED_EDGE('',*,*,#14209,.F.);
#19643=ORIENTED_EDGE('',*,*,#14214,.T.);
#19644=ORIENTED_EDGE('',*,*,#14215,.F.);
#19645=ORIENTED_EDGE('',*,*,#14216,.F.);
#19646=ORIENTED_EDGE('',*,*,#14217,.T.);
#19647=ORIENTED_EDGE('',*,*,#14218,.T.);
#19648=ORIENTED_EDGE('',*,*,#14219,.T.);
#19649=ORIENTED_EDGE('',*,*,#14220,.F.);
#19650=ORIENTED_EDGE('',*,*,#14221,.F.);
#19651=ORIENTED_EDGE('',*,*,#14222,.T.);
#19652=ORIENTED_EDGE('',*,*,#14223,.T.);
#19653=ORIENTED_EDGE('',*,*,#14218,.F.);
#19654=ORIENTED_EDGE('',*,*,#14224,.F.);
#19655=ORIENTED_EDGE('',*,*,#14225,.T.);
#19656=ORIENTED_EDGE('',*,*,#14226,.T.);
#19657=ORIENTED_EDGE('',*,*,#14222,.F.);
#19658=ORIENTED_EDGE('',*,*,#14227,.F.);
#19659=ORIENTED_EDGE('',*,*,#14228,.T.);
#19660=ORIENTED_EDGE('',*,*,#14229,.T.);
#19661=ORIENTED_EDGE('',*,*,#14225,.F.);
#19662=ORIENTED_EDGE('',*,*,#14230,.F.);
#19663=ORIENTED_EDGE('',*,*,#14231,.T.);
#19664=ORIENTED_EDGE('',*,*,#14232,.T.);
#19665=ORIENTED_EDGE('',*,*,#14228,.F.);
#19666=ORIENTED_EDGE('',*,*,#14233,.F.);
#19667=ORIENTED_EDGE('',*,*,#14234,.T.);
#19668=ORIENTED_EDGE('',*,*,#14235,.T.);
#19669=ORIENTED_EDGE('',*,*,#14231,.F.);
#19670=ORIENTED_EDGE('',*,*,#14236,.F.);
#19671=ORIENTED_EDGE('',*,*,#14237,.T.);
#19672=ORIENTED_EDGE('',*,*,#14238,.T.);
#19673=ORIENTED_EDGE('',*,*,#14234,.F.);
#19674=ORIENTED_EDGE('',*,*,#14239,.F.);
#19675=ORIENTED_EDGE('',*,*,#14240,.T.);
#19676=ORIENTED_EDGE('',*,*,#14241,.T.);
#19677=ORIENTED_EDGE('',*,*,#14237,.F.);
#19678=ORIENTED_EDGE('',*,*,#14242,.F.);
#19679=ORIENTED_EDGE('',*,*,#14243,.F.);
#19680=ORIENTED_EDGE('',*,*,#14244,.F.);
#19681=ORIENTED_EDGE('',*,*,#14245,.F.);
#19682=ORIENTED_EDGE('',*,*,#14246,.T.);
#19683=ORIENTED_EDGE('',*,*,#14243,.T.);
#19684=ORIENTED_EDGE('',*,*,#14247,.T.);
#19685=ORIENTED_EDGE('',*,*,#14240,.F.);
#19686=ORIENTED_EDGE('',*,*,#14248,.F.);
#19687=ORIENTED_EDGE('',*,*,#14249,.F.);
#19688=ORIENTED_EDGE('',*,*,#14219,.F.);
#19689=ORIENTED_EDGE('',*,*,#14223,.F.);
#19690=ORIENTED_EDGE('',*,*,#14226,.F.);
#19691=ORIENTED_EDGE('',*,*,#14229,.F.);
#19692=ORIENTED_EDGE('',*,*,#14232,.F.);
#19693=ORIENTED_EDGE('',*,*,#14235,.F.);
#19694=ORIENTED_EDGE('',*,*,#14238,.F.);
#19695=ORIENTED_EDGE('',*,*,#14241,.F.);
#19696=ORIENTED_EDGE('',*,*,#14247,.F.);
#19697=ORIENTED_EDGE('',*,*,#14246,.F.);
#19698=ORIENTED_EDGE('',*,*,#14250,.F.);
#19699=ORIENTED_EDGE('',*,*,#14191,.F.);
#19700=ORIENTED_EDGE('',*,*,#14195,.F.);
#19701=ORIENTED_EDGE('',*,*,#14198,.F.);
#19702=ORIENTED_EDGE('',*,*,#14201,.F.);
#19703=ORIENTED_EDGE('',*,*,#14204,.F.);
#19704=ORIENTED_EDGE('',*,*,#14207,.F.);
#19705=ORIENTED_EDGE('',*,*,#14210,.F.);
#19706=ORIENTED_EDGE('',*,*,#14213,.F.);
#19707=ORIENTED_EDGE('',*,*,#14251,.F.);
#19708=ORIENTED_EDGE('',*,*,#14217,.F.);
#19709=ORIENTED_EDGE('',*,*,#14252,.F.);
#19710=ORIENTED_EDGE('',*,*,#14253,.F.);
#19711=ORIENTED_EDGE('',*,*,#14214,.F.);
#19712=ORIENTED_EDGE('',*,*,#14211,.F.);
#19713=ORIENTED_EDGE('',*,*,#14208,.F.);
#19714=ORIENTED_EDGE('',*,*,#14205,.F.);
#19715=ORIENTED_EDGE('',*,*,#14202,.F.);
#19716=ORIENTED_EDGE('',*,*,#14199,.F.);
#19717=ORIENTED_EDGE('',*,*,#14196,.F.);
#19718=ORIENTED_EDGE('',*,*,#14193,.F.);
#19719=ORIENTED_EDGE('',*,*,#14254,.F.);
#19720=ORIENTED_EDGE('',*,*,#14244,.T.);
#19721=ORIENTED_EDGE('',*,*,#14248,.T.);
#19722=ORIENTED_EDGE('',*,*,#14242,.T.);
#19723=ORIENTED_EDGE('',*,*,#14239,.T.);
#19724=ORIENTED_EDGE('',*,*,#14236,.T.);
#19725=ORIENTED_EDGE('',*,*,#14233,.T.);
#19726=ORIENTED_EDGE('',*,*,#14230,.T.);
#19727=ORIENTED_EDGE('',*,*,#14227,.T.);
#19728=ORIENTED_EDGE('',*,*,#14224,.T.);
#19729=ORIENTED_EDGE('',*,*,#14221,.T.);
#19730=ORIENTED_EDGE('',*,*,#14255,.T.);
#19731=ORIENTED_EDGE('',*,*,#14256,.T.);
#19732=ORIENTED_EDGE('',*,*,#14252,.T.);
#19733=ORIENTED_EDGE('',*,*,#14220,.T.);
#19734=ORIENTED_EDGE('',*,*,#14249,.T.);
#19735=ORIENTED_EDGE('',*,*,#14216,.T.);
#19736=ORIENTED_EDGE('',*,*,#14257,.T.);
#19737=ORIENTED_EDGE('',*,*,#14258,.T.);
#19738=ORIENTED_EDGE('',*,*,#14259,.T.);
#19739=ORIENTED_EDGE('',*,*,#14260,.T.);
#19740=ORIENTED_EDGE('',*,*,#14261,.F.);
#19741=ORIENTED_EDGE('',*,*,#14262,.T.);
#19742=ORIENTED_EDGE('',*,*,#14260,.F.);
#19743=ORIENTED_EDGE('',*,*,#14262,.F.);
#19744=ORIENTED_EDGE('',*,*,#14263,.F.);
#19745=ORIENTED_EDGE('',*,*,#14264,.T.);
#19746=ORIENTED_EDGE('',*,*,#14259,.F.);
#19747=ORIENTED_EDGE('',*,*,#14264,.F.);
#19748=ORIENTED_EDGE('',*,*,#14265,.F.);
#19749=ORIENTED_EDGE('',*,*,#14266,.T.);
#19750=ORIENTED_EDGE('',*,*,#14258,.F.);
#19751=ORIENTED_EDGE('',*,*,#14266,.F.);
#19752=ORIENTED_EDGE('',*,*,#14267,.F.);
#19753=ORIENTED_EDGE('',*,*,#14268,.F.);
#19754=ORIENTED_EDGE('',*,*,#14255,.F.);
#19755=ORIENTED_EDGE('',*,*,#14269,.F.);
#19756=ORIENTED_EDGE('',*,*,#14267,.T.);
#19757=ORIENTED_EDGE('',*,*,#14270,.F.);
#19758=ORIENTED_EDGE('',*,*,#14261,.T.);
#19759=ORIENTED_EDGE('',*,*,#14263,.T.);
#19760=ORIENTED_EDGE('',*,*,#14265,.T.);
#19761=ORIENTED_EDGE('',*,*,#14271,.T.);
#19762=ORIENTED_EDGE('',*,*,#14269,.T.);
#19763=ORIENTED_EDGE('',*,*,#14256,.F.);
#19764=ORIENTED_EDGE('',*,*,#14268,.T.);
#19765=ORIENTED_EDGE('',*,*,#14270,.T.);
#19766=ORIENTED_EDGE('',*,*,#14215,.T.);
#19767=ORIENTED_EDGE('',*,*,#14251,.T.);
#19768=ORIENTED_EDGE('',*,*,#14212,.F.);
#19769=ORIENTED_EDGE('',*,*,#14253,.T.);
#19770=ORIENTED_EDGE('',*,*,#14257,.F.);
#19771=ORIENTED_EDGE('',*,*,#14271,.F.);
#19772=ORIENTED_EDGE('',*,*,#14272,.T.);
#19773=ORIENTED_EDGE('',*,*,#14273,.T.);
#19774=ORIENTED_EDGE('',*,*,#14272,.F.);
#19775=ORIENTED_EDGE('',*,*,#14273,.F.);
#19776=ORIENTED_EDGE('',*,*,#14254,.T.);
#19777=ORIENTED_EDGE('',*,*,#14192,.F.);
#19778=ORIENTED_EDGE('',*,*,#14250,.T.);
#19779=ORIENTED_EDGE('',*,*,#14245,.T.);
#19780=ORIENTED_EDGE('',*,*,#14274,.F.);
#19781=ORIENTED_EDGE('',*,*,#14275,.F.);
#19782=ORIENTED_EDGE('',*,*,#14276,.T.);
#19783=ORIENTED_EDGE('',*,*,#14274,.T.);
#19784=ORIENTED_EDGE('',*,*,#14276,.F.);
#19785=ORIENTED_EDGE('',*,*,#14277,.F.);
#19786=ORIENTED_EDGE('',*,*,#14278,.T.);
#19787=ORIENTED_EDGE('',*,*,#14275,.T.);
#19788=ORIENTED_EDGE('',*,*,#14278,.F.);
#19789=ORIENTED_EDGE('',*,*,#14279,.F.);
#19790=ORIENTED_EDGE('',*,*,#14280,.T.);
#19791=ORIENTED_EDGE('',*,*,#14277,.T.);
#19792=ORIENTED_EDGE('',*,*,#14280,.F.);
#19793=ORIENTED_EDGE('',*,*,#14279,.T.);
#19794=ORIENTED_EDGE('',*,*,#14281,.F.);
#19795=ORIENTED_EDGE('',*,*,#14282,.F.);
#19796=ORIENTED_EDGE('',*,*,#14283,.T.);
#19797=ORIENTED_EDGE('',*,*,#14281,.T.);
#19798=ORIENTED_EDGE('',*,*,#14283,.F.);
#19799=ORIENTED_EDGE('',*,*,#14284,.F.);
#19800=ORIENTED_EDGE('',*,*,#14285,.T.);
#19801=ORIENTED_EDGE('',*,*,#14282,.T.);
#19802=ORIENTED_EDGE('',*,*,#14285,.F.);
#19803=ORIENTED_EDGE('',*,*,#14286,.F.);
#19804=ORIENTED_EDGE('',*,*,#14287,.T.);
#19805=ORIENTED_EDGE('',*,*,#14284,.T.);
#19806=ORIENTED_EDGE('',*,*,#14287,.F.);
#19807=ORIENTED_EDGE('',*,*,#14286,.T.);
#19808=ORIENTED_EDGE('',*,*,#14288,.T.);
#19809=ORIENTED_EDGE('',*,*,#14289,.T.);
#19810=ORIENTED_EDGE('',*,*,#14290,.T.);
#19811=ORIENTED_EDGE('',*,*,#14291,.F.);
#19812=ORIENTED_EDGE('',*,*,#14292,.T.);
#19813=ORIENTED_EDGE('',*,*,#14293,.T.);
#19814=ORIENTED_EDGE('',*,*,#14294,.T.);
#19815=ORIENTED_EDGE('',*,*,#14289,.F.);
#19816=ORIENTED_EDGE('',*,*,#14295,.T.);
#19817=ORIENTED_EDGE('',*,*,#14296,.T.);
#19818=ORIENTED_EDGE('',*,*,#14297,.T.);
#19819=ORIENTED_EDGE('',*,*,#14293,.F.);
#19820=ORIENTED_EDGE('',*,*,#14298,.T.);
#19821=ORIENTED_EDGE('',*,*,#14299,.T.);
#19822=ORIENTED_EDGE('',*,*,#14300,.T.);
#19823=ORIENTED_EDGE('',*,*,#14296,.F.);
#19824=ORIENTED_EDGE('',*,*,#14301,.T.);
#19825=ORIENTED_EDGE('',*,*,#14302,.T.);
#19826=ORIENTED_EDGE('',*,*,#14303,.T.);
#19827=ORIENTED_EDGE('',*,*,#14299,.F.);
#19828=ORIENTED_EDGE('',*,*,#14304,.T.);
#19829=ORIENTED_EDGE('',*,*,#14291,.T.);
#19830=ORIENTED_EDGE('',*,*,#14305,.T.);
#19831=ORIENTED_EDGE('',*,*,#14302,.F.);
#19832=ORIENTED_EDGE('',*,*,#14304,.F.);
#19833=ORIENTED_EDGE('',*,*,#14301,.F.);
#19834=ORIENTED_EDGE('',*,*,#14298,.F.);
#19835=ORIENTED_EDGE('',*,*,#14295,.F.);
#19836=ORIENTED_EDGE('',*,*,#14292,.F.);
#19837=ORIENTED_EDGE('',*,*,#14288,.F.);
#19838=ORIENTED_EDGE('',*,*,#14305,.F.);
#19839=ORIENTED_EDGE('',*,*,#14290,.F.);
#19840=ORIENTED_EDGE('',*,*,#14294,.F.);
#19841=ORIENTED_EDGE('',*,*,#14297,.F.);
#19842=ORIENTED_EDGE('',*,*,#14300,.F.);
#19843=ORIENTED_EDGE('',*,*,#14303,.F.);
#19844=ORIENTED_EDGE('',*,*,#14306,.F.);
#19845=ORIENTED_EDGE('',*,*,#14307,.F.);
#19846=ORIENTED_EDGE('',*,*,#14308,.T.);
#19847=ORIENTED_EDGE('',*,*,#14306,.T.);
#19848=ORIENTED_EDGE('',*,*,#14308,.F.);
#19849=ORIENTED_EDGE('',*,*,#14309,.F.);
#19850=ORIENTED_EDGE('',*,*,#14310,.T.);
#19851=ORIENTED_EDGE('',*,*,#14307,.T.);
#19852=ORIENTED_EDGE('',*,*,#14310,.F.);
#19853=ORIENTED_EDGE('',*,*,#14311,.F.);
#19854=ORIENTED_EDGE('',*,*,#14312,.T.);
#19855=ORIENTED_EDGE('',*,*,#14309,.T.);
#19856=ORIENTED_EDGE('',*,*,#14312,.F.);
#19857=ORIENTED_EDGE('',*,*,#14311,.T.);
#19858=ORIENTED_EDGE('',*,*,#14313,.F.);
#19859=ORIENTED_EDGE('',*,*,#14314,.F.);
#19860=ORIENTED_EDGE('',*,*,#14315,.T.);
#19861=ORIENTED_EDGE('',*,*,#14313,.T.);
#19862=ORIENTED_EDGE('',*,*,#14315,.F.);
#19863=ORIENTED_EDGE('',*,*,#14316,.F.);
#19864=ORIENTED_EDGE('',*,*,#14317,.T.);
#19865=ORIENTED_EDGE('',*,*,#14314,.T.);
#19866=ORIENTED_EDGE('',*,*,#14317,.F.);
#19867=ORIENTED_EDGE('',*,*,#14318,.F.);
#19868=ORIENTED_EDGE('',*,*,#14319,.T.);
#19869=ORIENTED_EDGE('',*,*,#14316,.T.);
#19870=ORIENTED_EDGE('',*,*,#14319,.F.);
#19871=ORIENTED_EDGE('',*,*,#14318,.T.);
#19872=ORIENTED_EDGE('',*,*,#14320,.T.);
#19873=ORIENTED_EDGE('',*,*,#14321,.T.);
#19874=ORIENTED_EDGE('',*,*,#14322,.T.);
#19875=ORIENTED_EDGE('',*,*,#14323,.F.);
#19876=ORIENTED_EDGE('',*,*,#14324,.T.);
#19877=ORIENTED_EDGE('',*,*,#14325,.T.);
#19878=ORIENTED_EDGE('',*,*,#14326,.T.);
#19879=ORIENTED_EDGE('',*,*,#14321,.F.);
#19880=ORIENTED_EDGE('',*,*,#14327,.T.);
#19881=ORIENTED_EDGE('',*,*,#14328,.T.);
#19882=ORIENTED_EDGE('',*,*,#14329,.T.);
#19883=ORIENTED_EDGE('',*,*,#14325,.F.);
#19884=ORIENTED_EDGE('',*,*,#14330,.T.);
#19885=ORIENTED_EDGE('',*,*,#14331,.T.);
#19886=ORIENTED_EDGE('',*,*,#14332,.T.);
#19887=ORIENTED_EDGE('',*,*,#14328,.F.);
#19888=ORIENTED_EDGE('',*,*,#14333,.T.);
#19889=ORIENTED_EDGE('',*,*,#14334,.T.);
#19890=ORIENTED_EDGE('',*,*,#14335,.T.);
#19891=ORIENTED_EDGE('',*,*,#14331,.F.);
#19892=ORIENTED_EDGE('',*,*,#14336,.T.);
#19893=ORIENTED_EDGE('',*,*,#14323,.T.);
#19894=ORIENTED_EDGE('',*,*,#14337,.T.);
#19895=ORIENTED_EDGE('',*,*,#14334,.F.);
#19896=ORIENTED_EDGE('',*,*,#14336,.F.);
#19897=ORIENTED_EDGE('',*,*,#14333,.F.);
#19898=ORIENTED_EDGE('',*,*,#14330,.F.);
#19899=ORIENTED_EDGE('',*,*,#14327,.F.);
#19900=ORIENTED_EDGE('',*,*,#14324,.F.);
#19901=ORIENTED_EDGE('',*,*,#14320,.F.);
#19902=ORIENTED_EDGE('',*,*,#14337,.F.);
#19903=ORIENTED_EDGE('',*,*,#14322,.F.);
#19904=ORIENTED_EDGE('',*,*,#14326,.F.);
#19905=ORIENTED_EDGE('',*,*,#14329,.F.);
#19906=ORIENTED_EDGE('',*,*,#14332,.F.);
#19907=ORIENTED_EDGE('',*,*,#14335,.F.);
#19908=ORIENTED_EDGE('',*,*,#14338,.F.);
#19909=ORIENTED_EDGE('',*,*,#14339,.T.);
#19910=ORIENTED_EDGE('',*,*,#14340,.T.);
#19911=ORIENTED_EDGE('',*,*,#14341,.T.);
#19912=ORIENTED_EDGE('',*,*,#14342,.F.);
#19913=ORIENTED_EDGE('',*,*,#14343,.T.);
#19914=ORIENTED_EDGE('',*,*,#14338,.T.);
#19915=ORIENTED_EDGE('',*,*,#14344,.T.);
#19916=ORIENTED_EDGE('',*,*,#14345,.F.);
#19917=ORIENTED_EDGE('',*,*,#14346,.T.);
#19918=ORIENTED_EDGE('',*,*,#14342,.T.);
#19919=ORIENTED_EDGE('',*,*,#14347,.T.);
#19920=ORIENTED_EDGE('',*,*,#14348,.F.);
#19921=ORIENTED_EDGE('',*,*,#14349,.T.);
#19922=ORIENTED_EDGE('',*,*,#14345,.T.);
#19923=ORIENTED_EDGE('',*,*,#14350,.T.);
#19924=ORIENTED_EDGE('',*,*,#14351,.F.);
#19925=ORIENTED_EDGE('',*,*,#14352,.T.);
#19926=ORIENTED_EDGE('',*,*,#14348,.T.);
#19927=ORIENTED_EDGE('',*,*,#14353,.T.);
#19928=ORIENTED_EDGE('',*,*,#14354,.F.);
#19929=ORIENTED_EDGE('',*,*,#14355,.T.);
#19930=ORIENTED_EDGE('',*,*,#14351,.T.);
#19931=ORIENTED_EDGE('',*,*,#14356,.T.);
#19932=ORIENTED_EDGE('',*,*,#14357,.F.);
#19933=ORIENTED_EDGE('',*,*,#14358,.T.);
#19934=ORIENTED_EDGE('',*,*,#14354,.T.);
#19935=ORIENTED_EDGE('',*,*,#14359,.T.);
#19936=ORIENTED_EDGE('',*,*,#14360,.F.);
#19937=ORIENTED_EDGE('',*,*,#14361,.T.);
#19938=ORIENTED_EDGE('',*,*,#14357,.T.);
#19939=ORIENTED_EDGE('',*,*,#14362,.T.);
#19940=ORIENTED_EDGE('',*,*,#14363,.F.);
#19941=ORIENTED_EDGE('',*,*,#14364,.T.);
#19942=ORIENTED_EDGE('',*,*,#14360,.T.);
#19943=ORIENTED_EDGE('',*,*,#14365,.T.);
#19944=ORIENTED_EDGE('',*,*,#14366,.F.);
#19945=ORIENTED_EDGE('',*,*,#14367,.T.);
#19946=ORIENTED_EDGE('',*,*,#14363,.T.);
#19947=ORIENTED_EDGE('',*,*,#14368,.T.);
#19948=ORIENTED_EDGE('',*,*,#14369,.F.);
#19949=ORIENTED_EDGE('',*,*,#14370,.T.);
#19950=ORIENTED_EDGE('',*,*,#14366,.T.);
#19951=ORIENTED_EDGE('',*,*,#14371,.T.);
#19952=ORIENTED_EDGE('',*,*,#14372,.F.);
#19953=ORIENTED_EDGE('',*,*,#14373,.T.);
#19954=ORIENTED_EDGE('',*,*,#14369,.T.);
#19955=ORIENTED_EDGE('',*,*,#14374,.T.);
#19956=ORIENTED_EDGE('',*,*,#14375,.F.);
#19957=ORIENTED_EDGE('',*,*,#14376,.T.);
#19958=ORIENTED_EDGE('',*,*,#14372,.T.);
#19959=ORIENTED_EDGE('',*,*,#14377,.T.);
#19960=ORIENTED_EDGE('',*,*,#14378,.F.);
#19961=ORIENTED_EDGE('',*,*,#14379,.T.);
#19962=ORIENTED_EDGE('',*,*,#14375,.T.);
#19963=ORIENTED_EDGE('',*,*,#14380,.T.);
#19964=ORIENTED_EDGE('',*,*,#14381,.F.);
#19965=ORIENTED_EDGE('',*,*,#14382,.T.);
#19966=ORIENTED_EDGE('',*,*,#14378,.T.);
#19967=ORIENTED_EDGE('',*,*,#14383,.T.);
#19968=ORIENTED_EDGE('',*,*,#14384,.F.);
#19969=ORIENTED_EDGE('',*,*,#14385,.T.);
#19970=ORIENTED_EDGE('',*,*,#14381,.T.);
#19971=ORIENTED_EDGE('',*,*,#14386,.T.);
#19972=ORIENTED_EDGE('',*,*,#14387,.F.);
#19973=ORIENTED_EDGE('',*,*,#14388,.T.);
#19974=ORIENTED_EDGE('',*,*,#14384,.T.);
#19975=ORIENTED_EDGE('',*,*,#14389,.T.);
#19976=ORIENTED_EDGE('',*,*,#14390,.F.);
#19977=ORIENTED_EDGE('',*,*,#14391,.T.);
#19978=ORIENTED_EDGE('',*,*,#14387,.T.);
#19979=ORIENTED_EDGE('',*,*,#14392,.T.);
#19980=ORIENTED_EDGE('',*,*,#14393,.F.);
#19981=ORIENTED_EDGE('',*,*,#14394,.T.);
#19982=ORIENTED_EDGE('',*,*,#14390,.T.);
#19983=ORIENTED_EDGE('',*,*,#14395,.T.);
#19984=ORIENTED_EDGE('',*,*,#14396,.F.);
#19985=ORIENTED_EDGE('',*,*,#14397,.T.);
#19986=ORIENTED_EDGE('',*,*,#14393,.T.);
#19987=ORIENTED_EDGE('',*,*,#14398,.T.);
#19988=ORIENTED_EDGE('',*,*,#14399,.F.);
#19989=ORIENTED_EDGE('',*,*,#14400,.T.);
#19990=ORIENTED_EDGE('',*,*,#14396,.T.);
#19991=ORIENTED_EDGE('',*,*,#14401,.T.);
#19992=ORIENTED_EDGE('',*,*,#14402,.F.);
#19993=ORIENTED_EDGE('',*,*,#14403,.T.);
#19994=ORIENTED_EDGE('',*,*,#14399,.T.);
#19995=ORIENTED_EDGE('',*,*,#14404,.T.);
#19996=ORIENTED_EDGE('',*,*,#14405,.F.);
#19997=ORIENTED_EDGE('',*,*,#14406,.T.);
#19998=ORIENTED_EDGE('',*,*,#14402,.T.);
#19999=ORIENTED_EDGE('',*,*,#14407,.T.);
#20000=ORIENTED_EDGE('',*,*,#14408,.F.);
#20001=ORIENTED_EDGE('',*,*,#14409,.T.);
#20002=ORIENTED_EDGE('',*,*,#14405,.T.);
#20003=ORIENTED_EDGE('',*,*,#14410,.T.);
#20004=ORIENTED_EDGE('',*,*,#14411,.F.);
#20005=ORIENTED_EDGE('',*,*,#14412,.T.);
#20006=ORIENTED_EDGE('',*,*,#14408,.T.);
#20007=ORIENTED_EDGE('',*,*,#14413,.T.);
#20008=ORIENTED_EDGE('',*,*,#14414,.F.);
#20009=ORIENTED_EDGE('',*,*,#14415,.T.);
#20010=ORIENTED_EDGE('',*,*,#14411,.T.);
#20011=ORIENTED_EDGE('',*,*,#14416,.T.);
#20012=ORIENTED_EDGE('',*,*,#14417,.F.);
#20013=ORIENTED_EDGE('',*,*,#14418,.T.);
#20014=ORIENTED_EDGE('',*,*,#14414,.T.);
#20015=ORIENTED_EDGE('',*,*,#14419,.T.);
#20016=ORIENTED_EDGE('',*,*,#14420,.F.);
#20017=ORIENTED_EDGE('',*,*,#14421,.T.);
#20018=ORIENTED_EDGE('',*,*,#14417,.T.);
#20019=ORIENTED_EDGE('',*,*,#14422,.T.);
#20020=ORIENTED_EDGE('',*,*,#14423,.F.);
#20021=ORIENTED_EDGE('',*,*,#14424,.T.);
#20022=ORIENTED_EDGE('',*,*,#14420,.T.);
#20023=ORIENTED_EDGE('',*,*,#14425,.T.);
#20024=ORIENTED_EDGE('',*,*,#14426,.F.);
#20025=ORIENTED_EDGE('',*,*,#14427,.T.);
#20026=ORIENTED_EDGE('',*,*,#14423,.T.);
#20027=ORIENTED_EDGE('',*,*,#14428,.T.);
#20028=ORIENTED_EDGE('',*,*,#14429,.F.);
#20029=ORIENTED_EDGE('',*,*,#14430,.T.);
#20030=ORIENTED_EDGE('',*,*,#14426,.T.);
#20031=ORIENTED_EDGE('',*,*,#14431,.T.);
#20032=ORIENTED_EDGE('',*,*,#14432,.F.);
#20033=ORIENTED_EDGE('',*,*,#14433,.T.);
#20034=ORIENTED_EDGE('',*,*,#14429,.T.);
#20035=ORIENTED_EDGE('',*,*,#14434,.T.);
#20036=ORIENTED_EDGE('',*,*,#14435,.F.);
#20037=ORIENTED_EDGE('',*,*,#14436,.T.);
#20038=ORIENTED_EDGE('',*,*,#14432,.T.);
#20039=ORIENTED_EDGE('',*,*,#14437,.T.);
#20040=ORIENTED_EDGE('',*,*,#14438,.F.);
#20041=ORIENTED_EDGE('',*,*,#14439,.T.);
#20042=ORIENTED_EDGE('',*,*,#14435,.T.);
#20043=ORIENTED_EDGE('',*,*,#14440,.T.);
#20044=ORIENTED_EDGE('',*,*,#14441,.F.);
#20045=ORIENTED_EDGE('',*,*,#14442,.T.);
#20046=ORIENTED_EDGE('',*,*,#14438,.T.);
#20047=ORIENTED_EDGE('',*,*,#14443,.T.);
#20048=ORIENTED_EDGE('',*,*,#14444,.F.);
#20049=ORIENTED_EDGE('',*,*,#14445,.T.);
#20050=ORIENTED_EDGE('',*,*,#14441,.T.);
#20051=ORIENTED_EDGE('',*,*,#14446,.T.);
#20052=ORIENTED_EDGE('',*,*,#14447,.F.);
#20053=ORIENTED_EDGE('',*,*,#14448,.T.);
#20054=ORIENTED_EDGE('',*,*,#14444,.T.);
#20055=ORIENTED_EDGE('',*,*,#14449,.T.);
#20056=ORIENTED_EDGE('',*,*,#14450,.F.);
#20057=ORIENTED_EDGE('',*,*,#14451,.T.);
#20058=ORIENTED_EDGE('',*,*,#14447,.T.);
#20059=ORIENTED_EDGE('',*,*,#14452,.T.);
#20060=ORIENTED_EDGE('',*,*,#14453,.F.);
#20061=ORIENTED_EDGE('',*,*,#14454,.T.);
#20062=ORIENTED_EDGE('',*,*,#14450,.T.);
#20063=ORIENTED_EDGE('',*,*,#14455,.T.);
#20064=ORIENTED_EDGE('',*,*,#14456,.F.);
#20065=ORIENTED_EDGE('',*,*,#14457,.T.);
#20066=ORIENTED_EDGE('',*,*,#14453,.T.);
#20067=ORIENTED_EDGE('',*,*,#14458,.T.);
#20068=ORIENTED_EDGE('',*,*,#14459,.F.);
#20069=ORIENTED_EDGE('',*,*,#14460,.T.);
#20070=ORIENTED_EDGE('',*,*,#14456,.T.);
#20071=ORIENTED_EDGE('',*,*,#14461,.T.);
#20072=ORIENTED_EDGE('',*,*,#14462,.F.);
#20073=ORIENTED_EDGE('',*,*,#14463,.T.);
#20074=ORIENTED_EDGE('',*,*,#14459,.T.);
#20075=ORIENTED_EDGE('',*,*,#14464,.T.);
#20076=ORIENTED_EDGE('',*,*,#14465,.F.);
#20077=ORIENTED_EDGE('',*,*,#14466,.T.);
#20078=ORIENTED_EDGE('',*,*,#14462,.T.);
#20079=ORIENTED_EDGE('',*,*,#14467,.T.);
#20080=ORIENTED_EDGE('',*,*,#14468,.F.);
#20081=ORIENTED_EDGE('',*,*,#14469,.T.);
#20082=ORIENTED_EDGE('',*,*,#14465,.T.);
#20083=ORIENTED_EDGE('',*,*,#14470,.T.);
#20084=ORIENTED_EDGE('',*,*,#14471,.F.);
#20085=ORIENTED_EDGE('',*,*,#14472,.T.);
#20086=ORIENTED_EDGE('',*,*,#14468,.T.);
#20087=ORIENTED_EDGE('',*,*,#14473,.T.);
#20088=ORIENTED_EDGE('',*,*,#14474,.F.);
#20089=ORIENTED_EDGE('',*,*,#14475,.T.);
#20090=ORIENTED_EDGE('',*,*,#14471,.T.);
#20091=ORIENTED_EDGE('',*,*,#14476,.T.);
#20092=ORIENTED_EDGE('',*,*,#14477,.F.);
#20093=ORIENTED_EDGE('',*,*,#14478,.T.);
#20094=ORIENTED_EDGE('',*,*,#14474,.T.);
#20095=ORIENTED_EDGE('',*,*,#14479,.T.);
#20096=ORIENTED_EDGE('',*,*,#14480,.F.);
#20097=ORIENTED_EDGE('',*,*,#14481,.T.);
#20098=ORIENTED_EDGE('',*,*,#14477,.T.);
#20099=ORIENTED_EDGE('',*,*,#14482,.T.);
#20100=ORIENTED_EDGE('',*,*,#14483,.F.);
#20101=ORIENTED_EDGE('',*,*,#14484,.T.);
#20102=ORIENTED_EDGE('',*,*,#14480,.T.);
#20103=ORIENTED_EDGE('',*,*,#14485,.T.);
#20104=ORIENTED_EDGE('',*,*,#14486,.F.);
#20105=ORIENTED_EDGE('',*,*,#14487,.T.);
#20106=ORIENTED_EDGE('',*,*,#14483,.T.);
#20107=ORIENTED_EDGE('',*,*,#14488,.T.);
#20108=ORIENTED_EDGE('',*,*,#14489,.F.);
#20109=ORIENTED_EDGE('',*,*,#14490,.T.);
#20110=ORIENTED_EDGE('',*,*,#14486,.T.);
#20111=ORIENTED_EDGE('',*,*,#14491,.T.);
#20112=ORIENTED_EDGE('',*,*,#14492,.F.);
#20113=ORIENTED_EDGE('',*,*,#14493,.T.);
#20114=ORIENTED_EDGE('',*,*,#14489,.T.);
#20115=ORIENTED_EDGE('',*,*,#14494,.T.);
#20116=ORIENTED_EDGE('',*,*,#14495,.F.);
#20117=ORIENTED_EDGE('',*,*,#14496,.T.);
#20118=ORIENTED_EDGE('',*,*,#14492,.T.);
#20119=ORIENTED_EDGE('',*,*,#14497,.T.);
#20120=ORIENTED_EDGE('',*,*,#14498,.F.);
#20121=ORIENTED_EDGE('',*,*,#14499,.T.);
#20122=ORIENTED_EDGE('',*,*,#14495,.T.);
#20123=ORIENTED_EDGE('',*,*,#14500,.T.);
#20124=ORIENTED_EDGE('',*,*,#14501,.F.);
#20125=ORIENTED_EDGE('',*,*,#14502,.T.);
#20126=ORIENTED_EDGE('',*,*,#14498,.T.);
#20127=ORIENTED_EDGE('',*,*,#14503,.T.);
#20128=ORIENTED_EDGE('',*,*,#14504,.F.);
#20129=ORIENTED_EDGE('',*,*,#14505,.T.);
#20130=ORIENTED_EDGE('',*,*,#14501,.T.);
#20131=ORIENTED_EDGE('',*,*,#14506,.T.);
#20132=ORIENTED_EDGE('',*,*,#14507,.F.);
#20133=ORIENTED_EDGE('',*,*,#14508,.T.);
#20134=ORIENTED_EDGE('',*,*,#14504,.T.);
#20135=ORIENTED_EDGE('',*,*,#14509,.T.);
#20136=ORIENTED_EDGE('',*,*,#14510,.F.);
#20137=ORIENTED_EDGE('',*,*,#14511,.T.);
#20138=ORIENTED_EDGE('',*,*,#14507,.T.);
#20139=ORIENTED_EDGE('',*,*,#14512,.T.);
#20140=ORIENTED_EDGE('',*,*,#14513,.F.);
#20141=ORIENTED_EDGE('',*,*,#14514,.T.);
#20142=ORIENTED_EDGE('',*,*,#14510,.T.);
#20143=ORIENTED_EDGE('',*,*,#14515,.T.);
#20144=ORIENTED_EDGE('',*,*,#14516,.F.);
#20145=ORIENTED_EDGE('',*,*,#14517,.T.);
#20146=ORIENTED_EDGE('',*,*,#14513,.T.);
#20147=ORIENTED_EDGE('',*,*,#14518,.T.);
#20148=ORIENTED_EDGE('',*,*,#14519,.F.);
#20149=ORIENTED_EDGE('',*,*,#14520,.T.);
#20150=ORIENTED_EDGE('',*,*,#14516,.T.);
#20151=ORIENTED_EDGE('',*,*,#14521,.T.);
#20152=ORIENTED_EDGE('',*,*,#14522,.F.);
#20153=ORIENTED_EDGE('',*,*,#14523,.T.);
#20154=ORIENTED_EDGE('',*,*,#14519,.T.);
#20155=ORIENTED_EDGE('',*,*,#14524,.T.);
#20156=ORIENTED_EDGE('',*,*,#14525,.F.);
#20157=ORIENTED_EDGE('',*,*,#14526,.T.);
#20158=ORIENTED_EDGE('',*,*,#14522,.T.);
#20159=ORIENTED_EDGE('',*,*,#14527,.T.);
#20160=ORIENTED_EDGE('',*,*,#14528,.F.);
#20161=ORIENTED_EDGE('',*,*,#14529,.T.);
#20162=ORIENTED_EDGE('',*,*,#14530,.F.);
#20163=ORIENTED_EDGE('',*,*,#14531,.F.);
#20164=ORIENTED_EDGE('',*,*,#14532,.T.);
#20165=ORIENTED_EDGE('',*,*,#14528,.T.);
#20166=ORIENTED_EDGE('',*,*,#14533,.F.);
#20167=ORIENTED_EDGE('',*,*,#14534,.F.);
#20168=ORIENTED_EDGE('',*,*,#14535,.F.);
#20169=ORIENTED_EDGE('',*,*,#14536,.T.);
#20170=ORIENTED_EDGE('',*,*,#14531,.T.);
#20171=ORIENTED_EDGE('',*,*,#14537,.F.);
#20172=ORIENTED_EDGE('',*,*,#14538,.F.);
#20173=ORIENTED_EDGE('',*,*,#14539,.T.);
#20174=ORIENTED_EDGE('',*,*,#14535,.T.);
#20175=ORIENTED_EDGE('',*,*,#14540,.F.);
#20176=ORIENTED_EDGE('',*,*,#14541,.F.);
#20177=ORIENTED_EDGE('',*,*,#14542,.T.);
#20178=ORIENTED_EDGE('',*,*,#14538,.T.);
#20179=ORIENTED_EDGE('',*,*,#14543,.F.);
#20180=ORIENTED_EDGE('',*,*,#14544,.F.);
#20181=ORIENTED_EDGE('',*,*,#14545,.T.);
#20182=ORIENTED_EDGE('',*,*,#14541,.T.);
#20183=ORIENTED_EDGE('',*,*,#14546,.F.);
#20184=ORIENTED_EDGE('',*,*,#14547,.F.);
#20185=ORIENTED_EDGE('',*,*,#14548,.T.);
#20186=ORIENTED_EDGE('',*,*,#14544,.T.);
#20187=ORIENTED_EDGE('',*,*,#14549,.F.);
#20188=ORIENTED_EDGE('',*,*,#14550,.F.);
#20189=ORIENTED_EDGE('',*,*,#14551,.T.);
#20190=ORIENTED_EDGE('',*,*,#14547,.T.);
#20191=ORIENTED_EDGE('',*,*,#14552,.F.);
#20192=ORIENTED_EDGE('',*,*,#14553,.F.);
#20193=ORIENTED_EDGE('',*,*,#14554,.T.);
#20194=ORIENTED_EDGE('',*,*,#14550,.T.);
#20195=ORIENTED_EDGE('',*,*,#14555,.F.);
#20196=ORIENTED_EDGE('',*,*,#14556,.F.);
#20197=ORIENTED_EDGE('',*,*,#14557,.T.);
#20198=ORIENTED_EDGE('',*,*,#14553,.T.);
#20199=ORIENTED_EDGE('',*,*,#14558,.F.);
#20200=ORIENTED_EDGE('',*,*,#14559,.F.);
#20201=ORIENTED_EDGE('',*,*,#14560,.T.);
#20202=ORIENTED_EDGE('',*,*,#14556,.T.);
#20203=ORIENTED_EDGE('',*,*,#14561,.F.);
#20204=ORIENTED_EDGE('',*,*,#14562,.F.);
#20205=ORIENTED_EDGE('',*,*,#14563,.T.);
#20206=ORIENTED_EDGE('',*,*,#14559,.T.);
#20207=ORIENTED_EDGE('',*,*,#14564,.F.);
#20208=ORIENTED_EDGE('',*,*,#14565,.F.);
#20209=ORIENTED_EDGE('',*,*,#14566,.T.);
#20210=ORIENTED_EDGE('',*,*,#14562,.T.);
#20211=ORIENTED_EDGE('',*,*,#14567,.F.);
#20212=ORIENTED_EDGE('',*,*,#14568,.F.);
#20213=ORIENTED_EDGE('',*,*,#14569,.T.);
#20214=ORIENTED_EDGE('',*,*,#14565,.T.);
#20215=ORIENTED_EDGE('',*,*,#14570,.F.);
#20216=ORIENTED_EDGE('',*,*,#14571,.F.);
#20217=ORIENTED_EDGE('',*,*,#14572,.T.);
#20218=ORIENTED_EDGE('',*,*,#14568,.T.);
#20219=ORIENTED_EDGE('',*,*,#14573,.F.);
#20220=ORIENTED_EDGE('',*,*,#14574,.F.);
#20221=ORIENTED_EDGE('',*,*,#14575,.T.);
#20222=ORIENTED_EDGE('',*,*,#14571,.T.);
#20223=ORIENTED_EDGE('',*,*,#14576,.F.);
#20224=ORIENTED_EDGE('',*,*,#14577,.F.);
#20225=ORIENTED_EDGE('',*,*,#14578,.T.);
#20226=ORIENTED_EDGE('',*,*,#14574,.T.);
#20227=ORIENTED_EDGE('',*,*,#14579,.F.);
#20228=ORIENTED_EDGE('',*,*,#14580,.F.);
#20229=ORIENTED_EDGE('',*,*,#14581,.T.);
#20230=ORIENTED_EDGE('',*,*,#14577,.T.);
#20231=ORIENTED_EDGE('',*,*,#14582,.F.);
#20232=ORIENTED_EDGE('',*,*,#14583,.F.);
#20233=ORIENTED_EDGE('',*,*,#14584,.T.);
#20234=ORIENTED_EDGE('',*,*,#14580,.T.);
#20235=ORIENTED_EDGE('',*,*,#14585,.F.);
#20236=ORIENTED_EDGE('',*,*,#14586,.F.);
#20237=ORIENTED_EDGE('',*,*,#14587,.T.);
#20238=ORIENTED_EDGE('',*,*,#14583,.T.);
#20239=ORIENTED_EDGE('',*,*,#14588,.F.);
#20240=ORIENTED_EDGE('',*,*,#14589,.F.);
#20241=ORIENTED_EDGE('',*,*,#14590,.T.);
#20242=ORIENTED_EDGE('',*,*,#14586,.T.);
#20243=ORIENTED_EDGE('',*,*,#14591,.F.);
#20244=ORIENTED_EDGE('',*,*,#14592,.F.);
#20245=ORIENTED_EDGE('',*,*,#14593,.T.);
#20246=ORIENTED_EDGE('',*,*,#14589,.T.);
#20247=ORIENTED_EDGE('',*,*,#14594,.F.);
#20248=ORIENTED_EDGE('',*,*,#14595,.F.);
#20249=ORIENTED_EDGE('',*,*,#14596,.T.);
#20250=ORIENTED_EDGE('',*,*,#14592,.T.);
#20251=ORIENTED_EDGE('',*,*,#14597,.F.);
#20252=ORIENTED_EDGE('',*,*,#14598,.F.);
#20253=ORIENTED_EDGE('',*,*,#14599,.T.);
#20254=ORIENTED_EDGE('',*,*,#14595,.T.);
#20255=ORIENTED_EDGE('',*,*,#14600,.F.);
#20256=ORIENTED_EDGE('',*,*,#14601,.F.);
#20257=ORIENTED_EDGE('',*,*,#14602,.T.);
#20258=ORIENTED_EDGE('',*,*,#14598,.T.);
#20259=ORIENTED_EDGE('',*,*,#14603,.F.);
#20260=ORIENTED_EDGE('',*,*,#14604,.F.);
#20261=ORIENTED_EDGE('',*,*,#14605,.T.);
#20262=ORIENTED_EDGE('',*,*,#14601,.T.);
#20263=ORIENTED_EDGE('',*,*,#14606,.F.);
#20264=ORIENTED_EDGE('',*,*,#14607,.F.);
#20265=ORIENTED_EDGE('',*,*,#14608,.T.);
#20266=ORIENTED_EDGE('',*,*,#14604,.T.);
#20267=ORIENTED_EDGE('',*,*,#14609,.F.);
#20268=ORIENTED_EDGE('',*,*,#14610,.F.);
#20269=ORIENTED_EDGE('',*,*,#14611,.T.);
#20270=ORIENTED_EDGE('',*,*,#14607,.T.);
#20271=ORIENTED_EDGE('',*,*,#14612,.F.);
#20272=ORIENTED_EDGE('',*,*,#14613,.F.);
#20273=ORIENTED_EDGE('',*,*,#14614,.T.);
#20274=ORIENTED_EDGE('',*,*,#14610,.T.);
#20275=ORIENTED_EDGE('',*,*,#14615,.F.);
#20276=ORIENTED_EDGE('',*,*,#14616,.F.);
#20277=ORIENTED_EDGE('',*,*,#14617,.T.);
#20278=ORIENTED_EDGE('',*,*,#14613,.T.);
#20279=ORIENTED_EDGE('',*,*,#14618,.F.);
#20280=ORIENTED_EDGE('',*,*,#14619,.F.);
#20281=ORIENTED_EDGE('',*,*,#14620,.T.);
#20282=ORIENTED_EDGE('',*,*,#14616,.T.);
#20283=ORIENTED_EDGE('',*,*,#14621,.F.);
#20284=ORIENTED_EDGE('',*,*,#14622,.F.);
#20285=ORIENTED_EDGE('',*,*,#14623,.T.);
#20286=ORIENTED_EDGE('',*,*,#14619,.T.);
#20287=ORIENTED_EDGE('',*,*,#14624,.F.);
#20288=ORIENTED_EDGE('',*,*,#14625,.F.);
#20289=ORIENTED_EDGE('',*,*,#14626,.T.);
#20290=ORIENTED_EDGE('',*,*,#14622,.T.);
#20291=ORIENTED_EDGE('',*,*,#14627,.F.);
#20292=ORIENTED_EDGE('',*,*,#14628,.F.);
#20293=ORIENTED_EDGE('',*,*,#14629,.T.);
#20294=ORIENTED_EDGE('',*,*,#14625,.T.);
#20295=ORIENTED_EDGE('',*,*,#14630,.F.);
#20296=ORIENTED_EDGE('',*,*,#14631,.F.);
#20297=ORIENTED_EDGE('',*,*,#14632,.T.);
#20298=ORIENTED_EDGE('',*,*,#14628,.T.);
#20299=ORIENTED_EDGE('',*,*,#14633,.F.);
#20300=ORIENTED_EDGE('',*,*,#14634,.F.);
#20301=ORIENTED_EDGE('',*,*,#14635,.T.);
#20302=ORIENTED_EDGE('',*,*,#14631,.T.);
#20303=ORIENTED_EDGE('',*,*,#14636,.F.);
#20304=ORIENTED_EDGE('',*,*,#14637,.F.);
#20305=ORIENTED_EDGE('',*,*,#14638,.T.);
#20306=ORIENTED_EDGE('',*,*,#14634,.T.);
#20307=ORIENTED_EDGE('',*,*,#14639,.F.);
#20308=ORIENTED_EDGE('',*,*,#14640,.F.);
#20309=ORIENTED_EDGE('',*,*,#14641,.T.);
#20310=ORIENTED_EDGE('',*,*,#14637,.T.);
#20311=ORIENTED_EDGE('',*,*,#14642,.F.);
#20312=ORIENTED_EDGE('',*,*,#14643,.F.);
#20313=ORIENTED_EDGE('',*,*,#14644,.T.);
#20314=ORIENTED_EDGE('',*,*,#14640,.T.);
#20315=ORIENTED_EDGE('',*,*,#14645,.F.);
#20316=ORIENTED_EDGE('',*,*,#14646,.F.);
#20317=ORIENTED_EDGE('',*,*,#14647,.T.);
#20318=ORIENTED_EDGE('',*,*,#14643,.T.);
#20319=ORIENTED_EDGE('',*,*,#14648,.F.);
#20320=ORIENTED_EDGE('',*,*,#14649,.F.);
#20321=ORIENTED_EDGE('',*,*,#14650,.T.);
#20322=ORIENTED_EDGE('',*,*,#14646,.T.);
#20323=ORIENTED_EDGE('',*,*,#14651,.F.);
#20324=ORIENTED_EDGE('',*,*,#14652,.F.);
#20325=ORIENTED_EDGE('',*,*,#14653,.T.);
#20326=ORIENTED_EDGE('',*,*,#14649,.T.);
#20327=ORIENTED_EDGE('',*,*,#14654,.F.);
#20328=ORIENTED_EDGE('',*,*,#14655,.F.);
#20329=ORIENTED_EDGE('',*,*,#14656,.T.);
#20330=ORIENTED_EDGE('',*,*,#14652,.T.);
#20331=ORIENTED_EDGE('',*,*,#14657,.F.);
#20332=ORIENTED_EDGE('',*,*,#14658,.F.);
#20333=ORIENTED_EDGE('',*,*,#14659,.T.);
#20334=ORIENTED_EDGE('',*,*,#14655,.T.);
#20335=ORIENTED_EDGE('',*,*,#14660,.F.);
#20336=ORIENTED_EDGE('',*,*,#14661,.F.);
#20337=ORIENTED_EDGE('',*,*,#14662,.T.);
#20338=ORIENTED_EDGE('',*,*,#14658,.T.);
#20339=ORIENTED_EDGE('',*,*,#14663,.F.);
#20340=ORIENTED_EDGE('',*,*,#14664,.F.);
#20341=ORIENTED_EDGE('',*,*,#14665,.T.);
#20342=ORIENTED_EDGE('',*,*,#14661,.T.);
#20343=ORIENTED_EDGE('',*,*,#14666,.F.);
#20344=ORIENTED_EDGE('',*,*,#14667,.F.);
#20345=ORIENTED_EDGE('',*,*,#14668,.T.);
#20346=ORIENTED_EDGE('',*,*,#14664,.T.);
#20347=ORIENTED_EDGE('',*,*,#14669,.F.);
#20348=ORIENTED_EDGE('',*,*,#14670,.F.);
#20349=ORIENTED_EDGE('',*,*,#14671,.T.);
#20350=ORIENTED_EDGE('',*,*,#14667,.T.);
#20351=ORIENTED_EDGE('',*,*,#14672,.F.);
#20352=ORIENTED_EDGE('',*,*,#14673,.F.);
#20353=ORIENTED_EDGE('',*,*,#14674,.T.);
#20354=ORIENTED_EDGE('',*,*,#14670,.T.);
#20355=ORIENTED_EDGE('',*,*,#14675,.F.);
#20356=ORIENTED_EDGE('',*,*,#14676,.F.);
#20357=ORIENTED_EDGE('',*,*,#14677,.T.);
#20358=ORIENTED_EDGE('',*,*,#14673,.T.);
#20359=ORIENTED_EDGE('',*,*,#14678,.F.);
#20360=ORIENTED_EDGE('',*,*,#14679,.F.);
#20361=ORIENTED_EDGE('',*,*,#14680,.T.);
#20362=ORIENTED_EDGE('',*,*,#14676,.T.);
#20363=ORIENTED_EDGE('',*,*,#14681,.F.);
#20364=ORIENTED_EDGE('',*,*,#14682,.F.);
#20365=ORIENTED_EDGE('',*,*,#14683,.T.);
#20366=ORIENTED_EDGE('',*,*,#14679,.T.);
#20367=ORIENTED_EDGE('',*,*,#14684,.F.);
#20368=ORIENTED_EDGE('',*,*,#14685,.F.);
#20369=ORIENTED_EDGE('',*,*,#14686,.T.);
#20370=ORIENTED_EDGE('',*,*,#14682,.T.);
#20371=ORIENTED_EDGE('',*,*,#14687,.F.);
#20372=ORIENTED_EDGE('',*,*,#14688,.F.);
#20373=ORIENTED_EDGE('',*,*,#14689,.T.);
#20374=ORIENTED_EDGE('',*,*,#14685,.T.);
#20375=ORIENTED_EDGE('',*,*,#14690,.F.);
#20376=ORIENTED_EDGE('',*,*,#14691,.F.);
#20377=ORIENTED_EDGE('',*,*,#14692,.T.);
#20378=ORIENTED_EDGE('',*,*,#14688,.T.);
#20379=ORIENTED_EDGE('',*,*,#14693,.F.);
#20380=ORIENTED_EDGE('',*,*,#14694,.F.);
#20381=ORIENTED_EDGE('',*,*,#14695,.T.);
#20382=ORIENTED_EDGE('',*,*,#14691,.T.);
#20383=ORIENTED_EDGE('',*,*,#14696,.F.);
#20384=ORIENTED_EDGE('',*,*,#14697,.F.);
#20385=ORIENTED_EDGE('',*,*,#14698,.T.);
#20386=ORIENTED_EDGE('',*,*,#14694,.T.);
#20387=ORIENTED_EDGE('',*,*,#14699,.F.);
#20388=ORIENTED_EDGE('',*,*,#14700,.F.);
#20389=ORIENTED_EDGE('',*,*,#14701,.T.);
#20390=ORIENTED_EDGE('',*,*,#14697,.T.);
#20391=ORIENTED_EDGE('',*,*,#14702,.F.);
#20392=ORIENTED_EDGE('',*,*,#14703,.F.);
#20393=ORIENTED_EDGE('',*,*,#14704,.T.);
#20394=ORIENTED_EDGE('',*,*,#14700,.T.);
#20395=ORIENTED_EDGE('',*,*,#14705,.F.);
#20396=ORIENTED_EDGE('',*,*,#14706,.F.);
#20397=ORIENTED_EDGE('',*,*,#14707,.T.);
#20398=ORIENTED_EDGE('',*,*,#14703,.T.);
#20399=ORIENTED_EDGE('',*,*,#14708,.F.);
#20400=ORIENTED_EDGE('',*,*,#14709,.F.);
#20401=ORIENTED_EDGE('',*,*,#14710,.T.);
#20402=ORIENTED_EDGE('',*,*,#14706,.T.);
#20403=ORIENTED_EDGE('',*,*,#14711,.F.);
#20404=ORIENTED_EDGE('',*,*,#14712,.F.);
#20405=ORIENTED_EDGE('',*,*,#14713,.T.);
#20406=ORIENTED_EDGE('',*,*,#14709,.T.);
#20407=ORIENTED_EDGE('',*,*,#14714,.F.);
#20408=ORIENTED_EDGE('',*,*,#14715,.F.);
#20409=ORIENTED_EDGE('',*,*,#14716,.T.);
#20410=ORIENTED_EDGE('',*,*,#14712,.T.);
#20411=ORIENTED_EDGE('',*,*,#14717,.F.);
#20412=ORIENTED_EDGE('',*,*,#14718,.T.);
#20413=ORIENTED_EDGE('',*,*,#14719,.T.);
#20414=ORIENTED_EDGE('',*,*,#14340,.F.);
#20415=ORIENTED_EDGE('',*,*,#14720,.T.);
#20416=ORIENTED_EDGE('',*,*,#14721,.T.);
#20417=ORIENTED_EDGE('',*,*,#14718,.F.);
#20418=ORIENTED_EDGE('',*,*,#14722,.T.);
#20419=ORIENTED_EDGE('',*,*,#14723,.T.);
#20420=ORIENTED_EDGE('',*,*,#14722,.F.);
#20421=ORIENTED_EDGE('',*,*,#14723,.F.);
#20422=ORIENTED_EDGE('',*,*,#14724,.F.);
#20423=ORIENTED_EDGE('',*,*,#14725,.F.);
#20424=ORIENTED_EDGE('',*,*,#14527,.F.);
#20425=ORIENTED_EDGE('',*,*,#14524,.F.);
#20426=ORIENTED_EDGE('',*,*,#14521,.F.);
#20427=ORIENTED_EDGE('',*,*,#14518,.F.);
#20428=ORIENTED_EDGE('',*,*,#14515,.F.);
#20429=ORIENTED_EDGE('',*,*,#14512,.F.);
#20430=ORIENTED_EDGE('',*,*,#14509,.F.);
#20431=ORIENTED_EDGE('',*,*,#14506,.F.);
#20432=ORIENTED_EDGE('',*,*,#14503,.F.);
#20433=ORIENTED_EDGE('',*,*,#14500,.F.);
#20434=ORIENTED_EDGE('',*,*,#14497,.F.);
#20435=ORIENTED_EDGE('',*,*,#14494,.F.);
#20436=ORIENTED_EDGE('',*,*,#14491,.F.);
#20437=ORIENTED_EDGE('',*,*,#14488,.F.);
#20438=ORIENTED_EDGE('',*,*,#14485,.F.);
#20439=ORIENTED_EDGE('',*,*,#14482,.F.);
#20440=ORIENTED_EDGE('',*,*,#14479,.F.);
#20441=ORIENTED_EDGE('',*,*,#14476,.F.);
#20442=ORIENTED_EDGE('',*,*,#14473,.F.);
#20443=ORIENTED_EDGE('',*,*,#14470,.F.);
#20444=ORIENTED_EDGE('',*,*,#14467,.F.);
#20445=ORIENTED_EDGE('',*,*,#14464,.F.);
#20446=ORIENTED_EDGE('',*,*,#14461,.F.);
#20447=ORIENTED_EDGE('',*,*,#14458,.F.);
#20448=ORIENTED_EDGE('',*,*,#14455,.F.);
#20449=ORIENTED_EDGE('',*,*,#14452,.F.);
#20450=ORIENTED_EDGE('',*,*,#14449,.F.);
#20451=ORIENTED_EDGE('',*,*,#14446,.F.);
#20452=ORIENTED_EDGE('',*,*,#14443,.F.);
#20453=ORIENTED_EDGE('',*,*,#14440,.F.);
#20454=ORIENTED_EDGE('',*,*,#14437,.F.);
#20455=ORIENTED_EDGE('',*,*,#14434,.F.);
#20456=ORIENTED_EDGE('',*,*,#14431,.F.);
#20457=ORIENTED_EDGE('',*,*,#14428,.F.);
#20458=ORIENTED_EDGE('',*,*,#14425,.F.);
#20459=ORIENTED_EDGE('',*,*,#14422,.F.);
#20460=ORIENTED_EDGE('',*,*,#14419,.F.);
#20461=ORIENTED_EDGE('',*,*,#14416,.F.);
#20462=ORIENTED_EDGE('',*,*,#14413,.F.);
#20463=ORIENTED_EDGE('',*,*,#14410,.F.);
#20464=ORIENTED_EDGE('',*,*,#14407,.F.);
#20465=ORIENTED_EDGE('',*,*,#14404,.F.);
#20466=ORIENTED_EDGE('',*,*,#14401,.F.);
#20467=ORIENTED_EDGE('',*,*,#14398,.F.);
#20468=ORIENTED_EDGE('',*,*,#14395,.F.);
#20469=ORIENTED_EDGE('',*,*,#14392,.F.);
#20470=ORIENTED_EDGE('',*,*,#14389,.F.);
#20471=ORIENTED_EDGE('',*,*,#14386,.F.);
#20472=ORIENTED_EDGE('',*,*,#14383,.F.);
#20473=ORIENTED_EDGE('',*,*,#14380,.F.);
#20474=ORIENTED_EDGE('',*,*,#14377,.F.);
#20475=ORIENTED_EDGE('',*,*,#14374,.F.);
#20476=ORIENTED_EDGE('',*,*,#14371,.F.);
#20477=ORIENTED_EDGE('',*,*,#14368,.F.);
#20478=ORIENTED_EDGE('',*,*,#14365,.F.);
#20479=ORIENTED_EDGE('',*,*,#14362,.F.);
#20480=ORIENTED_EDGE('',*,*,#14359,.F.);
#20481=ORIENTED_EDGE('',*,*,#14356,.F.);
#20482=ORIENTED_EDGE('',*,*,#14353,.F.);
#20483=ORIENTED_EDGE('',*,*,#14350,.F.);
#20484=ORIENTED_EDGE('',*,*,#14347,.F.);
#20485=ORIENTED_EDGE('',*,*,#14344,.F.);
#20486=ORIENTED_EDGE('',*,*,#14341,.F.);
#20487=ORIENTED_EDGE('',*,*,#14719,.F.);
#20488=ORIENTED_EDGE('',*,*,#14726,.T.);
#20489=ORIENTED_EDGE('',*,*,#14717,.T.);
#20490=ORIENTED_EDGE('',*,*,#14714,.T.);
#20491=ORIENTED_EDGE('',*,*,#14711,.T.);
#20492=ORIENTED_EDGE('',*,*,#14708,.T.);
#20493=ORIENTED_EDGE('',*,*,#14705,.T.);
#20494=ORIENTED_EDGE('',*,*,#14702,.T.);
#20495=ORIENTED_EDGE('',*,*,#14699,.T.);
#20496=ORIENTED_EDGE('',*,*,#14696,.T.);
#20497=ORIENTED_EDGE('',*,*,#14693,.T.);
#20498=ORIENTED_EDGE('',*,*,#14690,.T.);
#20499=ORIENTED_EDGE('',*,*,#14687,.T.);
#20500=ORIENTED_EDGE('',*,*,#14684,.T.);
#20501=ORIENTED_EDGE('',*,*,#14681,.T.);
#20502=ORIENTED_EDGE('',*,*,#14678,.T.);
#20503=ORIENTED_EDGE('',*,*,#14675,.T.);
#20504=ORIENTED_EDGE('',*,*,#14672,.T.);
#20505=ORIENTED_EDGE('',*,*,#14669,.T.);
#20506=ORIENTED_EDGE('',*,*,#14666,.T.);
#20507=ORIENTED_EDGE('',*,*,#14663,.T.);
#20508=ORIENTED_EDGE('',*,*,#14660,.T.);
#20509=ORIENTED_EDGE('',*,*,#14657,.T.);
#20510=ORIENTED_EDGE('',*,*,#14654,.T.);
#20511=ORIENTED_EDGE('',*,*,#14651,.T.);
#20512=ORIENTED_EDGE('',*,*,#14648,.T.);
#20513=ORIENTED_EDGE('',*,*,#14645,.T.);
#20514=ORIENTED_EDGE('',*,*,#14642,.T.);
#20515=ORIENTED_EDGE('',*,*,#14639,.T.);
#20516=ORIENTED_EDGE('',*,*,#14636,.T.);
#20517=ORIENTED_EDGE('',*,*,#14633,.T.);
#20518=ORIENTED_EDGE('',*,*,#14630,.T.);
#20519=ORIENTED_EDGE('',*,*,#14627,.T.);
#20520=ORIENTED_EDGE('',*,*,#14624,.T.);
#20521=ORIENTED_EDGE('',*,*,#14621,.T.);
#20522=ORIENTED_EDGE('',*,*,#14618,.T.);
#20523=ORIENTED_EDGE('',*,*,#14615,.T.);
#20524=ORIENTED_EDGE('',*,*,#14612,.T.);
#20525=ORIENTED_EDGE('',*,*,#14609,.T.);
#20526=ORIENTED_EDGE('',*,*,#14606,.T.);
#20527=ORIENTED_EDGE('',*,*,#14603,.T.);
#20528=ORIENTED_EDGE('',*,*,#14600,.T.);
#20529=ORIENTED_EDGE('',*,*,#14597,.T.);
#20530=ORIENTED_EDGE('',*,*,#14594,.T.);
#20531=ORIENTED_EDGE('',*,*,#14591,.T.);
#20532=ORIENTED_EDGE('',*,*,#14588,.T.);
#20533=ORIENTED_EDGE('',*,*,#14585,.T.);
#20534=ORIENTED_EDGE('',*,*,#14582,.T.);
#20535=ORIENTED_EDGE('',*,*,#14579,.T.);
#20536=ORIENTED_EDGE('',*,*,#14576,.T.);
#20537=ORIENTED_EDGE('',*,*,#14573,.T.);
#20538=ORIENTED_EDGE('',*,*,#14570,.T.);
#20539=ORIENTED_EDGE('',*,*,#14567,.T.);
#20540=ORIENTED_EDGE('',*,*,#14564,.T.);
#20541=ORIENTED_EDGE('',*,*,#14561,.T.);
#20542=ORIENTED_EDGE('',*,*,#14558,.T.);
#20543=ORIENTED_EDGE('',*,*,#14555,.T.);
#20544=ORIENTED_EDGE('',*,*,#14552,.T.);
#20545=ORIENTED_EDGE('',*,*,#14549,.T.);
#20546=ORIENTED_EDGE('',*,*,#14546,.T.);
#20547=ORIENTED_EDGE('',*,*,#14543,.T.);
#20548=ORIENTED_EDGE('',*,*,#14540,.T.);
#20549=ORIENTED_EDGE('',*,*,#14537,.T.);
#20550=ORIENTED_EDGE('',*,*,#14534,.T.);
#20551=ORIENTED_EDGE('',*,*,#14715,.T.);
#20552=ORIENTED_EDGE('',*,*,#14726,.F.);
#20553=ORIENTED_EDGE('',*,*,#14721,.F.);
#20554=ORIENTED_EDGE('',*,*,#14727,.T.);
#20555=ORIENTED_EDGE('',*,*,#14728,.F.);
#20556=ORIENTED_EDGE('',*,*,#14529,.F.);
#20557=ORIENTED_EDGE('',*,*,#14532,.F.);
#20558=ORIENTED_EDGE('',*,*,#14536,.F.);
#20559=ORIENTED_EDGE('',*,*,#14539,.F.);
#20560=ORIENTED_EDGE('',*,*,#14542,.F.);
#20561=ORIENTED_EDGE('',*,*,#14545,.F.);
#20562=ORIENTED_EDGE('',*,*,#14548,.F.);
#20563=ORIENTED_EDGE('',*,*,#14551,.F.);
#20564=ORIENTED_EDGE('',*,*,#14554,.F.);
#20565=ORIENTED_EDGE('',*,*,#14557,.F.);
#20566=ORIENTED_EDGE('',*,*,#14560,.F.);
#20567=ORIENTED_EDGE('',*,*,#14563,.F.);
#20568=ORIENTED_EDGE('',*,*,#14566,.F.);
#20569=ORIENTED_EDGE('',*,*,#14569,.F.);
#20570=ORIENTED_EDGE('',*,*,#14572,.F.);
#20571=ORIENTED_EDGE('',*,*,#14575,.F.);
#20572=ORIENTED_EDGE('',*,*,#14578,.F.);
#20573=ORIENTED_EDGE('',*,*,#14581,.F.);
#20574=ORIENTED_EDGE('',*,*,#14584,.F.);
#20575=ORIENTED_EDGE('',*,*,#14587,.F.);
#20576=ORIENTED_EDGE('',*,*,#14590,.F.);
#20577=ORIENTED_EDGE('',*,*,#14593,.F.);
#20578=ORIENTED_EDGE('',*,*,#14596,.F.);
#20579=ORIENTED_EDGE('',*,*,#14599,.F.);
#20580=ORIENTED_EDGE('',*,*,#14602,.F.);
#20581=ORIENTED_EDGE('',*,*,#14605,.F.);
#20582=ORIENTED_EDGE('',*,*,#14608,.F.);
#20583=ORIENTED_EDGE('',*,*,#14611,.F.);
#20584=ORIENTED_EDGE('',*,*,#14614,.F.);
#20585=ORIENTED_EDGE('',*,*,#14617,.F.);
#20586=ORIENTED_EDGE('',*,*,#14620,.F.);
#20587=ORIENTED_EDGE('',*,*,#14623,.F.);
#20588=ORIENTED_EDGE('',*,*,#14626,.F.);
#20589=ORIENTED_EDGE('',*,*,#14629,.F.);
#20590=ORIENTED_EDGE('',*,*,#14632,.F.);
#20591=ORIENTED_EDGE('',*,*,#14635,.F.);
#20592=ORIENTED_EDGE('',*,*,#14638,.F.);
#20593=ORIENTED_EDGE('',*,*,#14641,.F.);
#20594=ORIENTED_EDGE('',*,*,#14644,.F.);
#20595=ORIENTED_EDGE('',*,*,#14647,.F.);
#20596=ORIENTED_EDGE('',*,*,#14650,.F.);
#20597=ORIENTED_EDGE('',*,*,#14653,.F.);
#20598=ORIENTED_EDGE('',*,*,#14656,.F.);
#20599=ORIENTED_EDGE('',*,*,#14659,.F.);
#20600=ORIENTED_EDGE('',*,*,#14662,.F.);
#20601=ORIENTED_EDGE('',*,*,#14665,.F.);
#20602=ORIENTED_EDGE('',*,*,#14668,.F.);
#20603=ORIENTED_EDGE('',*,*,#14671,.F.);
#20604=ORIENTED_EDGE('',*,*,#14674,.F.);
#20605=ORIENTED_EDGE('',*,*,#14677,.F.);
#20606=ORIENTED_EDGE('',*,*,#14680,.F.);
#20607=ORIENTED_EDGE('',*,*,#14683,.F.);
#20608=ORIENTED_EDGE('',*,*,#14686,.F.);
#20609=ORIENTED_EDGE('',*,*,#14689,.F.);
#20610=ORIENTED_EDGE('',*,*,#14692,.F.);
#20611=ORIENTED_EDGE('',*,*,#14695,.F.);
#20612=ORIENTED_EDGE('',*,*,#14698,.F.);
#20613=ORIENTED_EDGE('',*,*,#14701,.F.);
#20614=ORIENTED_EDGE('',*,*,#14704,.F.);
#20615=ORIENTED_EDGE('',*,*,#14707,.F.);
#20616=ORIENTED_EDGE('',*,*,#14710,.F.);
#20617=ORIENTED_EDGE('',*,*,#14713,.F.);
#20618=ORIENTED_EDGE('',*,*,#14716,.F.);
#20619=ORIENTED_EDGE('',*,*,#14727,.F.);
#20620=ORIENTED_EDGE('',*,*,#14720,.F.);
#20621=ORIENTED_EDGE('',*,*,#14339,.F.);
#20622=ORIENTED_EDGE('',*,*,#14343,.F.);
#20623=ORIENTED_EDGE('',*,*,#14346,.F.);
#20624=ORIENTED_EDGE('',*,*,#14349,.F.);
#20625=ORIENTED_EDGE('',*,*,#14352,.F.);
#20626=ORIENTED_EDGE('',*,*,#14355,.F.);
#20627=ORIENTED_EDGE('',*,*,#14358,.F.);
#20628=ORIENTED_EDGE('',*,*,#14361,.F.);
#20629=ORIENTED_EDGE('',*,*,#14364,.F.);
#20630=ORIENTED_EDGE('',*,*,#14367,.F.);
#20631=ORIENTED_EDGE('',*,*,#14370,.F.);
#20632=ORIENTED_EDGE('',*,*,#14373,.F.);
#20633=ORIENTED_EDGE('',*,*,#14376,.F.);
#20634=ORIENTED_EDGE('',*,*,#14379,.F.);
#20635=ORIENTED_EDGE('',*,*,#14382,.F.);
#20636=ORIENTED_EDGE('',*,*,#14385,.F.);
#20637=ORIENTED_EDGE('',*,*,#14388,.F.);
#20638=ORIENTED_EDGE('',*,*,#14391,.F.);
#20639=ORIENTED_EDGE('',*,*,#14394,.F.);
#20640=ORIENTED_EDGE('',*,*,#14397,.F.);
#20641=ORIENTED_EDGE('',*,*,#14400,.F.);
#20642=ORIENTED_EDGE('',*,*,#14403,.F.);
#20643=ORIENTED_EDGE('',*,*,#14406,.F.);
#20644=ORIENTED_EDGE('',*,*,#14409,.F.);
#20645=ORIENTED_EDGE('',*,*,#14412,.F.);
#20646=ORIENTED_EDGE('',*,*,#14415,.F.);
#20647=ORIENTED_EDGE('',*,*,#14418,.F.);
#20648=ORIENTED_EDGE('',*,*,#14421,.F.);
#20649=ORIENTED_EDGE('',*,*,#14424,.F.);
#20650=ORIENTED_EDGE('',*,*,#14427,.F.);
#20651=ORIENTED_EDGE('',*,*,#14430,.F.);
#20652=ORIENTED_EDGE('',*,*,#14433,.F.);
#20653=ORIENTED_EDGE('',*,*,#14436,.F.);
#20654=ORIENTED_EDGE('',*,*,#14439,.F.);
#20655=ORIENTED_EDGE('',*,*,#14442,.F.);
#20656=ORIENTED_EDGE('',*,*,#14445,.F.);
#20657=ORIENTED_EDGE('',*,*,#14448,.F.);
#20658=ORIENTED_EDGE('',*,*,#14451,.F.);
#20659=ORIENTED_EDGE('',*,*,#14454,.F.);
#20660=ORIENTED_EDGE('',*,*,#14457,.F.);
#20661=ORIENTED_EDGE('',*,*,#14460,.F.);
#20662=ORIENTED_EDGE('',*,*,#14463,.F.);
#20663=ORIENTED_EDGE('',*,*,#14466,.F.);
#20664=ORIENTED_EDGE('',*,*,#14469,.F.);
#20665=ORIENTED_EDGE('',*,*,#14472,.F.);
#20666=ORIENTED_EDGE('',*,*,#14475,.F.);
#20667=ORIENTED_EDGE('',*,*,#14478,.F.);
#20668=ORIENTED_EDGE('',*,*,#14481,.F.);
#20669=ORIENTED_EDGE('',*,*,#14484,.F.);
#20670=ORIENTED_EDGE('',*,*,#14487,.F.);
#20671=ORIENTED_EDGE('',*,*,#14490,.F.);
#20672=ORIENTED_EDGE('',*,*,#14493,.F.);
#20673=ORIENTED_EDGE('',*,*,#14496,.F.);
#20674=ORIENTED_EDGE('',*,*,#14499,.F.);
#20675=ORIENTED_EDGE('',*,*,#14502,.F.);
#20676=ORIENTED_EDGE('',*,*,#14505,.F.);
#20677=ORIENTED_EDGE('',*,*,#14508,.F.);
#20678=ORIENTED_EDGE('',*,*,#14511,.F.);
#20679=ORIENTED_EDGE('',*,*,#14514,.F.);
#20680=ORIENTED_EDGE('',*,*,#14517,.F.);
#20681=ORIENTED_EDGE('',*,*,#14520,.F.);
#20682=ORIENTED_EDGE('',*,*,#14523,.F.);
#20683=ORIENTED_EDGE('',*,*,#14526,.F.);
#20684=ORIENTED_EDGE('',*,*,#14729,.F.);
#20685=ORIENTED_EDGE('',*,*,#14730,.F.);
#20686=ORIENTED_EDGE('',*,*,#14731,.T.);
#20687=ORIENTED_EDGE('',*,*,#14732,.F.);
#20688=ORIENTED_EDGE('',*,*,#14733,.F.);
#20689=ORIENTED_EDGE('',*,*,#14734,.F.);
#20690=ORIENTED_EDGE('',*,*,#14733,.T.);
#20691=ORIENTED_EDGE('',*,*,#14735,.T.);
#20692=ORIENTED_EDGE('',*,*,#14736,.T.);
#20693=ORIENTED_EDGE('',*,*,#14735,.F.);
#20694=ORIENTED_EDGE('',*,*,#14732,.T.);
#20695=ORIENTED_EDGE('',*,*,#14737,.T.);
#20696=ORIENTED_EDGE('',*,*,#14738,.F.);
#20697=ORIENTED_EDGE('',*,*,#14739,.F.);
#20698=ORIENTED_EDGE('',*,*,#14736,.F.);
#20699=ORIENTED_EDGE('',*,*,#14738,.T.);
#20700=ORIENTED_EDGE('',*,*,#14740,.T.);
#20701=ORIENTED_EDGE('',*,*,#14741,.F.);
#20702=ORIENTED_EDGE('',*,*,#14740,.F.);
#20703=ORIENTED_EDGE('',*,*,#14737,.F.);
#20704=ORIENTED_EDGE('',*,*,#14731,.F.);
#20705=ORIENTED_EDGE('',*,*,#14742,.F.);
#20706=ORIENTED_EDGE('',*,*,#14743,.T.);
#20707=ORIENTED_EDGE('',*,*,#14744,.F.);
#20708=ORIENTED_EDGE('',*,*,#14743,.F.);
#20709=ORIENTED_EDGE('',*,*,#14739,.T.);
#20710=ORIENTED_EDGE('',*,*,#14741,.T.);
#20711=ORIENTED_EDGE('',*,*,#14730,.T.);
#20712=ORIENTED_EDGE('',*,*,#14734,.T.);
#20713=ORIENTED_EDGE('',*,*,#14742,.T.);
#20714=ORIENTED_EDGE('',*,*,#14745,.F.);
#20715=ORIENTED_EDGE('',*,*,#14746,.T.);
#20716=ORIENTED_EDGE('',*,*,#14724,.T.);
#20717=ORIENTED_EDGE('',*,*,#14533,.T.);
#20718=ORIENTED_EDGE('',*,*,#14530,.T.);
#20719=ORIENTED_EDGE('',*,*,#14728,.T.);
#20720=ORIENTED_EDGE('',*,*,#14747,.F.);
#20721=ORIENTED_EDGE('',*,*,#14748,.T.);
#20722=ORIENTED_EDGE('',*,*,#14745,.T.);
#20723=ORIENTED_EDGE('',*,*,#14748,.F.);
#20724=ORIENTED_EDGE('',*,*,#14747,.T.);
#20725=ORIENTED_EDGE('',*,*,#14744,.T.);
#20726=ORIENTED_EDGE('',*,*,#14525,.T.);
#20727=ORIENTED_EDGE('',*,*,#14725,.T.);
#20728=ORIENTED_EDGE('',*,*,#14746,.F.);
#20729=ORIENTED_EDGE('',*,*,#14729,.T.);
#20730=ORIENTED_EDGE('',*,*,#14749,.F.);
#20731=ORIENTED_EDGE('',*,*,#14750,.T.);
#20732=ORIENTED_EDGE('',*,*,#14751,.T.);
#20733=ORIENTED_EDGE('',*,*,#14750,.F.);
#20734=ORIENTED_EDGE('',*,*,#14752,.F.);
#20735=ORIENTED_EDGE('',*,*,#14753,.T.);
#20736=ORIENTED_EDGE('',*,*,#14754,.T.);
#20737=ORIENTED_EDGE('',*,*,#14753,.F.);
#20738=ORIENTED_EDGE('',*,*,#14752,.T.);
#20739=ORIENTED_EDGE('',*,*,#14749,.T.);
#20740=ORIENTED_EDGE('',*,*,#14754,.F.);
#20741=ORIENTED_EDGE('',*,*,#14751,.F.);
#20742=ORIENTED_EDGE('',*,*,#14755,.F.);
#20743=ORIENTED_EDGE('',*,*,#14756,.T.);
#20744=ORIENTED_EDGE('',*,*,#14757,.F.);
#20745=ORIENTED_EDGE('',*,*,#14758,.F.);
#20746=ORIENTED_EDGE('',*,*,#14759,.F.);
#20747=ORIENTED_EDGE('',*,*,#14756,.F.);
#20748=ORIENTED_EDGE('',*,*,#14760,.F.);
#20749=ORIENTED_EDGE('',*,*,#14761,.T.);
#20750=ORIENTED_EDGE('',*,*,#14762,.F.);
#20751=ORIENTED_EDGE('',*,*,#14763,.F.);
#20752=ORIENTED_EDGE('',*,*,#14761,.F.);
#20753=ORIENTED_EDGE('',*,*,#14764,.F.);
#20754=ORIENTED_EDGE('',*,*,#14758,.T.);
#20755=ORIENTED_EDGE('',*,*,#14765,.F.);
#20756=ORIENTED_EDGE('',*,*,#14766,.T.);
#20757=ORIENTED_EDGE('',*,*,#14767,.T.);
#20758=ORIENTED_EDGE('',*,*,#14766,.F.);
#20759=ORIENTED_EDGE('',*,*,#14759,.T.);
#20760=ORIENTED_EDGE('',*,*,#14764,.T.);
#20761=ORIENTED_EDGE('',*,*,#14757,.T.);
#20762=ORIENTED_EDGE('',*,*,#14760,.T.);
#20763=ORIENTED_EDGE('',*,*,#14755,.T.);
#20764=ORIENTED_EDGE('',*,*,#14768,.F.);
#20765=ORIENTED_EDGE('',*,*,#14769,.T.);
#20766=ORIENTED_EDGE('',*,*,#14770,.T.);
#20767=ORIENTED_EDGE('',*,*,#14769,.F.);
#20768=ORIENTED_EDGE('',*,*,#14762,.T.);
#20769=ORIENTED_EDGE('',*,*,#14763,.T.);
#20770=ORIENTED_EDGE('',*,*,#14768,.T.);
#20771=ORIENTED_EDGE('',*,*,#14765,.T.);
#20772=ORIENTED_EDGE('',*,*,#14770,.F.);
#20773=ORIENTED_EDGE('',*,*,#14767,.F.);
#20774=ORIENTED_EDGE('',*,*,#14771,.F.);
#20775=ORIENTED_EDGE('',*,*,#14772,.T.);
#20776=ORIENTED_EDGE('',*,*,#14773,.F.);
#20777=ORIENTED_EDGE('',*,*,#14772,.F.);
#20778=ORIENTED_EDGE('',*,*,#14774,.F.);
#20779=ORIENTED_EDGE('',*,*,#14775,.T.);
#20780=ORIENTED_EDGE('',*,*,#14776,.F.);
#20781=ORIENTED_EDGE('',*,*,#14777,.F.);
#20782=ORIENTED_EDGE('',*,*,#14778,.F.);
#20783=ORIENTED_EDGE('',*,*,#14775,.F.);
#20784=ORIENTED_EDGE('',*,*,#14779,.F.);
#20785=ORIENTED_EDGE('',*,*,#14780,.T.);
#20786=ORIENTED_EDGE('',*,*,#14781,.F.);
#20787=ORIENTED_EDGE('',*,*,#14782,.F.);
#20788=ORIENTED_EDGE('',*,*,#14780,.F.);
#20789=ORIENTED_EDGE('',*,*,#14783,.F.);
#20790=ORIENTED_EDGE('',*,*,#14777,.T.);
#20791=ORIENTED_EDGE('',*,*,#14784,.F.);
#20792=ORIENTED_EDGE('',*,*,#14785,.F.);
#20793=ORIENTED_EDGE('',*,*,#14786,.F.);
#20794=ORIENTED_EDGE('',*,*,#14787,.F.);
#20795=ORIENTED_EDGE('',*,*,#14788,.F.);
#20796=ORIENTED_EDGE('',*,*,#14789,.F.);
#20797=ORIENTED_EDGE('',*,*,#14790,.F.);
#20798=ORIENTED_EDGE('',*,*,#14791,.F.);
#20799=ORIENTED_EDGE('',*,*,#14792,.F.);
#20800=ORIENTED_EDGE('',*,*,#14785,.T.);
#20801=ORIENTED_EDGE('',*,*,#14793,.F.);
#20802=ORIENTED_EDGE('',*,*,#14794,.F.);
#20803=ORIENTED_EDGE('',*,*,#14795,.F.);
#20804=ORIENTED_EDGE('',*,*,#14796,.F.);
#20805=ORIENTED_EDGE('',*,*,#14797,.F.);
#20806=ORIENTED_EDGE('',*,*,#14791,.T.);
#20807=ORIENTED_EDGE('',*,*,#14798,.T.);
#20808=ORIENTED_EDGE('',*,*,#14773,.T.);
#20809=ORIENTED_EDGE('',*,*,#14793,.T.);
#20810=ORIENTED_EDGE('',*,*,#14790,.T.);
#20811=ORIENTED_EDGE('',*,*,#14784,.T.);
#20812=ORIENTED_EDGE('',*,*,#14799,.T.);
#20813=ORIENTED_EDGE('',*,*,#14800,.F.);
#20814=ORIENTED_EDGE('',*,*,#14771,.T.);
#20815=ORIENTED_EDGE('',*,*,#14797,.T.);
#20816=ORIENTED_EDGE('',*,*,#14801,.T.);
#20817=ORIENTED_EDGE('',*,*,#14786,.T.);
#20818=ORIENTED_EDGE('',*,*,#14792,.T.);
#20819=ORIENTED_EDGE('',*,*,#14798,.F.);
#20820=ORIENTED_EDGE('',*,*,#14802,.T.);
#20821=ORIENTED_EDGE('',*,*,#14800,.T.);
#20822=ORIENTED_EDGE('',*,*,#14802,.F.);
#20823=ORIENTED_EDGE('',*,*,#14794,.T.);
#20824=ORIENTED_EDGE('',*,*,#14799,.F.);
#20825=ORIENTED_EDGE('',*,*,#14789,.T.);
#20826=ORIENTED_EDGE('',*,*,#14803,.T.);
#20827=ORIENTED_EDGE('',*,*,#14778,.T.);
#20828=ORIENTED_EDGE('',*,*,#14783,.T.);
#20829=ORIENTED_EDGE('',*,*,#14776,.T.);
#20830=ORIENTED_EDGE('',*,*,#14779,.T.);
#20831=ORIENTED_EDGE('',*,*,#14774,.T.);
#20832=ORIENTED_EDGE('',*,*,#14796,.T.);
#20833=ORIENTED_EDGE('',*,*,#14804,.T.);
#20834=ORIENTED_EDGE('',*,*,#14787,.T.);
#20835=ORIENTED_EDGE('',*,*,#14801,.F.);
#20836=ORIENTED_EDGE('',*,*,#14781,.T.);
#20837=ORIENTED_EDGE('',*,*,#14782,.T.);
#20838=ORIENTED_EDGE('',*,*,#14795,.T.);
#20839=ORIENTED_EDGE('',*,*,#14803,.F.);
#20840=ORIENTED_EDGE('',*,*,#14788,.T.);
#20841=ORIENTED_EDGE('',*,*,#14804,.F.);
#20842=ORIENTED_EDGE('',*,*,#14805,.F.);
#20843=ORIENTED_EDGE('',*,*,#14806,.T.);
#20844=ORIENTED_EDGE('',*,*,#14807,.T.);
#20845=ORIENTED_EDGE('',*,*,#14806,.F.);
#20846=ORIENTED_EDGE('',*,*,#14808,.F.);
#20847=ORIENTED_EDGE('',*,*,#14809,.T.);
#20848=ORIENTED_EDGE('',*,*,#14810,.T.);
#20849=ORIENTED_EDGE('',*,*,#14809,.F.);
#20850=ORIENTED_EDGE('',*,*,#14808,.T.);
#20851=ORIENTED_EDGE('',*,*,#14805,.T.);
#20852=ORIENTED_EDGE('',*,*,#14810,.F.);
#20853=ORIENTED_EDGE('',*,*,#14807,.F.);
#20854=ORIENTED_EDGE('',*,*,#14811,.F.);
#20855=ORIENTED_EDGE('',*,*,#14812,.T.);
#20856=ORIENTED_EDGE('',*,*,#14813,.T.);
#20857=ORIENTED_EDGE('',*,*,#14812,.F.);
#20858=ORIENTED_EDGE('',*,*,#14814,.F.);
#20859=ORIENTED_EDGE('',*,*,#14815,.T.);
#20860=ORIENTED_EDGE('',*,*,#14816,.T.);
#20861=ORIENTED_EDGE('',*,*,#14815,.F.);
#20862=ORIENTED_EDGE('',*,*,#14814,.T.);
#20863=ORIENTED_EDGE('',*,*,#14811,.T.);
#20864=ORIENTED_EDGE('',*,*,#14816,.F.);
#20865=ORIENTED_EDGE('',*,*,#14813,.F.);
#20866=ORIENTED_EDGE('',*,*,#14817,.F.);
#20867=ORIENTED_EDGE('',*,*,#14818,.F.);
#20868=ORIENTED_EDGE('',*,*,#14819,.F.);
#20869=ORIENTED_EDGE('',*,*,#14820,.F.);
#20870=ORIENTED_EDGE('',*,*,#14821,.F.);
#20871=ORIENTED_EDGE('',*,*,#14822,.F.);
#20872=ORIENTED_EDGE('',*,*,#14823,.F.);
#20873=ORIENTED_EDGE('',*,*,#14824,.F.);
#20874=ORIENTED_EDGE('',*,*,#14821,.T.);
#20875=ORIENTED_EDGE('',*,*,#14825,.T.);
#20876=ORIENTED_EDGE('',*,*,#14826,.T.);
#20877=ORIENTED_EDGE('',*,*,#14827,.T.);
#20878=ORIENTED_EDGE('',*,*,#14820,.T.);
#20879=ORIENTED_EDGE('',*,*,#14828,.F.);
#20880=ORIENTED_EDGE('',*,*,#14829,.T.);
#20881=ORIENTED_EDGE('',*,*,#14825,.F.);
#20882=ORIENTED_EDGE('',*,*,#14819,.T.);
#20883=ORIENTED_EDGE('',*,*,#14830,.T.);
#20884=ORIENTED_EDGE('',*,*,#14831,.T.);
#20885=ORIENTED_EDGE('',*,*,#14828,.T.);
#20886=ORIENTED_EDGE('',*,*,#14818,.T.);
#20887=ORIENTED_EDGE('',*,*,#14832,.F.);
#20888=ORIENTED_EDGE('',*,*,#14833,.T.);
#20889=ORIENTED_EDGE('',*,*,#14830,.F.);
#20890=ORIENTED_EDGE('',*,*,#14834,.F.);
#20891=ORIENTED_EDGE('',*,*,#14835,.F.);
#20892=ORIENTED_EDGE('',*,*,#14826,.F.);
#20893=ORIENTED_EDGE('',*,*,#14829,.F.);
#20894=ORIENTED_EDGE('',*,*,#14831,.F.);
#20895=ORIENTED_EDGE('',*,*,#14833,.F.);
#20896=ORIENTED_EDGE('',*,*,#14836,.F.);
#20897=ORIENTED_EDGE('',*,*,#14837,.F.);
#20898=ORIENTED_EDGE('',*,*,#14822,.T.);
#20899=ORIENTED_EDGE('',*,*,#14827,.F.);
#20900=ORIENTED_EDGE('',*,*,#14835,.T.);
#20901=ORIENTED_EDGE('',*,*,#14838,.F.);
#20902=ORIENTED_EDGE('',*,*,#14817,.T.);
#20903=ORIENTED_EDGE('',*,*,#14839,.T.);
#20904=ORIENTED_EDGE('',*,*,#14836,.T.);
#20905=ORIENTED_EDGE('',*,*,#14832,.T.);
#20906=ORIENTED_EDGE('',*,*,#14823,.T.);
#20907=ORIENTED_EDGE('',*,*,#14838,.T.);
#20908=ORIENTED_EDGE('',*,*,#14834,.T.);
#20909=ORIENTED_EDGE('',*,*,#14840,.T.);
#20910=ORIENTED_EDGE('',*,*,#14824,.T.);
#20911=ORIENTED_EDGE('',*,*,#14840,.F.);
#20912=ORIENTED_EDGE('',*,*,#14837,.T.);
#20913=ORIENTED_EDGE('',*,*,#14839,.F.);
#20914=ORIENTED_EDGE('',*,*,#14841,.F.);
#20915=ORIENTED_EDGE('',*,*,#14842,.T.);
#20916=ORIENTED_EDGE('',*,*,#14843,.T.);
#20917=ORIENTED_EDGE('',*,*,#14844,.F.);
#20918=ORIENTED_EDGE('',*,*,#14845,.F.);
#20919=ORIENTED_EDGE('',*,*,#14846,.T.);
#20920=ORIENTED_EDGE('',*,*,#14847,.T.);
#20921=ORIENTED_EDGE('',*,*,#14842,.F.);
#20922=ORIENTED_EDGE('',*,*,#14848,.F.);
#20923=ORIENTED_EDGE('',*,*,#14849,.T.);
#20924=ORIENTED_EDGE('',*,*,#14850,.T.);
#20925=ORIENTED_EDGE('',*,*,#14846,.F.);
#20926=ORIENTED_EDGE('',*,*,#14851,.F.);
#20927=ORIENTED_EDGE('',*,*,#14852,.T.);
#20928=ORIENTED_EDGE('',*,*,#14853,.T.);
#20929=ORIENTED_EDGE('',*,*,#14849,.F.);
#20930=ORIENTED_EDGE('',*,*,#14854,.F.);
#20931=ORIENTED_EDGE('',*,*,#14855,.T.);
#20932=ORIENTED_EDGE('',*,*,#14856,.T.);
#20933=ORIENTED_EDGE('',*,*,#14852,.F.);
#20934=ORIENTED_EDGE('',*,*,#14857,.F.);
#20935=ORIENTED_EDGE('',*,*,#14844,.T.);
#20936=ORIENTED_EDGE('',*,*,#14858,.T.);
#20937=ORIENTED_EDGE('',*,*,#14855,.F.);
#20938=ORIENTED_EDGE('',*,*,#14858,.F.);
#20939=ORIENTED_EDGE('',*,*,#14843,.F.);
#20940=ORIENTED_EDGE('',*,*,#14847,.F.);
#20941=ORIENTED_EDGE('',*,*,#14850,.F.);
#20942=ORIENTED_EDGE('',*,*,#14853,.F.);
#20943=ORIENTED_EDGE('',*,*,#14856,.F.);
#20944=ORIENTED_EDGE('',*,*,#14859,.F.);
#20945=ORIENTED_EDGE('',*,*,#14841,.T.);
#20946=ORIENTED_EDGE('',*,*,#14857,.T.);
#20947=ORIENTED_EDGE('',*,*,#14854,.T.);
#20948=ORIENTED_EDGE('',*,*,#14851,.T.);
#20949=ORIENTED_EDGE('',*,*,#14848,.T.);
#20950=ORIENTED_EDGE('',*,*,#14845,.T.);
#20951=ORIENTED_EDGE('',*,*,#14860,.F.);
#20952=ORIENTED_EDGE('',*,*,#14861,.T.);
#20953=ORIENTED_EDGE('',*,*,#14859,.T.);
#20954=ORIENTED_EDGE('',*,*,#14861,.F.);
#20955=ORIENTED_EDGE('',*,*,#14862,.F.);
#20956=ORIENTED_EDGE('',*,*,#14863,.T.);
#20957=ORIENTED_EDGE('',*,*,#14860,.T.);
#20958=ORIENTED_EDGE('',*,*,#14863,.F.);
#20959=ORIENTED_EDGE('',*,*,#14864,.F.);
#20960=ORIENTED_EDGE('',*,*,#14865,.T.);
#20961=ORIENTED_EDGE('',*,*,#14862,.T.);
#20962=ORIENTED_EDGE('',*,*,#14865,.F.);
#20963=ORIENTED_EDGE('',*,*,#14864,.T.);
#20964=ORIENTED_EDGE('',*,*,#14866,.F.);
#20965=ORIENTED_EDGE('',*,*,#14867,.T.);
#20966=ORIENTED_EDGE('',*,*,#14868,.T.);
#20967=ORIENTED_EDGE('',*,*,#14867,.F.);
#20968=ORIENTED_EDGE('',*,*,#14869,.F.);
#20969=ORIENTED_EDGE('',*,*,#14870,.T.);
#20970=ORIENTED_EDGE('',*,*,#14871,.T.);
#20971=ORIENTED_EDGE('',*,*,#14870,.F.);
#20972=ORIENTED_EDGE('',*,*,#14869,.T.);
#20973=ORIENTED_EDGE('',*,*,#14866,.T.);
#20974=ORIENTED_EDGE('',*,*,#14871,.F.);
#20975=ORIENTED_EDGE('',*,*,#14868,.F.);
#20976=ORIENTED_EDGE('',*,*,#14872,.F.);
#20977=ORIENTED_EDGE('',*,*,#14873,.F.);
#20978=ORIENTED_EDGE('',*,*,#14874,.T.);
#20979=ORIENTED_EDGE('',*,*,#14872,.T.);
#20980=ORIENTED_EDGE('',*,*,#14874,.F.);
#20981=ORIENTED_EDGE('',*,*,#14875,.F.);
#20982=ORIENTED_EDGE('',*,*,#14876,.T.);
#20983=ORIENTED_EDGE('',*,*,#14873,.T.);
#20984=ORIENTED_EDGE('',*,*,#14876,.F.);
#20985=ORIENTED_EDGE('',*,*,#14877,.F.);
#20986=ORIENTED_EDGE('',*,*,#14878,.T.);
#20987=ORIENTED_EDGE('',*,*,#14875,.T.);
#20988=ORIENTED_EDGE('',*,*,#14878,.F.);
#20989=ORIENTED_EDGE('',*,*,#14877,.T.);
#20990=ORIENTED_EDGE('',*,*,#14879,.F.);
#20991=ORIENTED_EDGE('',*,*,#14880,.F.);
#20992=ORIENTED_EDGE('',*,*,#14881,.T.);
#20993=ORIENTED_EDGE('',*,*,#14879,.T.);
#20994=ORIENTED_EDGE('',*,*,#14881,.F.);
#20995=ORIENTED_EDGE('',*,*,#14882,.F.);
#20996=ORIENTED_EDGE('',*,*,#14883,.T.);
#20997=ORIENTED_EDGE('',*,*,#14880,.T.);
#20998=ORIENTED_EDGE('',*,*,#14883,.F.);
#20999=ORIENTED_EDGE('',*,*,#14884,.F.);
#21000=ORIENTED_EDGE('',*,*,#14885,.T.);
#21001=ORIENTED_EDGE('',*,*,#14882,.T.);
#21002=ORIENTED_EDGE('',*,*,#14885,.F.);
#21003=ORIENTED_EDGE('',*,*,#14884,.T.);
#21004=ORIENTED_EDGE('',*,*,#14886,.T.);
#21005=ORIENTED_EDGE('',*,*,#14887,.T.);
#21006=ORIENTED_EDGE('',*,*,#14888,.T.);
#21007=ORIENTED_EDGE('',*,*,#14889,.F.);
#21008=ORIENTED_EDGE('',*,*,#14890,.T.);
#21009=ORIENTED_EDGE('',*,*,#14891,.T.);
#21010=ORIENTED_EDGE('',*,*,#14892,.T.);
#21011=ORIENTED_EDGE('',*,*,#14887,.F.);
#21012=ORIENTED_EDGE('',*,*,#14893,.T.);
#21013=ORIENTED_EDGE('',*,*,#14894,.T.);
#21014=ORIENTED_EDGE('',*,*,#14895,.T.);
#21015=ORIENTED_EDGE('',*,*,#14891,.F.);
#21016=ORIENTED_EDGE('',*,*,#14896,.T.);
#21017=ORIENTED_EDGE('',*,*,#14897,.T.);
#21018=ORIENTED_EDGE('',*,*,#14898,.T.);
#21019=ORIENTED_EDGE('',*,*,#14894,.F.);
#21020=ORIENTED_EDGE('',*,*,#14899,.T.);
#21021=ORIENTED_EDGE('',*,*,#14900,.T.);
#21022=ORIENTED_EDGE('',*,*,#14901,.T.);
#21023=ORIENTED_EDGE('',*,*,#14897,.F.);
#21024=ORIENTED_EDGE('',*,*,#14902,.T.);
#21025=ORIENTED_EDGE('',*,*,#14889,.T.);
#21026=ORIENTED_EDGE('',*,*,#14903,.T.);
#21027=ORIENTED_EDGE('',*,*,#14900,.F.);
#21028=ORIENTED_EDGE('',*,*,#14902,.F.);
#21029=ORIENTED_EDGE('',*,*,#14899,.F.);
#21030=ORIENTED_EDGE('',*,*,#14896,.F.);
#21031=ORIENTED_EDGE('',*,*,#14893,.F.);
#21032=ORIENTED_EDGE('',*,*,#14890,.F.);
#21033=ORIENTED_EDGE('',*,*,#14886,.F.);
#21034=ORIENTED_EDGE('',*,*,#14903,.F.);
#21035=ORIENTED_EDGE('',*,*,#14888,.F.);
#21036=ORIENTED_EDGE('',*,*,#14892,.F.);
#21037=ORIENTED_EDGE('',*,*,#14895,.F.);
#21038=ORIENTED_EDGE('',*,*,#14898,.F.);
#21039=ORIENTED_EDGE('',*,*,#14901,.F.);
#21040=CYLINDRICAL_SURFACE('',#24004,0.210000000000001);
#21041=CYLINDRICAL_SURFACE('',#24007,0.21);
#21042=CYLINDRICAL_SURFACE('',#24010,0.329999999999998);
#21043=CYLINDRICAL_SURFACE('',#24013,0.329999999999998);
#21044=CYLINDRICAL_SURFACE('',#24016,0.275);
#21045=CYLINDRICAL_SURFACE('',#24019,0.275);
#21046=CYLINDRICAL_SURFACE('',#24022,0.210000000000001);
#21047=CYLINDRICAL_SURFACE('',#24025,0.21);
#21048=CYLINDRICAL_SURFACE('',#24028,0.21);
#21049=CYLINDRICAL_SURFACE('',#24031,0.210000000000001);
#21050=CYLINDRICAL_SURFACE('',#24055,0.5);
#21051=CYLINDRICAL_SURFACE('',#24058,0.5);
#21052=CYLINDRICAL_SURFACE('',#24061,0.164999999999999);
#21053=CYLINDRICAL_SURFACE('',#24064,0.164999999999999);
#21054=CYLINDRICAL_SURFACE('',#24067,0.165);
#21055=CYLINDRICAL_SURFACE('',#24070,0.164999999999999);
#21056=CYLINDRICAL_SURFACE('',#24073,0.5);
#21057=CYLINDRICAL_SURFACE('',#24078,0.5);
#21058=CYLINDRICAL_SURFACE('',#24083,0.5);
#21059=CYLINDRICAL_SURFACE('',#24088,0.5);
#21060=CYLINDRICAL_SURFACE('',#24094,0.274999999999999);
#21061=CYLINDRICAL_SURFACE('',#24096,0.275);
#21062=CYLINDRICAL_SURFACE('',#24098,0.275);
#21063=CYLINDRICAL_SURFACE('',#24100,0.274999999999999);
#21064=CYLINDRICAL_SURFACE('',#24108,0.165);
#21065=CYLINDRICAL_SURFACE('',#24111,0.165);
#21066=CYLINDRICAL_SURFACE('',#24114,0.165);
#21067=CYLINDRICAL_SURFACE('',#24117,1.6);
#21068=CYLINDRICAL_SURFACE('',#24122,1.4);
#21069=CYLINDRICAL_SURFACE('',#24124,0.21);
#21070=CYLINDRICAL_SURFACE('',#24128,0.21);
#21071=CYLINDRICAL_SURFACE('',#24139,0.225);
#21072=CYLINDRICAL_SURFACE('',#24142,0.225);
#21073=CYLINDRICAL_SURFACE('',#24145,0.225);
#21074=CYLINDRICAL_SURFACE('',#24148,1.59);
#21075=CYLINDRICAL_SURFACE('',#24153,1.2);
#21076=CYLINDRICAL_SURFACE('',#24155,2.4);
#21077=CYLINDRICAL_SURFACE('',#24161,0.165);
#21078=CYLINDRICAL_SURFACE('',#24164,0.165);
#21079=CYLINDRICAL_SURFACE('',#24167,0.165);
#21080=CYLINDRICAL_SURFACE('',#24170,2.35);
#21081=CYLINDRICAL_SURFACE('',#24175,2.15);
#21082=CYLINDRICAL_SURFACE('',#24177,0.25);
#21083=CYLINDRICAL_SURFACE('',#24181,0.25);
#21084=CYLINDRICAL_SURFACE('',#24192,0.225);
#21085=CYLINDRICAL_SURFACE('',#24195,0.225);
#21086=CYLINDRICAL_SURFACE('',#24198,0.225);
#21087=CYLINDRICAL_SURFACE('',#24205,3.);
#21088=CYLINDRICAL_SURFACE('',#24207,2.34);
#21089=CYLINDRICAL_SURFACE('',#24211,1.8);
#21090=CYLINDRICAL_SURFACE('',#24215,0.475);
#21091=CYLINDRICAL_SURFACE('',#24220,0.275);
#21092=CYLINDRICAL_SURFACE('',#24229,0.475000000000001);
#21093=CYLINDRICAL_SURFACE('',#24234,0.274999999999999);
#21094=CYLINDRICAL_SURFACE('',#24243,0.375);
#21095=CYLINDRICAL_SURFACE('',#24248,0.375);
#21096=CYLINDRICAL_SURFACE('',#24253,0.375);
#21097=CYLINDRICAL_SURFACE('',#24258,0.375);
#21098=CYLINDRICAL_SURFACE('',#24263,0.225);
#21099=CYLINDRICAL_SURFACE('',#24265,0.225);
#21100=CYLINDRICAL_SURFACE('',#24267,0.225);
#21101=CYLINDRICAL_SURFACE('',#24269,0.225000000000001);
#21102=CYLINDRICAL_SURFACE('',#24293,1.070235);
#21103=CYLINDRICAL_SURFACE('',#24295,0.6);
#21104=CYLINDRICAL_SURFACE('',#24301,1.070235);
#21105=CYLINDRICAL_SURFACE('',#24313,1.129765);
#21106=CYLINDRICAL_SURFACE('',#24320,1.6);
#21107=CYLINDRICAL_SURFACE('',#24325,1.129765);
#21108=CYLINDRICAL_SURFACE('',#24345,1.123812);
#21109=CYLINDRICAL_SURFACE('',#24381,1.076188);
#21110=CYLINDRICAL_SURFACE('',#24395,1.119765);
#21111=CYLINDRICAL_SURFACE('',#24399,1.085235);
#21112=CYLINDRICAL_SURFACE('',#24403,1.119765);
#21113=CYLINDRICAL_SURFACE('',#24407,1.085235);
#21114=CYLINDRICAL_SURFACE('',#24421,1.63531);
#21115=CYLINDRICAL_SURFACE('',#24423,1.);
#21116=CYLINDRICAL_SURFACE('',#24429,1.63531);
#21117=CYLINDRICAL_SURFACE('',#24441,1.71469);
#21118=CYLINDRICAL_SURFACE('',#24448,2.35);
#21119=CYLINDRICAL_SURFACE('',#24453,1.71469);
#21120=CYLINDRICAL_SURFACE('',#24475,1.706752);
#21121=CYLINDRICAL_SURFACE('',#24515,1.643248);
#21122=CYLINDRICAL_SURFACE('',#24529,1.70469);
#21123=CYLINDRICAL_SURFACE('',#24533,1.65031);
#21124=CYLINDRICAL_SURFACE('',#24537,1.70469);
#21125=CYLINDRICAL_SURFACE('',#24541,1.65031);
#21126=CYLINDRICAL_SURFACE('',#24549,0.275);
#21127=CYLINDRICAL_SURFACE('',#24552,0.275);
#21128=CYLINDRICAL_SURFACE('',#24555,0.275);
#21129=CYLINDRICAL_SURFACE('',#24558,0.275);
#21130=CYLINDRICAL_SURFACE('',#24568,0.210000000000001);
#21131=CYLINDRICAL_SURFACE('',#24571,0.210000000000001);
#21132=CYLINDRICAL_SURFACE('',#24574,0.210000000000001);
#21133=CYLINDRICAL_SURFACE('',#24577,0.210000000000001);
#21134=CYLINDRICAL_SURFACE('',#24580,0.275);
#21135=CYLINDRICAL_SURFACE('',#24583,0.275);
#21136=CYLINDRICAL_SURFACE('',#24586,0.275);
#21137=CYLINDRICAL_SURFACE('',#24589,0.275);
#21138=CYLINDRICAL_SURFACE('',#24592,0.275);
#21139=CYLINDRICAL_SURFACE('',#24595,0.275);
#21140=CYLINDRICAL_SURFACE('',#24598,0.275);
#21141=CYLINDRICAL_SURFACE('',#24601,0.275);
#21142=CYLINDRICAL_SURFACE('',#24611,0.210000000000001);
#21143=CYLINDRICAL_SURFACE('',#24615,0.210000000000001);
#21144=CYLINDRICAL_SURFACE('',#24619,0.210000000000001);
#21145=CYLINDRICAL_SURFACE('',#24623,0.210000000000001);
#21146=CYLINDRICAL_SURFACE('',#24627,0.165);
#21147=CYLINDRICAL_SURFACE('',#24631,0.165);
#21148=CYLINDRICAL_SURFACE('',#24635,0.165);
#21149=CYLINDRICAL_SURFACE('',#24639,1.11);
#21150=CYLINDRICAL_SURFACE('',#24652,0.21);
#21151=CYLINDRICAL_SURFACE('',#24658,0.21);
#21152=CYLINDRICAL_SURFACE('',#24664,0.21);
#21153=CYLINDRICAL_SURFACE('',#24670,0.21);
#21154=CYLINDRICAL_SURFACE('',#24717,0.265);
#21155=CYLINDRICAL_SURFACE('',#24721,0.5);
#21156=CYLINDRICAL_SURFACE('',#24736,0.25);
#21157=CYLINDRICAL_SURFACE('',#24743,0.425);
#21158=CYLINDRICAL_SURFACE('',#24751,0.24505);
#21159=CYLINDRICAL_SURFACE('',#24753,0.457875);
#21160=CYLINDRICAL_SURFACE('',#24755,0.457875);
#21161=CYLINDRICAL_SURFACE('',#24756,0.457875);
#21162=CYLINDRICAL_SURFACE('',#24757,0.457875);
#21163=CYLINDRICAL_SURFACE('',#24758,0.457875);
#21164=CYLINDRICAL_SURFACE('',#24759,0.457875);
#21165=CYLINDRICAL_SURFACE('',#24760,0.457875);
#21166=CYLINDRICAL_SURFACE('',#24761,0.457875);
#21167=CYLINDRICAL_SURFACE('',#24762,0.457875);
#21168=CYLINDRICAL_SURFACE('',#24764,0.625);
#21169=CYLINDRICAL_SURFACE('',#24766,0.625);
#21170=CYLINDRICAL_SURFACE('',#24767,0.625);
#21171=CYLINDRICAL_SURFACE('',#24768,0.625);
#21172=CYLINDRICAL_SURFACE('',#24769,0.625);
#21173=CYLINDRICAL_SURFACE('',#24770,0.625);
#21174=CYLINDRICAL_SURFACE('',#24771,0.625);
#21175=CYLINDRICAL_SURFACE('',#24772,0.625);
#21176=CYLINDRICAL_SURFACE('',#24773,0.625);
#21177=CYLINDRICAL_SURFACE('',#24775,0.625);
#21178=CYLINDRICAL_SURFACE('',#24782,0.225);
#21179=CYLINDRICAL_SURFACE('',#24784,0.225);
#21180=CYLINDRICAL_SURFACE('',#24786,0.225);
#21181=CYLINDRICAL_SURFACE('',#24792,1.9);
#21182=CYLINDRICAL_SURFACE('',#24793,0.457875);
#21183=CYLINDRICAL_SURFACE('',#24794,1.1);
#21184=CYLINDRICAL_SURFACE('',#24802,0.35);
#21185=CYLINDRICAL_SURFACE('',#24810,0.1954);
#21186=CYLINDRICAL_SURFACE('',#24828,0.425);
#21187=CYLINDRICAL_SURFACE('',#24836,0.24505);
#21188=CYLINDRICAL_SURFACE('',#24871,0.5941);
#21189=CYLINDRICAL_SURFACE('',#24873,0.5941);
#21190=CYLINDRICAL_SURFACE('',#24874,0.5941);
#21191=CYLINDRICAL_SURFACE('',#24875,0.5941);
#21192=CYLINDRICAL_SURFACE('',#24876,0.5941);
#21193=CYLINDRICAL_SURFACE('',#24877,0.5941);
#21194=CYLINDRICAL_SURFACE('',#24878,0.5941);
#21195=CYLINDRICAL_SURFACE('',#24879,0.5941);
#21196=CYLINDRICAL_SURFACE('',#24880,0.5941);
#21197=CYLINDRICAL_SURFACE('',#24881,0.5941);
#21198=CYLINDRICAL_SURFACE('',#24882,0.5941);
#21199=CYLINDRICAL_SURFACE('',#24883,0.5941);
#21200=CYLINDRICAL_SURFACE('',#24884,0.5941);
#21201=CYLINDRICAL_SURFACE('',#24885,0.5941);
#21202=CYLINDRICAL_SURFACE('',#24886,0.5941);
#21203=CYLINDRICAL_SURFACE('',#24887,0.5941);
#21204=CYLINDRICAL_SURFACE('',#24888,0.5941);
#21205=CYLINDRICAL_SURFACE('',#24889,0.5941);
#21206=CYLINDRICAL_SURFACE('',#24890,0.5941);
#21207=CYLINDRICAL_SURFACE('',#24891,0.5941);
#21208=CYLINDRICAL_SURFACE('',#24892,0.5941);
#21209=CYLINDRICAL_SURFACE('',#24893,0.5941);
#21210=CYLINDRICAL_SURFACE('',#24894,0.5941);
#21211=CYLINDRICAL_SURFACE('',#24895,0.5941);
#21212=CYLINDRICAL_SURFACE('',#24896,0.5941);
#21213=CYLINDRICAL_SURFACE('',#24897,0.5941);
#21214=CYLINDRICAL_SURFACE('',#24898,0.5941);
#21215=CYLINDRICAL_SURFACE('',#24899,0.5941);
#21216=CYLINDRICAL_SURFACE('',#24900,0.5941);
#21217=CYLINDRICAL_SURFACE('',#24901,0.5941);
#21218=CYLINDRICAL_SURFACE('',#24902,0.5941);
#21219=CYLINDRICAL_SURFACE('',#24903,0.5941);
#21220=CYLINDRICAL_SURFACE('',#24904,0.5941);
#21221=CYLINDRICAL_SURFACE('',#24905,0.5941);
#21222=CYLINDRICAL_SURFACE('',#24906,0.5941);
#21223=CYLINDRICAL_SURFACE('',#24907,0.5941);
#21224=CYLINDRICAL_SURFACE('',#24908,0.5941);
#21225=CYLINDRICAL_SURFACE('',#24909,0.5941);
#21226=CYLINDRICAL_SURFACE('',#24910,0.5941);
#21227=CYLINDRICAL_SURFACE('',#24911,0.5941);
#21228=CYLINDRICAL_SURFACE('',#24912,0.5941);
#21229=CYLINDRICAL_SURFACE('',#24913,0.5941);
#21230=CYLINDRICAL_SURFACE('',#24914,0.5941);
#21231=CYLINDRICAL_SURFACE('',#24915,0.5941);
#21232=CYLINDRICAL_SURFACE('',#24916,0.5941);
#21233=CYLINDRICAL_SURFACE('',#24917,0.5941);
#21234=CYLINDRICAL_SURFACE('',#24918,0.5941);
#21235=CYLINDRICAL_SURFACE('',#24919,0.5941);
#21236=CYLINDRICAL_SURFACE('',#24920,0.5941);
#21237=CYLINDRICAL_SURFACE('',#24921,0.5941);
#21238=CYLINDRICAL_SURFACE('',#24922,0.5941);
#21239=CYLINDRICAL_SURFACE('',#24923,0.5941);
#21240=CYLINDRICAL_SURFACE('',#24924,0.5941);
#21241=CYLINDRICAL_SURFACE('',#24925,0.5941);
#21242=CYLINDRICAL_SURFACE('',#24926,0.5941);
#21243=CYLINDRICAL_SURFACE('',#24927,0.5941);
#21244=CYLINDRICAL_SURFACE('',#24928,0.5941);
#21245=CYLINDRICAL_SURFACE('',#24929,0.5941);
#21246=CYLINDRICAL_SURFACE('',#24930,0.5941);
#21247=CYLINDRICAL_SURFACE('',#24931,0.5941);
#21248=CYLINDRICAL_SURFACE('',#24932,0.5941);
#21249=CYLINDRICAL_SURFACE('',#24933,0.5941);
#21250=CYLINDRICAL_SURFACE('',#24934,0.5941);
#21251=CYLINDRICAL_SURFACE('',#24935,0.415875);
#21252=CYLINDRICAL_SURFACE('',#24937,0.415875);
#21253=CYLINDRICAL_SURFACE('',#24939,0.415875);
#21254=CYLINDRICAL_SURFACE('',#24940,0.415875);
#21255=CYLINDRICAL_SURFACE('',#24941,0.415875);
#21256=CYLINDRICAL_SURFACE('',#24942,0.415875);
#21257=CYLINDRICAL_SURFACE('',#24943,0.415875);
#21258=CYLINDRICAL_SURFACE('',#24944,0.415875);
#21259=CYLINDRICAL_SURFACE('',#24945,0.415875);
#21260=CYLINDRICAL_SURFACE('',#24946,0.415875);
#21261=CYLINDRICAL_SURFACE('',#24947,0.415875);
#21262=CYLINDRICAL_SURFACE('',#24948,0.415875);
#21263=CYLINDRICAL_SURFACE('',#24949,0.415875);
#21264=CYLINDRICAL_SURFACE('',#24950,0.415875);
#21265=CYLINDRICAL_SURFACE('',#24951,0.415875);
#21266=CYLINDRICAL_SURFACE('',#24952,0.415875);
#21267=CYLINDRICAL_SURFACE('',#24953,0.415875);
#21268=CYLINDRICAL_SURFACE('',#24954,0.415875);
#21269=CYLINDRICAL_SURFACE('',#24955,0.415875);
#21270=CYLINDRICAL_SURFACE('',#24956,0.415875);
#21271=CYLINDRICAL_SURFACE('',#24957,0.415875);
#21272=CYLINDRICAL_SURFACE('',#24958,0.415875);
#21273=CYLINDRICAL_SURFACE('',#24959,0.415875);
#21274=CYLINDRICAL_SURFACE('',#24960,0.415875);
#21275=CYLINDRICAL_SURFACE('',#24961,0.415875);
#21276=CYLINDRICAL_SURFACE('',#24962,0.415875);
#21277=CYLINDRICAL_SURFACE('',#24963,0.415875);
#21278=CYLINDRICAL_SURFACE('',#24964,0.415875);
#21279=CYLINDRICAL_SURFACE('',#24965,0.415875);
#21280=CYLINDRICAL_SURFACE('',#24966,0.415875);
#21281=CYLINDRICAL_SURFACE('',#24967,0.415875);
#21282=CYLINDRICAL_SURFACE('',#24968,0.415875);
#21283=CYLINDRICAL_SURFACE('',#24969,0.415875);
#21284=CYLINDRICAL_SURFACE('',#24970,0.415875);
#21285=CYLINDRICAL_SURFACE('',#24971,0.415875);
#21286=CYLINDRICAL_SURFACE('',#24972,0.415875);
#21287=CYLINDRICAL_SURFACE('',#24973,0.415875);
#21288=CYLINDRICAL_SURFACE('',#24974,0.415875);
#21289=CYLINDRICAL_SURFACE('',#24975,0.415875);
#21290=CYLINDRICAL_SURFACE('',#24976,0.415875);
#21291=CYLINDRICAL_SURFACE('',#24977,0.415875);
#21292=CYLINDRICAL_SURFACE('',#24978,0.415875);
#21293=CYLINDRICAL_SURFACE('',#24979,0.415875);
#21294=CYLINDRICAL_SURFACE('',#24980,0.415875);
#21295=CYLINDRICAL_SURFACE('',#24981,0.415875);
#21296=CYLINDRICAL_SURFACE('',#24982,0.415875);
#21297=CYLINDRICAL_SURFACE('',#24983,0.415875);
#21298=CYLINDRICAL_SURFACE('',#24984,0.415875);
#21299=CYLINDRICAL_SURFACE('',#24985,0.415875);
#21300=CYLINDRICAL_SURFACE('',#24986,0.415875);
#21301=CYLINDRICAL_SURFACE('',#24987,0.415875);
#21302=CYLINDRICAL_SURFACE('',#24988,0.415875);
#21303=CYLINDRICAL_SURFACE('',#24989,0.415875);
#21304=CYLINDRICAL_SURFACE('',#24990,0.415875);
#21305=CYLINDRICAL_SURFACE('',#24991,0.415875);
#21306=CYLINDRICAL_SURFACE('',#24992,0.415875);
#21307=CYLINDRICAL_SURFACE('',#24993,0.415875);
#21308=CYLINDRICAL_SURFACE('',#24994,0.415875);
#21309=CYLINDRICAL_SURFACE('',#24995,0.415875);
#21310=CYLINDRICAL_SURFACE('',#24996,0.415875);
#21311=CYLINDRICAL_SURFACE('',#24997,0.415875);
#21312=CYLINDRICAL_SURFACE('',#24998,0.415875);
#21313=CYLINDRICAL_SURFACE('',#24999,0.415875);
#21314=CYLINDRICAL_SURFACE('',#25003,0.6);
#21315=CYLINDRICAL_SURFACE('',#25006,0.415875);
#21316=CYLINDRICAL_SURFACE('',#25014,1.);
#21317=CYLINDRICAL_SURFACE('',#25021,1.35);
#21318=CYLINDRICAL_SURFACE('',#25024,0.5941);
#21319=CYLINDRICAL_SURFACE('',#25026,1.01);
#21320=CYLINDRICAL_SURFACE('',#25029,1.35);
#21321=CYLINDRICAL_SURFACE('',#25037,0.210000000000001);
#21322=CYLINDRICAL_SURFACE('',#25040,1.005);
#21323=CYLINDRICAL_SURFACE('',#25043,1.5);
#21324=CYLINDRICAL_SURFACE('',#25049,0.25);
#21325=CYLINDRICAL_SURFACE('',#25054,0.210000000000001);
#21326=CYLINDRICAL_SURFACE('',#25066,3.5);
#21327=CYLINDRICAL_SURFACE('',#25067,1.);
#21328=CYLINDRICAL_SURFACE('',#25069,1.5);
#21329=CYLINDRICAL_SURFACE('',#25073,0.33);
#21330=CYLINDRICAL_SURFACE('',#25076,0.4);
#21331=CYLINDRICAL_SURFACE('',#25082,0.405);
#21332=CYLINDRICAL_SURFACE('',#25085,0.9);
#21333=CYLINDRICAL_SURFACE('',#25113,0.24505);
#21334=CYLINDRICAL_SURFACE('',#25119,0.32);
#21335=CYLINDRICAL_SURFACE('',#25122,0.6);
#21336=CYLINDRICAL_SURFACE('',#25132,0.5);
#21337=CYLINDRICAL_SURFACE('',#25140,0.2942);
#21338=CYLINDRICAL_SURFACE('',#25203,0.550000000000001);
#21339=CYLINDRICAL_SURFACE('',#25207,0.550000000000001);
#21340=CYLINDRICAL_SURFACE('',#25211,0.550000000000001);
#21341=CYLINDRICAL_SURFACE('',#25215,0.550000000000001);
#21342=CYLINDRICAL_SURFACE('',#25219,0.550000000000001);
#21343=CYLINDRICAL_SURFACE('',#25223,0.550000000000001);
#21344=CYLINDRICAL_SURFACE('',#25227,0.550000000000001);
#21345=CYLINDRICAL_SURFACE('',#25231,0.550000000000001);
#21346=CYLINDRICAL_SURFACE('',#25235,0.5);
#21347=CYLINDRICAL_SURFACE('',#25240,0.5);
#21348=CYLINDRICAL_SURFACE('',#25245,0.5);
#21349=CYLINDRICAL_SURFACE('',#25250,0.5);
#21350=CYLINDRICAL_SURFACE('',#25255,0.275);
#21351=CYLINDRICAL_SURFACE('',#25257,0.274999999999999);
#21352=CYLINDRICAL_SURFACE('',#25259,0.275);
#21353=CYLINDRICAL_SURFACE('',#25261,0.274999999999999);
#21354=CYLINDRICAL_SURFACE('',#25263,0.210000000000001);
#21355=CYLINDRICAL_SURFACE('',#25266,0.21);
#21356=CYLINDRICAL_SURFACE('',#25269,0.329999999999998);
#21357=CYLINDRICAL_SURFACE('',#25272,0.329999999999998);
#21358=CYLINDRICAL_SURFACE('',#25275,0.275);
#21359=CYLINDRICAL_SURFACE('',#25278,0.275);
#21360=CYLINDRICAL_SURFACE('',#25281,0.210000000000001);
#21361=CYLINDRICAL_SURFACE('',#25284,0.21);
#21362=CYLINDRICAL_SURFACE('',#25287,0.21);
#21363=CYLINDRICAL_SURFACE('',#25290,0.210000000000001);
#21364=CYLINDRICAL_SURFACE('',#25300,0.5);
#21365=CYLINDRICAL_SURFACE('',#25303,0.5);
#21366=CYLINDRICAL_SURFACE('',#25306,0.164999999999999);
#21367=CYLINDRICAL_SURFACE('',#25309,0.164999999999999);
#21368=CYLINDRICAL_SURFACE('',#25312,0.165);
#21369=CYLINDRICAL_SURFACE('',#25315,0.164999999999999);
#21370=CYLINDRICAL_SURFACE('',#25318,0.5);
#21371=CYLINDRICAL_SURFACE('',#25323,0.5);
#21372=CYLINDRICAL_SURFACE('',#25328,0.5);
#21373=CYLINDRICAL_SURFACE('',#25333,0.5);
#21374=CYLINDRICAL_SURFACE('',#25339,0.274999999999999);
#21375=CYLINDRICAL_SURFACE('',#25341,0.275);
#21376=CYLINDRICAL_SURFACE('',#25343,0.275);
#21377=CYLINDRICAL_SURFACE('',#25345,0.274999999999999);
#21378=CYLINDRICAL_SURFACE('',#25353,0.165);
#21379=CYLINDRICAL_SURFACE('',#25356,0.165);
#21380=CYLINDRICAL_SURFACE('',#25359,0.165);
#21381=CYLINDRICAL_SURFACE('',#25362,1.6);
#21382=CYLINDRICAL_SURFACE('',#25367,1.4);
#21383=CYLINDRICAL_SURFACE('',#25369,0.21);
#21384=CYLINDRICAL_SURFACE('',#25373,0.21);
#21385=CYLINDRICAL_SURFACE('',#25384,0.225);
#21386=CYLINDRICAL_SURFACE('',#25387,0.225);
#21387=CYLINDRICAL_SURFACE('',#25390,0.225);
#21388=CYLINDRICAL_SURFACE('',#25393,1.59);
#21389=CYLINDRICAL_SURFACE('',#25398,1.2);
#21390=CYLINDRICAL_SURFACE('',#25400,2.4);
#21391=CYLINDRICAL_SURFACE('',#25406,0.165);
#21392=CYLINDRICAL_SURFACE('',#25409,0.165);
#21393=CYLINDRICAL_SURFACE('',#25412,0.165);
#21394=CYLINDRICAL_SURFACE('',#25415,2.35);
#21395=CYLINDRICAL_SURFACE('',#25420,2.15);
#21396=CYLINDRICAL_SURFACE('',#25422,0.25);
#21397=CYLINDRICAL_SURFACE('',#25426,0.25);
#21398=CYLINDRICAL_SURFACE('',#25437,0.225);
#21399=CYLINDRICAL_SURFACE('',#25440,0.225);
#21400=CYLINDRICAL_SURFACE('',#25443,0.225);
#21401=CYLINDRICAL_SURFACE('',#25450,3.);
#21402=CYLINDRICAL_SURFACE('',#25452,2.34);
#21403=CYLINDRICAL_SURFACE('',#25456,1.8);
#21404=CYLINDRICAL_SURFACE('',#25460,0.475);
#21405=CYLINDRICAL_SURFACE('',#25465,0.275);
#21406=CYLINDRICAL_SURFACE('',#25474,0.475000000000001);
#21407=CYLINDRICAL_SURFACE('',#25479,0.274999999999999);
#21408=CYLINDRICAL_SURFACE('',#25488,0.375);
#21409=CYLINDRICAL_SURFACE('',#25493,0.375);
#21410=CYLINDRICAL_SURFACE('',#25498,0.375);
#21411=CYLINDRICAL_SURFACE('',#25503,0.375);
#21412=CYLINDRICAL_SURFACE('',#25508,0.225);
#21413=CYLINDRICAL_SURFACE('',#25510,0.225);
#21414=CYLINDRICAL_SURFACE('',#25512,0.225);
#21415=CYLINDRICAL_SURFACE('',#25514,0.225000000000001);
#21416=CYLINDRICAL_SURFACE('',#25538,1.070235);
#21417=CYLINDRICAL_SURFACE('',#25540,0.6);
#21418=CYLINDRICAL_SURFACE('',#25546,1.070235);
#21419=CYLINDRICAL_SURFACE('',#25558,1.129765);
#21420=CYLINDRICAL_SURFACE('',#25565,1.6);
#21421=CYLINDRICAL_SURFACE('',#25570,1.129765);
#21422=CYLINDRICAL_SURFACE('',#25590,1.123812);
#21423=CYLINDRICAL_SURFACE('',#25626,1.076188);
#21424=CYLINDRICAL_SURFACE('',#25640,1.119765);
#21425=CYLINDRICAL_SURFACE('',#25644,1.085235);
#21426=CYLINDRICAL_SURFACE('',#25648,1.119765);
#21427=CYLINDRICAL_SURFACE('',#25652,1.085235);
#21428=CYLINDRICAL_SURFACE('',#25666,1.63531);
#21429=CYLINDRICAL_SURFACE('',#25668,1.);
#21430=CYLINDRICAL_SURFACE('',#25674,1.63531);
#21431=CYLINDRICAL_SURFACE('',#25686,1.71469);
#21432=CYLINDRICAL_SURFACE('',#25693,2.35);
#21433=CYLINDRICAL_SURFACE('',#25698,1.71469);
#21434=CYLINDRICAL_SURFACE('',#25720,1.706752);
#21435=CYLINDRICAL_SURFACE('',#25760,1.643248);
#21436=CYLINDRICAL_SURFACE('',#25774,1.70469);
#21437=CYLINDRICAL_SURFACE('',#25778,1.65031);
#21438=CYLINDRICAL_SURFACE('',#25782,1.70469);
#21439=CYLINDRICAL_SURFACE('',#25786,1.65031);
#21440=CYLINDRICAL_SURFACE('',#25807,0.425);
#21441=CYLINDRICAL_SURFACE('',#25815,0.24505);
#21442=CYLINDRICAL_SURFACE('',#25818,0.275);
#21443=CYLINDRICAL_SURFACE('',#25821,0.275);
#21444=CYLINDRICAL_SURFACE('',#25824,0.275);
#21445=CYLINDRICAL_SURFACE('',#25827,0.275);
#21446=CYLINDRICAL_SURFACE('',#25837,0.275);
#21447=CYLINDRICAL_SURFACE('',#25840,0.275);
#21448=CYLINDRICAL_SURFACE('',#25843,0.275);
#21449=CYLINDRICAL_SURFACE('',#25846,0.275);
#21450=CYLINDRICAL_SURFACE('',#25849,0.275);
#21451=CYLINDRICAL_SURFACE('',#25852,0.275);
#21452=CYLINDRICAL_SURFACE('',#25855,0.275);
#21453=CYLINDRICAL_SURFACE('',#25858,0.275);
#21454=CYLINDRICAL_SURFACE('',#25868,0.210000000000001);
#21455=CYLINDRICAL_SURFACE('',#25872,0.210000000000001);
#21456=CYLINDRICAL_SURFACE('',#25876,0.210000000000001);
#21457=CYLINDRICAL_SURFACE('',#25880,0.210000000000001);
#21458=CYLINDRICAL_SURFACE('',#25884,0.165);
#21459=CYLINDRICAL_SURFACE('',#25888,0.165);
#21460=CYLINDRICAL_SURFACE('',#25892,0.165);
#21461=CYLINDRICAL_SURFACE('',#25896,1.11);
#21462=CYLINDRICAL_SURFACE('',#25909,0.21);
#21463=CYLINDRICAL_SURFACE('',#25915,0.21);
#21464=CYLINDRICAL_SURFACE('',#25921,0.21);
#21465=CYLINDRICAL_SURFACE('',#25927,0.21);
#21466=CYLINDRICAL_SURFACE('',#25974,0.265);
#21467=CYLINDRICAL_SURFACE('',#25978,0.5);
#21468=CYLINDRICAL_SURFACE('',#25993,0.25);
#21469=CYLINDRICAL_SURFACE('',#26000,0.425);
#21470=CYLINDRICAL_SURFACE('',#26008,0.24505);
#21471=CYLINDRICAL_SURFACE('',#26010,0.457875);
#21472=CYLINDRICAL_SURFACE('',#26012,0.457875);
#21473=CYLINDRICAL_SURFACE('',#26013,0.457875);
#21474=CYLINDRICAL_SURFACE('',#26014,0.457875);
#21475=CYLINDRICAL_SURFACE('',#26015,0.457875);
#21476=CYLINDRICAL_SURFACE('',#26016,0.457875);
#21477=CYLINDRICAL_SURFACE('',#26017,0.457875);
#21478=CYLINDRICAL_SURFACE('',#26018,0.457875);
#21479=CYLINDRICAL_SURFACE('',#26019,0.457875);
#21480=CYLINDRICAL_SURFACE('',#26021,0.625);
#21481=CYLINDRICAL_SURFACE('',#26023,0.625);
#21482=CYLINDRICAL_SURFACE('',#26024,0.625);
#21483=CYLINDRICAL_SURFACE('',#26025,0.625);
#21484=CYLINDRICAL_SURFACE('',#26026,0.625);
#21485=CYLINDRICAL_SURFACE('',#26027,0.625);
#21486=CYLINDRICAL_SURFACE('',#26028,0.625);
#21487=CYLINDRICAL_SURFACE('',#26029,0.625);
#21488=CYLINDRICAL_SURFACE('',#26030,0.625);
#21489=CYLINDRICAL_SURFACE('',#26032,0.625);
#21490=CYLINDRICAL_SURFACE('',#26039,0.225);
#21491=CYLINDRICAL_SURFACE('',#26041,0.225);
#21492=CYLINDRICAL_SURFACE('',#26043,0.225);
#21493=CYLINDRICAL_SURFACE('',#26049,1.9);
#21494=CYLINDRICAL_SURFACE('',#26050,0.457875);
#21495=CYLINDRICAL_SURFACE('',#26051,1.1);
#21496=CYLINDRICAL_SURFACE('',#26059,0.35);
#21497=CYLINDRICAL_SURFACE('',#26067,0.1954);
#21498=CYLINDRICAL_SURFACE('',#26085,0.425);
#21499=CYLINDRICAL_SURFACE('',#26093,0.24505);
#21500=CYLINDRICAL_SURFACE('',#26128,0.5941);
#21501=CYLINDRICAL_SURFACE('',#26130,0.5941);
#21502=CYLINDRICAL_SURFACE('',#26131,0.5941);
#21503=CYLINDRICAL_SURFACE('',#26132,0.5941);
#21504=CYLINDRICAL_SURFACE('',#26133,0.5941);
#21505=CYLINDRICAL_SURFACE('',#26134,0.5941);
#21506=CYLINDRICAL_SURFACE('',#26135,0.5941);
#21507=CYLINDRICAL_SURFACE('',#26136,0.5941);
#21508=CYLINDRICAL_SURFACE('',#26137,0.5941);
#21509=CYLINDRICAL_SURFACE('',#26138,0.5941);
#21510=CYLINDRICAL_SURFACE('',#26139,0.5941);
#21511=CYLINDRICAL_SURFACE('',#26140,0.5941);
#21512=CYLINDRICAL_SURFACE('',#26141,0.5941);
#21513=CYLINDRICAL_SURFACE('',#26142,0.5941);
#21514=CYLINDRICAL_SURFACE('',#26143,0.5941);
#21515=CYLINDRICAL_SURFACE('',#26144,0.5941);
#21516=CYLINDRICAL_SURFACE('',#26145,0.5941);
#21517=CYLINDRICAL_SURFACE('',#26146,0.5941);
#21518=CYLINDRICAL_SURFACE('',#26147,0.5941);
#21519=CYLINDRICAL_SURFACE('',#26148,0.5941);
#21520=CYLINDRICAL_SURFACE('',#26149,0.5941);
#21521=CYLINDRICAL_SURFACE('',#26150,0.5941);
#21522=CYLINDRICAL_SURFACE('',#26151,0.5941);
#21523=CYLINDRICAL_SURFACE('',#26152,0.5941);
#21524=CYLINDRICAL_SURFACE('',#26153,0.5941);
#21525=CYLINDRICAL_SURFACE('',#26154,0.5941);
#21526=CYLINDRICAL_SURFACE('',#26155,0.5941);
#21527=CYLINDRICAL_SURFACE('',#26156,0.5941);
#21528=CYLINDRICAL_SURFACE('',#26157,0.5941);
#21529=CYLINDRICAL_SURFACE('',#26158,0.5941);
#21530=CYLINDRICAL_SURFACE('',#26159,0.5941);
#21531=CYLINDRICAL_SURFACE('',#26160,0.5941);
#21532=CYLINDRICAL_SURFACE('',#26161,0.5941);
#21533=CYLINDRICAL_SURFACE('',#26162,0.5941);
#21534=CYLINDRICAL_SURFACE('',#26163,0.5941);
#21535=CYLINDRICAL_SURFACE('',#26164,0.5941);
#21536=CYLINDRICAL_SURFACE('',#26165,0.5941);
#21537=CYLINDRICAL_SURFACE('',#26166,0.5941);
#21538=CYLINDRICAL_SURFACE('',#26167,0.5941);
#21539=CYLINDRICAL_SURFACE('',#26168,0.5941);
#21540=CYLINDRICAL_SURFACE('',#26169,0.5941);
#21541=CYLINDRICAL_SURFACE('',#26170,0.5941);
#21542=CYLINDRICAL_SURFACE('',#26171,0.5941);
#21543=CYLINDRICAL_SURFACE('',#26172,0.5941);
#21544=CYLINDRICAL_SURFACE('',#26173,0.5941);
#21545=CYLINDRICAL_SURFACE('',#26174,0.5941);
#21546=CYLINDRICAL_SURFACE('',#26175,0.5941);
#21547=CYLINDRICAL_SURFACE('',#26176,0.5941);
#21548=CYLINDRICAL_SURFACE('',#26177,0.5941);
#21549=CYLINDRICAL_SURFACE('',#26178,0.5941);
#21550=CYLINDRICAL_SURFACE('',#26179,0.5941);
#21551=CYLINDRICAL_SURFACE('',#26180,0.5941);
#21552=CYLINDRICAL_SURFACE('',#26181,0.5941);
#21553=CYLINDRICAL_SURFACE('',#26182,0.5941);
#21554=CYLINDRICAL_SURFACE('',#26183,0.5941);
#21555=CYLINDRICAL_SURFACE('',#26184,0.5941);
#21556=CYLINDRICAL_SURFACE('',#26185,0.5941);
#21557=CYLINDRICAL_SURFACE('',#26186,0.5941);
#21558=CYLINDRICAL_SURFACE('',#26187,0.5941);
#21559=CYLINDRICAL_SURFACE('',#26188,0.5941);
#21560=CYLINDRICAL_SURFACE('',#26189,0.5941);
#21561=CYLINDRICAL_SURFACE('',#26190,0.5941);
#21562=CYLINDRICAL_SURFACE('',#26191,0.5941);
#21563=CYLINDRICAL_SURFACE('',#26192,0.415875);
#21564=CYLINDRICAL_SURFACE('',#26194,0.415875);
#21565=CYLINDRICAL_SURFACE('',#26196,0.415875);
#21566=CYLINDRICAL_SURFACE('',#26197,0.415875);
#21567=CYLINDRICAL_SURFACE('',#26198,0.415875);
#21568=CYLINDRICAL_SURFACE('',#26199,0.415875);
#21569=CYLINDRICAL_SURFACE('',#26200,0.415875);
#21570=CYLINDRICAL_SURFACE('',#26201,0.415875);
#21571=CYLINDRICAL_SURFACE('',#26202,0.415875);
#21572=CYLINDRICAL_SURFACE('',#26203,0.415875);
#21573=CYLINDRICAL_SURFACE('',#26204,0.415875);
#21574=CYLINDRICAL_SURFACE('',#26205,0.415875);
#21575=CYLINDRICAL_SURFACE('',#26206,0.415875);
#21576=CYLINDRICAL_SURFACE('',#26207,0.415875);
#21577=CYLINDRICAL_SURFACE('',#26208,0.415875);
#21578=CYLINDRICAL_SURFACE('',#26209,0.415875);
#21579=CYLINDRICAL_SURFACE('',#26210,0.415875);
#21580=CYLINDRICAL_SURFACE('',#26211,0.415875);
#21581=CYLINDRICAL_SURFACE('',#26212,0.415875);
#21582=CYLINDRICAL_SURFACE('',#26213,0.415875);
#21583=CYLINDRICAL_SURFACE('',#26214,0.415875);
#21584=CYLINDRICAL_SURFACE('',#26215,0.415875);
#21585=CYLINDRICAL_SURFACE('',#26216,0.415875);
#21586=CYLINDRICAL_SURFACE('',#26217,0.415875);
#21587=CYLINDRICAL_SURFACE('',#26218,0.415875);
#21588=CYLINDRICAL_SURFACE('',#26219,0.415875);
#21589=CYLINDRICAL_SURFACE('',#26220,0.415875);
#21590=CYLINDRICAL_SURFACE('',#26221,0.415875);
#21591=CYLINDRICAL_SURFACE('',#26222,0.415875);
#21592=CYLINDRICAL_SURFACE('',#26223,0.415875);
#21593=CYLINDRICAL_SURFACE('',#26224,0.415875);
#21594=CYLINDRICAL_SURFACE('',#26225,0.415875);
#21595=CYLINDRICAL_SURFACE('',#26226,0.415875);
#21596=CYLINDRICAL_SURFACE('',#26227,0.415875);
#21597=CYLINDRICAL_SURFACE('',#26228,0.415875);
#21598=CYLINDRICAL_SURFACE('',#26229,0.415875);
#21599=CYLINDRICAL_SURFACE('',#26230,0.415875);
#21600=CYLINDRICAL_SURFACE('',#26231,0.415875);
#21601=CYLINDRICAL_SURFACE('',#26232,0.415875);
#21602=CYLINDRICAL_SURFACE('',#26233,0.415875);
#21603=CYLINDRICAL_SURFACE('',#26234,0.415875);
#21604=CYLINDRICAL_SURFACE('',#26235,0.415875);
#21605=CYLINDRICAL_SURFACE('',#26236,0.415875);
#21606=CYLINDRICAL_SURFACE('',#26237,0.415875);
#21607=CYLINDRICAL_SURFACE('',#26238,0.415875);
#21608=CYLINDRICAL_SURFACE('',#26239,0.415875);
#21609=CYLINDRICAL_SURFACE('',#26240,0.415875);
#21610=CYLINDRICAL_SURFACE('',#26241,0.415875);
#21611=CYLINDRICAL_SURFACE('',#26242,0.415875);
#21612=CYLINDRICAL_SURFACE('',#26243,0.415875);
#21613=CYLINDRICAL_SURFACE('',#26244,0.415875);
#21614=CYLINDRICAL_SURFACE('',#26245,0.415875);
#21615=CYLINDRICAL_SURFACE('',#26246,0.415875);
#21616=CYLINDRICAL_SURFACE('',#26247,0.415875);
#21617=CYLINDRICAL_SURFACE('',#26248,0.415875);
#21618=CYLINDRICAL_SURFACE('',#26249,0.415875);
#21619=CYLINDRICAL_SURFACE('',#26250,0.415875);
#21620=CYLINDRICAL_SURFACE('',#26251,0.415875);
#21621=CYLINDRICAL_SURFACE('',#26252,0.415875);
#21622=CYLINDRICAL_SURFACE('',#26253,0.415875);
#21623=CYLINDRICAL_SURFACE('',#26254,0.415875);
#21624=CYLINDRICAL_SURFACE('',#26255,0.415875);
#21625=CYLINDRICAL_SURFACE('',#26256,0.415875);
#21626=CYLINDRICAL_SURFACE('',#26260,0.6);
#21627=CYLINDRICAL_SURFACE('',#26263,0.415875);
#21628=CYLINDRICAL_SURFACE('',#26271,1.);
#21629=CYLINDRICAL_SURFACE('',#26278,1.35);
#21630=CYLINDRICAL_SURFACE('',#26281,0.5941);
#21631=CYLINDRICAL_SURFACE('',#26283,1.01);
#21632=CYLINDRICAL_SURFACE('',#26286,1.35);
#21633=CYLINDRICAL_SURFACE('',#26294,0.210000000000001);
#21634=CYLINDRICAL_SURFACE('',#26297,1.005);
#21635=CYLINDRICAL_SURFACE('',#26300,1.5);
#21636=CYLINDRICAL_SURFACE('',#26306,0.25);
#21637=CYLINDRICAL_SURFACE('',#26311,0.210000000000001);
#21638=CYLINDRICAL_SURFACE('',#26323,3.5);
#21639=CYLINDRICAL_SURFACE('',#26324,1.);
#21640=CYLINDRICAL_SURFACE('',#26326,1.5);
#21641=CYLINDRICAL_SURFACE('',#26330,0.33);
#21642=CYLINDRICAL_SURFACE('',#26333,0.4);
#21643=CYLINDRICAL_SURFACE('',#26339,0.405);
#21644=CYLINDRICAL_SURFACE('',#26342,0.9);
#21645=CYLINDRICAL_SURFACE('',#26370,0.24505);
#21646=CYLINDRICAL_SURFACE('',#26376,0.32);
#21647=CYLINDRICAL_SURFACE('',#26379,0.6);
#21648=CYLINDRICAL_SURFACE('',#26389,0.5);
#21649=CYLINDRICAL_SURFACE('',#26397,0.2942);
#21650=ADVANCED_FACE('',(#2869),#21040,.F.);
#21651=ADVANCED_FACE('',(#2870),#21041,.F.);
#21652=ADVANCED_FACE('',(#2871),#21042,.F.);
#21653=ADVANCED_FACE('',(#2872),#21043,.F.);
#21654=ADVANCED_FACE('',(#2873),#21044,.F.);
#21655=ADVANCED_FACE('',(#2874),#21045,.F.);
#21656=ADVANCED_FACE('',(#2875),#21046,.F.);
#21657=ADVANCED_FACE('',(#2876),#21047,.F.);
#21658=ADVANCED_FACE('',(#2877),#21048,.F.);
#21659=ADVANCED_FACE('',(#2878),#21049,.F.);
#21660=ADVANCED_FACE('',(#2879),#2296,.T.);
#21661=ADVANCED_FACE('',(#2880),#2297,.T.);
#21662=ADVANCED_FACE('',(#2881),#2298,.T.);
#21663=ADVANCED_FACE('',(#2882),#2299,.T.);
#21664=ADVANCED_FACE('',(#2883,#1887,#1888,#1889,#1890,#1891,#1892,#1893,
#1894,#1895,#1896),#2300,.T.);
#21665=ADVANCED_FACE('',(#2884,#1897,#1898,#1899,#1900,#1901,#1902,#1903,
#1904,#1905,#1906),#2301,.F.);
#21666=ADVANCED_FACE('',(#2885),#2302,.T.);
#21667=ADVANCED_FACE('',(#2886),#2303,.T.);
#21668=ADVANCED_FACE('',(#2887),#2304,.T.);
#21669=ADVANCED_FACE('',(#2888),#2305,.T.);
#21670=ADVANCED_FACE('',(#2889),#2306,.T.);
#21671=ADVANCED_FACE('',(#2890),#2307,.F.);
#21672=ADVANCED_FACE('',(#2891),#2308,.T.);
#21673=ADVANCED_FACE('',(#2892),#2309,.T.);
#21674=ADVANCED_FACE('',(#2893),#2310,.T.);
#21675=ADVANCED_FACE('',(#2894),#2311,.T.);
#21676=ADVANCED_FACE('',(#2895),#2312,.T.);
#21677=ADVANCED_FACE('',(#2896),#2313,.F.);
#21678=ADVANCED_FACE('',(#2897),#21050,.F.);
#21679=ADVANCED_FACE('',(#2898),#21051,.F.);
#21680=ADVANCED_FACE('',(#2899),#21052,.F.);
#21681=ADVANCED_FACE('',(#2900),#21053,.F.);
#21682=ADVANCED_FACE('',(#2901),#21054,.F.);
#21683=ADVANCED_FACE('',(#2902),#21055,.F.);
#21684=ADVANCED_FACE('',(#2903),#21056,.F.);
#21685=ADVANCED_FACE('',(#2904,#1907),#2314,.T.);
#21686=ADVANCED_FACE('',(#2905),#21057,.F.);
#21687=ADVANCED_FACE('',(#2906,#1908),#2315,.T.);
#21688=ADVANCED_FACE('',(#2907),#21058,.F.);
#21689=ADVANCED_FACE('',(#2908,#1909),#2316,.T.);
#21690=ADVANCED_FACE('',(#2909),#21059,.F.);
#21691=ADVANCED_FACE('',(#2910,#1910),#2317,.T.);
#21692=ADVANCED_FACE('',(#2911,#1911,#1912,#1913,#1914,#1915,#1916),#2318,
 .T.);
#21693=ADVANCED_FACE('',(#2912),#21060,.F.);
#21694=ADVANCED_FACE('',(#2913),#21061,.F.);
#21695=ADVANCED_FACE('',(#2914),#21062,.F.);
#21696=ADVANCED_FACE('',(#2915),#21063,.F.);
#21697=ADVANCED_FACE('',(#2916),#2319,.T.);
#21698=ADVANCED_FACE('',(#2917),#2320,.T.);
#21699=ADVANCED_FACE('',(#2918),#2321,.T.);
#21700=ADVANCED_FACE('',(#2919),#2322,.T.);
#21701=ADVANCED_FACE('',(#2920,#1917,#1918,#1919,#1920,#1921,#1922,#1923,
#1924),#2323,.F.);
#21702=ADVANCED_FACE('',(#2921),#21064,.F.);
#21703=ADVANCED_FACE('',(#2922),#21065,.F.);
#21704=ADVANCED_FACE('',(#2923),#21066,.F.);
#21705=ADVANCED_FACE('',(#2924),#21067,.F.);
#21706=ADVANCED_FACE('',(#2925,#1925),#2324,.F.);
#21707=ADVANCED_FACE('',(#2926),#21068,.F.);
#21708=ADVANCED_FACE('',(#2927),#21069,.F.);
#21709=ADVANCED_FACE('',(#2928),#2325,.F.);
#21710=ADVANCED_FACE('',(#2929),#21070,.F.);
#21711=ADVANCED_FACE('',(#2930),#2326,.F.);
#21712=ADVANCED_FACE('',(#2931),#2327,.T.);
#21713=ADVANCED_FACE('',(#2932,#1926,#1927,#1928,#1929),#2328,.T.);
#21714=ADVANCED_FACE('',(#2933),#2329,.T.);
#21715=ADVANCED_FACE('',(#2934,#1930,#1931,#1932,#1933),#2330,.T.);
#21716=ADVANCED_FACE('',(#2935),#2331,.T.);
#21717=ADVANCED_FACE('',(#2936,#1934,#1935),#2332,.F.);
#21718=ADVANCED_FACE('',(#2937),#21071,.F.);
#21719=ADVANCED_FACE('',(#2938),#21072,.F.);
#21720=ADVANCED_FACE('',(#2939),#21073,.F.);
#21721=ADVANCED_FACE('',(#2940),#21074,.T.);
#21722=ADVANCED_FACE('',(#2941,#1936),#2333,.T.);
#21723=ADVANCED_FACE('',(#2942),#21075,.F.);
#21724=ADVANCED_FACE('',(#2943),#21076,.T.);
#21725=ADVANCED_FACE('',(#2944,#1937,#1938,#1939,#1940),#2334,.T.);
#21726=ADVANCED_FACE('',(#2945,#1941,#1942,#1943,#1944),#2335,.F.);
#21727=ADVANCED_FACE('',(#2946),#21077,.F.);
#21728=ADVANCED_FACE('',(#2947),#21078,.F.);
#21729=ADVANCED_FACE('',(#2948),#21079,.F.);
#21730=ADVANCED_FACE('',(#2949),#21080,.F.);
#21731=ADVANCED_FACE('',(#2950,#1945),#2336,.T.);
#21732=ADVANCED_FACE('',(#2951),#21081,.F.);
#21733=ADVANCED_FACE('',(#2952),#21082,.F.);
#21734=ADVANCED_FACE('',(#2953),#2337,.F.);
#21735=ADVANCED_FACE('',(#2954),#21083,.F.);
#21736=ADVANCED_FACE('',(#2955),#2338,.F.);
#21737=ADVANCED_FACE('',(#2956),#2339,.T.);
#21738=ADVANCED_FACE('',(#2957,#1946,#1947,#1948,#1949),#2340,.T.);
#21739=ADVANCED_FACE('',(#2958),#2341,.T.);
#21740=ADVANCED_FACE('',(#2959,#1950,#1951,#1952,#1953),#2342,.T.);
#21741=ADVANCED_FACE('',(#2960),#2343,.T.);
#21742=ADVANCED_FACE('',(#2961,#1954,#1955),#2344,.F.);
#21743=ADVANCED_FACE('',(#2962),#21084,.F.);
#21744=ADVANCED_FACE('',(#2963),#21085,.F.);
#21745=ADVANCED_FACE('',(#2964),#21086,.F.);
#21746=ADVANCED_FACE('',(#2965),#2345,.F.);
#21747=ADVANCED_FACE('',(#2966,#1956,#1957,#1958,#1959),#2346,.F.);
#21748=ADVANCED_FACE('',(#2967),#21087,.T.);
#21749=ADVANCED_FACE('',(#2968),#21088,.T.);
#21750=ADVANCED_FACE('',(#2969,#1960),#2347,.F.);
#21751=ADVANCED_FACE('',(#2970),#21089,.F.);
#21752=ADVANCED_FACE('',(#2971,#1961,#1962,#1963,#1964),#2348,.T.);
#21753=ADVANCED_FACE('',(#2972),#21090,.F.);
#21754=ADVANCED_FACE('',(#2973,#1965),#2349,.T.);
#21755=ADVANCED_FACE('',(#2974),#21091,.F.);
#21756=ADVANCED_FACE('',(#2975),#2350,.T.);
#21757=ADVANCED_FACE('',(#2976),#2351,.T.);
#21758=ADVANCED_FACE('',(#2977),#2352,.T.);
#21759=ADVANCED_FACE('',(#2978),#2353,.T.);
#21760=ADVANCED_FACE('',(#2979,#1966),#2354,.T.);
#21761=ADVANCED_FACE('',(#2980,#1967),#2355,.F.);
#21762=ADVANCED_FACE('',(#2981),#21092,.F.);
#21763=ADVANCED_FACE('',(#2982,#1968),#2356,.T.);
#21764=ADVANCED_FACE('',(#2983),#21093,.F.);
#21765=ADVANCED_FACE('',(#2984),#2357,.T.);
#21766=ADVANCED_FACE('',(#2985),#2358,.T.);
#21767=ADVANCED_FACE('',(#2986),#2359,.T.);
#21768=ADVANCED_FACE('',(#2987),#2360,.T.);
#21769=ADVANCED_FACE('',(#2988,#1969),#2361,.T.);
#21770=ADVANCED_FACE('',(#2989,#1970),#2362,.F.);
#21771=ADVANCED_FACE('',(#2990),#21094,.F.);
#21772=ADVANCED_FACE('',(#2991,#1971),#2363,.T.);
#21773=ADVANCED_FACE('',(#2992),#21095,.F.);
#21774=ADVANCED_FACE('',(#2993,#1972),#2364,.T.);
#21775=ADVANCED_FACE('',(#2994),#21096,.F.);
#21776=ADVANCED_FACE('',(#2995,#1973),#2365,.T.);
#21777=ADVANCED_FACE('',(#2996),#21097,.F.);
#21778=ADVANCED_FACE('',(#2997,#1974),#2366,.T.);
#21779=ADVANCED_FACE('',(#2998),#21098,.F.);
#21780=ADVANCED_FACE('',(#2999),#21099,.F.);
#21781=ADVANCED_FACE('',(#3000),#21100,.F.);
#21782=ADVANCED_FACE('',(#3001),#21101,.F.);
#21783=ADVANCED_FACE('',(#3002),#2367,.T.);
#21784=ADVANCED_FACE('',(#3003),#2368,.T.);
#21785=ADVANCED_FACE('',(#3004),#2369,.T.);
#21786=ADVANCED_FACE('',(#3005),#2370,.T.);
#21787=ADVANCED_FACE('',(#3006,#1975,#1976,#1977,#1978),#2371,.T.);
#21788=ADVANCED_FACE('',(#3007),#2372,.T.);
#21789=ADVANCED_FACE('',(#3008),#2373,.T.);
#21790=ADVANCED_FACE('',(#3009),#2374,.T.);
#21791=ADVANCED_FACE('',(#3010),#2375,.T.);
#21792=ADVANCED_FACE('',(#3011),#2376,.T.);
#21793=ADVANCED_FACE('',(#3012,#1979,#1980,#1981,#1982),#2377,.T.);
#21794=ADVANCED_FACE('',(#3013),#2378,.T.);
#21795=ADVANCED_FACE('',(#3014),#2379,.T.);
#21796=ADVANCED_FACE('',(#3015),#2380,.F.);
#21797=ADVANCED_FACE('',(#3016),#1496,.F.);
#21798=ADVANCED_FACE('',(#3017),#21102,.T.);
#21799=ADVANCED_FACE('',(#3018),#21103,.F.);
#21800=ADVANCED_FACE('',(#3019),#1441,.F.);
#21801=ADVANCED_FACE('',(#3020,#1983),#2381,.T.);
#21802=ADVANCED_FACE('',(#3021),#21104,.T.);
#21803=ADVANCED_FACE('',(#3022,#1984),#2382,.T.);
#21804=ADVANCED_FACE('',(#3023),#1442,.F.);
#21805=ADVANCED_FACE('',(#3024),#1497,.F.);
#21806=ADVANCED_FACE('',(#3025),#21105,.F.);
#21807=ADVANCED_FACE('',(#3026,#1985),#2383,.T.);
#21808=ADVANCED_FACE('',(#3027),#1443,.T.);
#21809=ADVANCED_FACE('',(#3028),#21106,.T.);
#21810=ADVANCED_FACE('',(#3029),#1444,.T.);
#21811=ADVANCED_FACE('',(#3030,#1986),#2384,.T.);
#21812=ADVANCED_FACE('',(#3031),#21107,.F.);
#21813=ADVANCED_FACE('',(#3032),#1381,.T.);
#21814=ADVANCED_FACE('',(#3033),#1382,.T.);
#21815=ADVANCED_FACE('',(#3034),#1383,.T.);
#21816=ADVANCED_FACE('',(#3035),#1384,.T.);
#21817=ADVANCED_FACE('',(#3036),#1385,.T.);
#21818=ADVANCED_FACE('',(#3037),#1386,.T.);
#21819=ADVANCED_FACE('',(#3038),#1387,.T.);
#21820=ADVANCED_FACE('',(#3039),#1388,.F.);
#21821=ADVANCED_FACE('',(#3040),#21108,.T.);
#21822=ADVANCED_FACE('',(#3041),#2385,.T.);
#21823=ADVANCED_FACE('',(#3042),#1389,.F.);
#21824=ADVANCED_FACE('',(#3043),#2386,.T.);
#21825=ADVANCED_FACE('',(#3044),#1390,.F.);
#21826=ADVANCED_FACE('',(#3045),#2387,.T.);
#21827=ADVANCED_FACE('',(#3046),#1391,.F.);
#21828=ADVANCED_FACE('',(#3047),#2388,.T.);
#21829=ADVANCED_FACE('',(#3048),#1392,.F.);
#21830=ADVANCED_FACE('',(#3049),#2389,.T.);
#21831=ADVANCED_FACE('',(#3050),#1393,.F.);
#21832=ADVANCED_FACE('',(#3051),#21109,.F.);
#21833=ADVANCED_FACE('',(#3052),#2390,.T.);
#21834=ADVANCED_FACE('',(#3053),#1394,.F.);
#21835=ADVANCED_FACE('',(#3054,#1987),#2391,.T.);
#21836=ADVANCED_FACE('',(#3055),#2392,.T.);
#21837=ADVANCED_FACE('',(#3056,#1988),#2393,.T.);
#21838=ADVANCED_FACE('',(#3057),#21110,.T.);
#21839=ADVANCED_FACE('',(#3058,#1989),#2394,.T.);
#21840=ADVANCED_FACE('',(#3059),#21111,.F.);
#21841=ADVANCED_FACE('',(#3060,#1990),#2395,.T.);
#21842=ADVANCED_FACE('',(#3061),#21112,.T.);
#21843=ADVANCED_FACE('',(#3062,#1991),#2396,.T.);
#21844=ADVANCED_FACE('',(#3063),#21113,.F.);
#21845=ADVANCED_FACE('',(#3064),#1498,.F.);
#21846=ADVANCED_FACE('',(#3065),#21114,.T.);
#21847=ADVANCED_FACE('',(#3066),#21115,.F.);
#21848=ADVANCED_FACE('',(#3067),#1445,.F.);
#21849=ADVANCED_FACE('',(#3068,#1992),#2397,.T.);
#21850=ADVANCED_FACE('',(#3069),#21116,.T.);
#21851=ADVANCED_FACE('',(#3070,#1993),#2398,.T.);
#21852=ADVANCED_FACE('',(#3071),#1446,.F.);
#21853=ADVANCED_FACE('',(#3072),#1499,.F.);
#21854=ADVANCED_FACE('',(#3073),#21117,.F.);
#21855=ADVANCED_FACE('',(#3074,#1994),#2399,.T.);
#21856=ADVANCED_FACE('',(#3075),#1447,.T.);
#21857=ADVANCED_FACE('',(#3076),#21118,.T.);
#21858=ADVANCED_FACE('',(#3077),#1448,.T.);
#21859=ADVANCED_FACE('',(#3078,#1995),#2400,.T.);
#21860=ADVANCED_FACE('',(#3079),#21119,.F.);
#21861=ADVANCED_FACE('',(#3080),#1395,.T.);
#21862=ADVANCED_FACE('',(#3081),#1396,.T.);
#21863=ADVANCED_FACE('',(#3082),#1397,.T.);
#21864=ADVANCED_FACE('',(#3083),#1398,.T.);
#21865=ADVANCED_FACE('',(#3084),#1399,.T.);
#21866=ADVANCED_FACE('',(#3085),#1400,.T.);
#21867=ADVANCED_FACE('',(#3086),#1401,.T.);
#21868=ADVANCED_FACE('',(#3087),#1402,.T.);
#21869=ADVANCED_FACE('',(#3088),#1403,.F.);
#21870=ADVANCED_FACE('',(#3089),#21120,.T.);
#21871=ADVANCED_FACE('',(#3090),#2401,.T.);
#21872=ADVANCED_FACE('',(#3091),#1404,.F.);
#21873=ADVANCED_FACE('',(#3092),#2402,.T.);
#21874=ADVANCED_FACE('',(#3093),#1405,.F.);
#21875=ADVANCED_FACE('',(#3094),#2403,.T.);
#21876=ADVANCED_FACE('',(#3095),#1406,.F.);
#21877=ADVANCED_FACE('',(#3096),#2404,.T.);
#21878=ADVANCED_FACE('',(#3097),#1407,.F.);
#21879=ADVANCED_FACE('',(#3098),#2405,.T.);
#21880=ADVANCED_FACE('',(#3099),#1408,.F.);
#21881=ADVANCED_FACE('',(#3100),#2406,.T.);
#21882=ADVANCED_FACE('',(#3101),#1409,.F.);
#21883=ADVANCED_FACE('',(#3102),#21121,.F.);
#21884=ADVANCED_FACE('',(#3103),#2407,.T.);
#21885=ADVANCED_FACE('',(#3104),#1410,.F.);
#21886=ADVANCED_FACE('',(#3105,#1996),#2408,.T.);
#21887=ADVANCED_FACE('',(#3106),#2409,.T.);
#21888=ADVANCED_FACE('',(#3107,#1997),#2410,.T.);
#21889=ADVANCED_FACE('',(#3108),#21122,.T.);
#21890=ADVANCED_FACE('',(#3109,#1998),#2411,.T.);
#21891=ADVANCED_FACE('',(#3110),#21123,.F.);
#21892=ADVANCED_FACE('',(#3111,#1999),#2412,.T.);
#21893=ADVANCED_FACE('',(#3112),#21124,.T.);
#21894=ADVANCED_FACE('',(#3113,#2000),#2413,.T.);
#21895=ADVANCED_FACE('',(#3114),#21125,.F.);
#21896=ADVANCED_FACE('',(#3115),#21126,.F.);
#21897=ADVANCED_FACE('',(#3116),#21127,.F.);
#21898=ADVANCED_FACE('',(#3117),#21128,.F.);
#21899=ADVANCED_FACE('',(#3118),#21129,.F.);
#21900=ADVANCED_FACE('',(#3119),#2414,.T.);
#21901=ADVANCED_FACE('',(#3120),#2415,.T.);
#21902=ADVANCED_FACE('',(#3121),#2416,.T.);
#21903=ADVANCED_FACE('',(#3122),#2417,.T.);
#21904=ADVANCED_FACE('',(#3123,#2001,#2002,#2003,#2004),#2418,.T.);
#21905=ADVANCED_FACE('',(#3124,#2005,#2006,#2007,#2008),#2419,.F.);
#21906=ADVANCED_FACE('',(#3125),#21130,.F.);
#21907=ADVANCED_FACE('',(#3126),#21131,.F.);
#21908=ADVANCED_FACE('',(#3127),#21132,.F.);
#21909=ADVANCED_FACE('',(#3128),#21133,.F.);
#21910=ADVANCED_FACE('',(#3129),#21134,.F.);
#21911=ADVANCED_FACE('',(#3130),#21135,.F.);
#21912=ADVANCED_FACE('',(#3131),#21136,.F.);
#21913=ADVANCED_FACE('',(#3132),#21137,.F.);
#21914=ADVANCED_FACE('',(#3133),#21138,.F.);
#21915=ADVANCED_FACE('',(#3134),#21139,.F.);
#21916=ADVANCED_FACE('',(#3135),#21140,.F.);
#21917=ADVANCED_FACE('',(#3136),#21141,.F.);
#21918=ADVANCED_FACE('',(#3137),#2420,.T.);
#21919=ADVANCED_FACE('',(#3138),#2421,.T.);
#21920=ADVANCED_FACE('',(#3139),#2422,.T.);
#21921=ADVANCED_FACE('',(#3140),#2423,.T.);
#21922=ADVANCED_FACE('',(#3141,#2009,#2010,#2011,#2012,#2013,#2014,#2015,
#2016,#2017,#2018,#2019,#2020),#2424,.T.);
#21923=ADVANCED_FACE('',(#3142,#2021,#2022,#2023,#2024,#2025,#2026,#2027,
#2028,#2029,#2030,#2031,#2032),#2425,.F.);
#21924=ADVANCED_FACE('',(#3143),#21142,.F.);
#21925=ADVANCED_FACE('',(#3144),#2426,.T.);
#21926=ADVANCED_FACE('',(#3145),#21143,.F.);
#21927=ADVANCED_FACE('',(#3146),#2427,.T.);
#21928=ADVANCED_FACE('',(#3147),#21144,.F.);
#21929=ADVANCED_FACE('',(#3148),#2428,.T.);
#21930=ADVANCED_FACE('',(#3149),#21145,.F.);
#21931=ADVANCED_FACE('',(#3150),#2429,.T.);
#21932=ADVANCED_FACE('',(#3151),#21146,.F.);
#21933=ADVANCED_FACE('',(#3152),#2430,.T.);
#21934=ADVANCED_FACE('',(#3153),#21147,.F.);
#21935=ADVANCED_FACE('',(#3154),#2431,.T.);
#21936=ADVANCED_FACE('',(#3155),#21148,.F.);
#21937=ADVANCED_FACE('',(#3156),#2432,.T.);
#21938=ADVANCED_FACE('',(#3157),#21149,.F.);
#21939=ADVANCED_FACE('',(#3158),#2433,.T.);
#21940=ADVANCED_FACE('',(#3159,#2033,#2034,#2035,#2036),#2434,.T.);
#21941=ADVANCED_FACE('',(#3160),#2435,.T.);
#21942=ADVANCED_FACE('',(#3161,#2037),#2436,.T.);
#21943=ADVANCED_FACE('',(#3162,#2038,#2039,#2040,#2041),#2437,.T.);
#21944=ADVANCED_FACE('',(#3163),#2438,.F.);
#21945=ADVANCED_FACE('',(#3164),#2439,.T.);
#21946=ADVANCED_FACE('',(#3165),#21150,.F.);
#21947=ADVANCED_FACE('',(#3166),#2440,.T.);
#21948=ADVANCED_FACE('',(#3167),#21151,.F.);
#21949=ADVANCED_FACE('',(#3168),#2441,.T.);
#21950=ADVANCED_FACE('',(#3169),#21152,.F.);
#21951=ADVANCED_FACE('',(#3170),#2442,.T.);
#21952=ADVANCED_FACE('',(#3171),#21153,.F.);
#21953=ADVANCED_FACE('',(#3172),#2443,.T.);
#21954=ADVANCED_FACE('',(#3173),#2444,.T.);
#21955=ADVANCED_FACE('',(#3174),#2445,.T.);
#21956=ADVANCED_FACE('',(#3175),#2446,.T.);
#21957=ADVANCED_FACE('',(#3176),#2447,.T.);
#21958=ADVANCED_FACE('',(#3177,#2042,#2043,#2044,#2045),#2448,.T.);
#21959=ADVANCED_FACE('',(#3178),#2449,.T.);
#21960=ADVANCED_FACE('',(#3179),#2450,.T.);
#21961=ADVANCED_FACE('',(#3180),#2451,.T.);
#21962=ADVANCED_FACE('',(#3181),#2452,.T.);
#21963=ADVANCED_FACE('',(#3182),#2453,.T.);
#21964=ADVANCED_FACE('',(#3183),#2454,.T.);
#21965=ADVANCED_FACE('',(#3184),#2455,.T.);
#21966=ADVANCED_FACE('',(#3185),#2456,.T.);
#21967=ADVANCED_FACE('',(#3186),#2457,.T.);
#21968=ADVANCED_FACE('',(#3187),#2458,.T.);
#21969=ADVANCED_FACE('',(#3188),#2459,.T.);
#21970=ADVANCED_FACE('',(#3189),#2460,.T.);
#21971=ADVANCED_FACE('',(#3190),#2461,.T.);
#21972=ADVANCED_FACE('',(#3191),#2462,.T.);
#21973=ADVANCED_FACE('',(#3192),#2463,.T.);
#21974=ADVANCED_FACE('',(#3193),#2464,.T.);
#21975=ADVANCED_FACE('',(#3194),#2465,.T.);
#21976=ADVANCED_FACE('',(#3195),#2466,.F.);
#21977=ADVANCED_FACE('',(#3196),#2467,.T.);
#21978=ADVANCED_FACE('',(#3197),#2468,.T.);
#21979=ADVANCED_FACE('',(#3198),#2469,.T.);
#21980=ADVANCED_FACE('',(#3199),#2470,.T.);
#21981=ADVANCED_FACE('',(#3200),#2471,.T.);
#21982=ADVANCED_FACE('',(#3201),#2472,.T.);
#21983=ADVANCED_FACE('',(#3202),#2473,.T.);
#21984=ADVANCED_FACE('',(#3203),#2474,.T.);
#21985=ADVANCED_FACE('',(#3204),#2475,.T.);
#21986=ADVANCED_FACE('',(#3205),#2476,.T.);
#21987=ADVANCED_FACE('',(#3206),#1449,.F.);
#21988=ADVANCED_FACE('',(#3207),#21154,.F.);
#21989=ADVANCED_FACE('',(#3208,#2046),#2477,.T.);
#21990=ADVANCED_FACE('',(#3209),#21155,.T.);
#21991=ADVANCED_FACE('',(#3210,#2047),#2478,.F.);
#21992=ADVANCED_FACE('',(#3211),#2479,.F.);
#21993=ADVANCED_FACE('',(#3212),#2480,.F.);
#21994=ADVANCED_FACE('',(#3213),#2481,.F.);
#21995=ADVANCED_FACE('',(#3214),#2482,.F.);
#21996=ADVANCED_FACE('',(#3215),#2483,.F.);
#21997=ADVANCED_FACE('',(#3216),#2484,.F.);
#21998=ADVANCED_FACE('',(#3217),#2485,.F.);
#21999=ADVANCED_FACE('',(#3218),#2486,.F.);
#22000=ADVANCED_FACE('',(#3219,#2048),#2487,.T.);
#22001=ADVANCED_FACE('',(#3220),#21156,.T.);
#22002=ADVANCED_FACE('',(#3221),#2488,.F.);
#22003=ADVANCED_FACE('',(#3222),#2489,.T.);
#22004=ADVANCED_FACE('',(#3223),#1450,.T.);
#22005=ADVANCED_FACE('',(#3224),#21157,.T.);
#22006=ADVANCED_FACE('',(#3225),#1451,.T.);
#22007=ADVANCED_FACE('',(#3226,#2049),#2490,.T.);
#22008=ADVANCED_FACE('',(#3227),#1452,.T.);
#22009=ADVANCED_FACE('',(#3228),#21158,.T.);
#22010=ADVANCED_FACE('',(#3229),#21159,.F.);
#22011=ADVANCED_FACE('',(#3230),#21160,.F.);
#22012=ADVANCED_FACE('',(#3231),#21161,.F.);
#22013=ADVANCED_FACE('',(#3232),#21162,.F.);
#22014=ADVANCED_FACE('',(#3233),#21163,.F.);
#22015=ADVANCED_FACE('',(#3234),#21164,.F.);
#22016=ADVANCED_FACE('',(#3235),#21165,.F.);
#22017=ADVANCED_FACE('',(#3236),#21166,.F.);
#22018=ADVANCED_FACE('',(#3237),#21167,.F.);
#22019=ADVANCED_FACE('',(#3238),#21168,.F.);
#22020=ADVANCED_FACE('',(#3239),#21169,.F.);
#22021=ADVANCED_FACE('',(#3240),#21170,.F.);
#22022=ADVANCED_FACE('',(#3241),#21171,.F.);
#22023=ADVANCED_FACE('',(#3242),#21172,.F.);
#22024=ADVANCED_FACE('',(#3243),#21173,.F.);
#22025=ADVANCED_FACE('',(#3244),#21174,.F.);
#22026=ADVANCED_FACE('',(#3245),#21175,.F.);
#22027=ADVANCED_FACE('',(#3246),#21176,.F.);
#22028=ADVANCED_FACE('',(#3247),#21177,.F.);
#22029=ADVANCED_FACE('',(#3248),#11,.F.);
#22030=ADVANCED_FACE('',(#3249),#12,.F.);
#22031=ADVANCED_FACE('',(#3250,#2050,#2051,#2052,#2053),#2491,.T.);
#22032=ADVANCED_FACE('',(#3251),#21178,.F.);
#22033=ADVANCED_FACE('',(#3252),#21179,.F.);
#22034=ADVANCED_FACE('',(#3253),#21180,.F.);
#22035=ADVANCED_FACE('',(#3254),#2492,.F.);
#22036=ADVANCED_FACE('',(#3255,#2054,#2055,#2056,#2057),#2493,.F.);
#22037=ADVANCED_FACE('',(#3256),#21181,.T.);
#22038=ADVANCED_FACE('',(#3257),#21182,.F.);
#22039=ADVANCED_FACE('',(#3258),#21183,.T.);
#22040=ADVANCED_FACE('',(#3259,#2058),#2494,.F.);
#22041=ADVANCED_FACE('',(#3260),#2495,.T.);
#22042=ADVANCED_FACE('',(#3261),#1453,.T.);
#22043=ADVANCED_FACE('',(#3262),#21184,.T.);
#22044=ADVANCED_FACE('',(#3263),#1454,.T.);
#22045=ADVANCED_FACE('',(#3264,#2059),#2496,.T.);
#22046=ADVANCED_FACE('',(#3265),#1455,.T.);
#22047=ADVANCED_FACE('',(#3266),#21185,.T.);
#22048=ADVANCED_FACE('',(#3267),#1456,.T.);
#22049=ADVANCED_FACE('',(#3268),#2497,.T.);
#22050=ADVANCED_FACE('',(#3269),#2498,.F.);
#22051=ADVANCED_FACE('',(#3270),#2499,.F.);
#22052=ADVANCED_FACE('',(#3271),#2500,.F.);
#22053=ADVANCED_FACE('',(#3272),#2501,.F.);
#22054=ADVANCED_FACE('',(#3273),#2502,.F.);
#22055=ADVANCED_FACE('',(#3274),#2503,.F.);
#22056=ADVANCED_FACE('',(#3275),#2504,.F.);
#22057=ADVANCED_FACE('',(#3276),#2505,.F.);
#22058=ADVANCED_FACE('',(#3277),#2506,.T.);
#22059=ADVANCED_FACE('',(#3278),#1457,.T.);
#22060=ADVANCED_FACE('',(#3279),#21186,.T.);
#22061=ADVANCED_FACE('',(#3280),#1458,.T.);
#22062=ADVANCED_FACE('',(#3281,#2060),#2507,.T.);
#22063=ADVANCED_FACE('',(#3282),#1459,.T.);
#22064=ADVANCED_FACE('',(#3283),#21187,.T.);
#22065=ADVANCED_FACE('',(#3284),#1460,.T.);
#22066=ADVANCED_FACE('',(#3285),#2508,.T.);
#22067=ADVANCED_FACE('',(#3286),#2509,.F.);
#22068=ADVANCED_FACE('',(#3287),#2510,.F.);
#22069=ADVANCED_FACE('',(#3288),#2511,.F.);
#22070=ADVANCED_FACE('',(#3289),#2512,.F.);
#22071=ADVANCED_FACE('',(#3290),#2513,.F.);
#22072=ADVANCED_FACE('',(#3291),#2514,.F.);
#22073=ADVANCED_FACE('',(#3292),#2515,.F.);
#22074=ADVANCED_FACE('',(#3293),#2516,.F.);
#22075=ADVANCED_FACE('',(#3294),#21188,.T.);
#22076=ADVANCED_FACE('',(#3295),#21189,.T.);
#22077=ADVANCED_FACE('',(#3296),#21190,.T.);
#22078=ADVANCED_FACE('',(#3297),#21191,.T.);
#22079=ADVANCED_FACE('',(#3298),#21192,.T.);
#22080=ADVANCED_FACE('',(#3299),#21193,.T.);
#22081=ADVANCED_FACE('',(#3300),#21194,.T.);
#22082=ADVANCED_FACE('',(#3301),#21195,.T.);
#22083=ADVANCED_FACE('',(#3302),#21196,.T.);
#22084=ADVANCED_FACE('',(#3303),#21197,.T.);
#22085=ADVANCED_FACE('',(#3304),#21198,.T.);
#22086=ADVANCED_FACE('',(#3305),#21199,.T.);
#22087=ADVANCED_FACE('',(#3306),#21200,.T.);
#22088=ADVANCED_FACE('',(#3307),#21201,.T.);
#22089=ADVANCED_FACE('',(#3308),#21202,.T.);
#22090=ADVANCED_FACE('',(#3309),#21203,.T.);
#22091=ADVANCED_FACE('',(#3310),#21204,.T.);
#22092=ADVANCED_FACE('',(#3311),#21205,.T.);
#22093=ADVANCED_FACE('',(#3312),#21206,.T.);
#22094=ADVANCED_FACE('',(#3313),#21207,.T.);
#22095=ADVANCED_FACE('',(#3314),#21208,.T.);
#22096=ADVANCED_FACE('',(#3315),#21209,.T.);
#22097=ADVANCED_FACE('',(#3316),#21210,.T.);
#22098=ADVANCED_FACE('',(#3317),#21211,.T.);
#22099=ADVANCED_FACE('',(#3318),#21212,.T.);
#22100=ADVANCED_FACE('',(#3319),#21213,.T.);
#22101=ADVANCED_FACE('',(#3320),#21214,.T.);
#22102=ADVANCED_FACE('',(#3321),#21215,.T.);
#22103=ADVANCED_FACE('',(#3322),#21216,.T.);
#22104=ADVANCED_FACE('',(#3323),#21217,.T.);
#22105=ADVANCED_FACE('',(#3324),#21218,.T.);
#22106=ADVANCED_FACE('',(#3325),#21219,.T.);
#22107=ADVANCED_FACE('',(#3326),#21220,.T.);
#22108=ADVANCED_FACE('',(#3327),#21221,.T.);
#22109=ADVANCED_FACE('',(#3328),#21222,.T.);
#22110=ADVANCED_FACE('',(#3329),#21223,.T.);
#22111=ADVANCED_FACE('',(#3330),#21224,.T.);
#22112=ADVANCED_FACE('',(#3331),#21225,.T.);
#22113=ADVANCED_FACE('',(#3332),#21226,.T.);
#22114=ADVANCED_FACE('',(#3333),#21227,.T.);
#22115=ADVANCED_FACE('',(#3334),#21228,.T.);
#22116=ADVANCED_FACE('',(#3335),#21229,.T.);
#22117=ADVANCED_FACE('',(#3336),#21230,.T.);
#22118=ADVANCED_FACE('',(#3337),#21231,.T.);
#22119=ADVANCED_FACE('',(#3338),#21232,.T.);
#22120=ADVANCED_FACE('',(#3339),#21233,.T.);
#22121=ADVANCED_FACE('',(#3340),#21234,.T.);
#22122=ADVANCED_FACE('',(#3341),#21235,.T.);
#22123=ADVANCED_FACE('',(#3342),#21236,.T.);
#22124=ADVANCED_FACE('',(#3343),#21237,.T.);
#22125=ADVANCED_FACE('',(#3344),#21238,.T.);
#22126=ADVANCED_FACE('',(#3345),#21239,.T.);
#22127=ADVANCED_FACE('',(#3346),#21240,.T.);
#22128=ADVANCED_FACE('',(#3347),#21241,.T.);
#22129=ADVANCED_FACE('',(#3348),#21242,.T.);
#22130=ADVANCED_FACE('',(#3349),#21243,.T.);
#22131=ADVANCED_FACE('',(#3350),#21244,.T.);
#22132=ADVANCED_FACE('',(#3351),#21245,.T.);
#22133=ADVANCED_FACE('',(#3352),#21246,.T.);
#22134=ADVANCED_FACE('',(#3353),#21247,.T.);
#22135=ADVANCED_FACE('',(#3354),#21248,.T.);
#22136=ADVANCED_FACE('',(#3355),#21249,.T.);
#22137=ADVANCED_FACE('',(#3356),#21250,.T.);
#22138=ADVANCED_FACE('',(#3357),#21251,.T.);
#22139=ADVANCED_FACE('',(#3358),#21252,.T.);
#22140=ADVANCED_FACE('',(#3359),#21253,.T.);
#22141=ADVANCED_FACE('',(#3360),#21254,.T.);
#22142=ADVANCED_FACE('',(#3361),#21255,.T.);
#22143=ADVANCED_FACE('',(#3362),#21256,.T.);
#22144=ADVANCED_FACE('',(#3363),#21257,.T.);
#22145=ADVANCED_FACE('',(#3364),#21258,.T.);
#22146=ADVANCED_FACE('',(#3365),#21259,.T.);
#22147=ADVANCED_FACE('',(#3366),#21260,.T.);
#22148=ADVANCED_FACE('',(#3367),#21261,.T.);
#22149=ADVANCED_FACE('',(#3368),#21262,.T.);
#22150=ADVANCED_FACE('',(#3369),#21263,.T.);
#22151=ADVANCED_FACE('',(#3370),#21264,.T.);
#22152=ADVANCED_FACE('',(#3371),#21265,.T.);
#22153=ADVANCED_FACE('',(#3372),#21266,.T.);
#22154=ADVANCED_FACE('',(#3373),#21267,.T.);
#22155=ADVANCED_FACE('',(#3374),#21268,.T.);
#22156=ADVANCED_FACE('',(#3375),#21269,.T.);
#22157=ADVANCED_FACE('',(#3376),#21270,.T.);
#22158=ADVANCED_FACE('',(#3377),#21271,.T.);
#22159=ADVANCED_FACE('',(#3378),#21272,.T.);
#22160=ADVANCED_FACE('',(#3379),#21273,.T.);
#22161=ADVANCED_FACE('',(#3380),#21274,.T.);
#22162=ADVANCED_FACE('',(#3381),#21275,.T.);
#22163=ADVANCED_FACE('',(#3382),#21276,.T.);
#22164=ADVANCED_FACE('',(#3383),#21277,.T.);
#22165=ADVANCED_FACE('',(#3384),#21278,.T.);
#22166=ADVANCED_FACE('',(#3385),#21279,.T.);
#22167=ADVANCED_FACE('',(#3386),#21280,.T.);
#22168=ADVANCED_FACE('',(#3387),#21281,.T.);
#22169=ADVANCED_FACE('',(#3388),#21282,.T.);
#22170=ADVANCED_FACE('',(#3389),#21283,.T.);
#22171=ADVANCED_FACE('',(#3390),#21284,.T.);
#22172=ADVANCED_FACE('',(#3391),#21285,.T.);
#22173=ADVANCED_FACE('',(#3392),#21286,.T.);
#22174=ADVANCED_FACE('',(#3393),#21287,.T.);
#22175=ADVANCED_FACE('',(#3394),#21288,.T.);
#22176=ADVANCED_FACE('',(#3395),#21289,.T.);
#22177=ADVANCED_FACE('',(#3396),#21290,.T.);
#22178=ADVANCED_FACE('',(#3397),#21291,.T.);
#22179=ADVANCED_FACE('',(#3398),#21292,.T.);
#22180=ADVANCED_FACE('',(#3399),#21293,.T.);
#22181=ADVANCED_FACE('',(#3400),#21294,.T.);
#22182=ADVANCED_FACE('',(#3401),#21295,.T.);
#22183=ADVANCED_FACE('',(#3402),#21296,.T.);
#22184=ADVANCED_FACE('',(#3403),#21297,.T.);
#22185=ADVANCED_FACE('',(#3404),#21298,.T.);
#22186=ADVANCED_FACE('',(#3405),#21299,.T.);
#22187=ADVANCED_FACE('',(#3406),#21300,.T.);
#22188=ADVANCED_FACE('',(#3407),#21301,.T.);
#22189=ADVANCED_FACE('',(#3408),#21302,.T.);
#22190=ADVANCED_FACE('',(#3409),#21303,.T.);
#22191=ADVANCED_FACE('',(#3410),#21304,.T.);
#22192=ADVANCED_FACE('',(#3411),#21305,.T.);
#22193=ADVANCED_FACE('',(#3412),#21306,.T.);
#22194=ADVANCED_FACE('',(#3413),#21307,.T.);
#22195=ADVANCED_FACE('',(#3414),#21308,.T.);
#22196=ADVANCED_FACE('',(#3415),#21309,.T.);
#22197=ADVANCED_FACE('',(#3416),#21310,.T.);
#22198=ADVANCED_FACE('',(#3417),#21311,.T.);
#22199=ADVANCED_FACE('',(#3418),#21312,.T.);
#22200=ADVANCED_FACE('',(#3419),#21313,.T.);
#22201=ADVANCED_FACE('',(#3420,#2061),#2517,.T.);
#22202=ADVANCED_FACE('',(#3421),#21314,.T.);
#22203=ADVANCED_FACE('',(#3422),#2518,.F.);
#22204=ADVANCED_FACE('',(#3423),#13,.F.);
#22205=ADVANCED_FACE('',(#3424),#21315,.T.);
#22206=ADVANCED_FACE('',(#3425),#14,.F.);
#22207=ADVANCED_FACE('',(#3426),#2519,.F.);
#22208=ADVANCED_FACE('',(#3427),#2520,.T.);
#22209=ADVANCED_FACE('',(#3428),#2521,.F.);
#22210=ADVANCED_FACE('',(#3429),#2522,.F.);
#22211=ADVANCED_FACE('',(#3430),#2523,.F.);
#22212=ADVANCED_FACE('',(#3431,#2062),#21316,.T.);
#22213=ADVANCED_FACE('',(#3432),#2524,.T.);
#22214=ADVANCED_FACE('',(#3433,#2063),#2525,.F.);
#22215=ADVANCED_FACE('',(#3434),#21317,.T.);
#22216=ADVANCED_FACE('',(#3435,#2064),#2526,.T.);
#22217=ADVANCED_FACE('',(#3436),#21318,.T.);
#22218=ADVANCED_FACE('',(#3437),#21319,.F.);
#22219=ADVANCED_FACE('',(#3438),#21320,.T.);
#22220=ADVANCED_FACE('',(#3439,#2065),#2527,.T.);
#22221=ADVANCED_FACE('',(#3440,#2066),#2528,.F.);
#22222=ADVANCED_FACE('',(#3441),#2529,.T.);
#22223=ADVANCED_FACE('',(#3442),#21321,.F.);
#22224=ADVANCED_FACE('',(#3443),#2530,.T.);
#22225=ADVANCED_FACE('',(#3444,#2067),#21322,.F.);
#22226=ADVANCED_FACE('',(#3445,#2068),#21323,.T.);
#22227=ADVANCED_FACE('',(#3446,#2069),#2531,.T.);
#22228=ADVANCED_FACE('',(#3447,#2070),#2532,.F.);
#22229=ADVANCED_FACE('',(#3448),#21324,.F.);
#22230=ADVANCED_FACE('',(#3449),#2533,.T.);
#22231=ADVANCED_FACE('',(#3450),#21325,.F.);
#22232=ADVANCED_FACE('',(#3451),#2534,.T.);
#22233=ADVANCED_FACE('',(#3452),#2535,.F.);
#22234=ADVANCED_FACE('',(#3453),#2536,.F.);
#22235=ADVANCED_FACE('',(#3454),#2537,.F.);
#22236=ADVANCED_FACE('',(#3455,#2071,#2072),#2538,.T.);
#22237=ADVANCED_FACE('',(#3456,#2073,#2074),#2539,.F.);
#22238=ADVANCED_FACE('',(#3457),#21326,.T.);
#22239=ADVANCED_FACE('',(#3458,#2075),#21327,.F.);
#22240=ADVANCED_FACE('',(#3459,#2076),#21328,.T.);
#22241=ADVANCED_FACE('',(#3460),#2540,.F.);
#22242=ADVANCED_FACE('',(#3461),#21329,.F.);
#22243=ADVANCED_FACE('',(#3462),#21330,.T.);
#22244=ADVANCED_FACE('',(#3463,#2077),#2541,.T.);
#22245=ADVANCED_FACE('',(#3464,#2078),#2542,.F.);
#22246=ADVANCED_FACE('',(#3465),#21331,.F.);
#22247=ADVANCED_FACE('',(#3466),#21332,.T.);
#22248=ADVANCED_FACE('',(#3467,#2079),#2543,.T.);
#22249=ADVANCED_FACE('',(#3468,#2080),#2544,.F.);
#22250=ADVANCED_FACE('',(#3469),#2545,.F.);
#22251=ADVANCED_FACE('',(#3470),#2546,.T.);
#22252=ADVANCED_FACE('',(#3471),#2547,.T.);
#22253=ADVANCED_FACE('',(#3472),#2548,.T.);
#22254=ADVANCED_FACE('',(#3473),#2549,.T.);
#22255=ADVANCED_FACE('',(#3474),#2550,.T.);
#22256=ADVANCED_FACE('',(#3475),#2551,.F.);
#22257=ADVANCED_FACE('',(#3476),#2552,.T.);
#22258=ADVANCED_FACE('',(#3477),#2553,.T.);
#22259=ADVANCED_FACE('',(#3478),#2554,.T.);
#22260=ADVANCED_FACE('',(#3479),#2555,.F.);
#22261=ADVANCED_FACE('',(#3480),#2556,.F.);
#22262=ADVANCED_FACE('',(#3481),#2557,.F.);
#22263=ADVANCED_FACE('',(#3482),#2558,.F.);
#22264=ADVANCED_FACE('',(#3483),#2559,.F.);
#22265=ADVANCED_FACE('',(#3484),#2560,.F.);
#22266=ADVANCED_FACE('',(#3485),#2561,.F.);
#22267=ADVANCED_FACE('',(#3486,#2081),#2562,.T.);
#22268=ADVANCED_FACE('',(#3487),#1461,.T.);
#22269=ADVANCED_FACE('',(#3488),#21333,.T.);
#22270=ADVANCED_FACE('',(#3489),#1462,.T.);
#22271=ADVANCED_FACE('',(#3490),#2563,.T.);
#22272=ADVANCED_FACE('',(#3491),#21334,.F.);
#22273=ADVANCED_FACE('',(#3492),#21335,.T.);
#22274=ADVANCED_FACE('',(#3493,#2082),#2564,.T.);
#22275=ADVANCED_FACE('',(#3494,#2083),#2565,.F.);
#22276=ADVANCED_FACE('',(#3495),#2566,.T.);
#22277=ADVANCED_FACE('',(#3496),#1463,.T.);
#22278=ADVANCED_FACE('',(#3497),#21336,.T.);
#22279=ADVANCED_FACE('',(#3498),#1464,.T.);
#22280=ADVANCED_FACE('',(#3499,#2084),#2567,.T.);
#22281=ADVANCED_FACE('',(#3500),#1465,.T.);
#22282=ADVANCED_FACE('',(#3501),#21337,.T.);
#22283=ADVANCED_FACE('',(#3502),#1466,.T.);
#22284=ADVANCED_FACE('',(#3503),#2568,.T.);
#22285=ADVANCED_FACE('',(#3504),#2569,.F.);
#22286=ADVANCED_FACE('',(#3505),#2570,.F.);
#22287=ADVANCED_FACE('',(#3506),#2571,.F.);
#22288=ADVANCED_FACE('',(#3507),#2572,.F.);
#22289=ADVANCED_FACE('',(#3508),#2573,.F.);
#22290=ADVANCED_FACE('',(#3509),#2574,.F.);
#22291=ADVANCED_FACE('',(#3510),#2575,.F.);
#22292=ADVANCED_FACE('',(#3511),#2576,.F.);
#22293=ADVANCED_FACE('',(#3512),#21338,.F.);
#22294=ADVANCED_FACE('',(#3513),#2577,.F.);
#22295=ADVANCED_FACE('',(#3514),#21339,.F.);
#22296=ADVANCED_FACE('',(#3515),#2578,.F.);
#22297=ADVANCED_FACE('',(#3516),#21340,.F.);
#22298=ADVANCED_FACE('',(#3517),#2579,.F.);
#22299=ADVANCED_FACE('',(#3518),#21341,.F.);
#22300=ADVANCED_FACE('',(#3519),#2580,.F.);
#22301=ADVANCED_FACE('',(#3520),#21342,.F.);
#22302=ADVANCED_FACE('',(#3521),#2581,.F.);
#22303=ADVANCED_FACE('',(#3522),#21343,.F.);
#22304=ADVANCED_FACE('',(#3523),#2582,.F.);
#22305=ADVANCED_FACE('',(#3524),#21344,.F.);
#22306=ADVANCED_FACE('',(#3525),#2583,.F.);
#22307=ADVANCED_FACE('',(#3526),#21345,.F.);
#22308=ADVANCED_FACE('',(#3527),#2584,.F.);
#22309=ADVANCED_FACE('',(#3528),#21346,.F.);
#22310=ADVANCED_FACE('',(#3529,#2085),#2585,.T.);
#22311=ADVANCED_FACE('',(#3530),#21347,.F.);
#22312=ADVANCED_FACE('',(#3531,#2086),#2586,.T.);
#22313=ADVANCED_FACE('',(#3532),#21348,.F.);
#22314=ADVANCED_FACE('',(#3533,#2087),#2587,.T.);
#22315=ADVANCED_FACE('',(#3534),#21349,.F.);
#22316=ADVANCED_FACE('',(#3535,#2088),#2588,.T.);
#22317=ADVANCED_FACE('',(#3536),#21350,.F.);
#22318=ADVANCED_FACE('',(#3537),#21351,.F.);
#22319=ADVANCED_FACE('',(#3538),#21352,.F.);
#22320=ADVANCED_FACE('',(#3539),#21353,.F.);
#22321=ADVANCED_FACE('',(#3540),#21354,.F.);
#22322=ADVANCED_FACE('',(#3541),#21355,.F.);
#22323=ADVANCED_FACE('',(#3542),#21356,.F.);
#22324=ADVANCED_FACE('',(#3543),#21357,.F.);
#22325=ADVANCED_FACE('',(#3544),#21358,.F.);
#22326=ADVANCED_FACE('',(#3545),#21359,.F.);
#22327=ADVANCED_FACE('',(#3546),#21360,.F.);
#22328=ADVANCED_FACE('',(#3547),#21361,.F.);
#22329=ADVANCED_FACE('',(#3548),#21362,.F.);
#22330=ADVANCED_FACE('',(#3549),#21363,.F.);
#22331=ADVANCED_FACE('',(#3550),#2589,.T.);
#22332=ADVANCED_FACE('',(#3551),#2590,.T.);
#22333=ADVANCED_FACE('',(#3552),#2591,.T.);
#22334=ADVANCED_FACE('',(#3553),#2592,.T.);
#22335=ADVANCED_FACE('',(#3554,#2089,#2090,#2091,#2092,#2093,#2094,#2095,
#2096,#2097,#2098,#2099,#2100,#2101,#2102),#2593,.T.);
#22336=ADVANCED_FACE('',(#3555,#2103,#2104,#2105,#2106,#2107,#2108,#2109,
#2110,#2111,#2112,#2113,#2114,#2115,#2116,#2117,#2118,#2119,#2120,#2121,
#2122,#2123,#2124),#2594,.F.);
#22337=ADVANCED_FACE('',(#3556),#21364,.F.);
#22338=ADVANCED_FACE('',(#3557),#21365,.F.);
#22339=ADVANCED_FACE('',(#3558),#21366,.F.);
#22340=ADVANCED_FACE('',(#3559),#21367,.F.);
#22341=ADVANCED_FACE('',(#3560),#21368,.F.);
#22342=ADVANCED_FACE('',(#3561),#21369,.F.);
#22343=ADVANCED_FACE('',(#3562),#21370,.F.);
#22344=ADVANCED_FACE('',(#3563,#2125),#2595,.T.);
#22345=ADVANCED_FACE('',(#3564),#21371,.F.);
#22346=ADVANCED_FACE('',(#3565,#2126),#2596,.T.);
#22347=ADVANCED_FACE('',(#3566),#21372,.F.);
#22348=ADVANCED_FACE('',(#3567,#2127),#2597,.T.);
#22349=ADVANCED_FACE('',(#3568),#21373,.F.);
#22350=ADVANCED_FACE('',(#3569,#2128),#2598,.T.);
#22351=ADVANCED_FACE('',(#3570,#2129,#2130,#2131,#2132,#2133,#2134),#2599,
 .T.);
#22352=ADVANCED_FACE('',(#3571),#21374,.F.);
#22353=ADVANCED_FACE('',(#3572),#21375,.F.);
#22354=ADVANCED_FACE('',(#3573),#21376,.F.);
#22355=ADVANCED_FACE('',(#3574),#21377,.F.);
#22356=ADVANCED_FACE('',(#3575),#2600,.T.);
#22357=ADVANCED_FACE('',(#3576),#2601,.T.);
#22358=ADVANCED_FACE('',(#3577),#2602,.T.);
#22359=ADVANCED_FACE('',(#3578),#2603,.T.);
#22360=ADVANCED_FACE('',(#3579,#2135,#2136,#2137,#2138,#2139,#2140,#2141,
#2142),#2604,.F.);
#22361=ADVANCED_FACE('',(#3580),#21378,.F.);
#22362=ADVANCED_FACE('',(#3581),#21379,.F.);
#22363=ADVANCED_FACE('',(#3582),#21380,.F.);
#22364=ADVANCED_FACE('',(#3583),#21381,.F.);
#22365=ADVANCED_FACE('',(#3584,#2143),#2605,.F.);
#22366=ADVANCED_FACE('',(#3585),#21382,.F.);
#22367=ADVANCED_FACE('',(#3586),#21383,.F.);
#22368=ADVANCED_FACE('',(#3587),#2606,.F.);
#22369=ADVANCED_FACE('',(#3588),#21384,.F.);
#22370=ADVANCED_FACE('',(#3589),#2607,.F.);
#22371=ADVANCED_FACE('',(#3590),#2608,.T.);
#22372=ADVANCED_FACE('',(#3591,#2144,#2145,#2146,#2147),#2609,.T.);
#22373=ADVANCED_FACE('',(#3592),#2610,.T.);
#22374=ADVANCED_FACE('',(#3593,#2148,#2149,#2150,#2151),#2611,.T.);
#22375=ADVANCED_FACE('',(#3594),#2612,.T.);
#22376=ADVANCED_FACE('',(#3595,#2152,#2153),#2613,.F.);
#22377=ADVANCED_FACE('',(#3596),#21385,.F.);
#22378=ADVANCED_FACE('',(#3597),#21386,.F.);
#22379=ADVANCED_FACE('',(#3598),#21387,.F.);
#22380=ADVANCED_FACE('',(#3599),#21388,.T.);
#22381=ADVANCED_FACE('',(#3600,#2154),#2614,.T.);
#22382=ADVANCED_FACE('',(#3601),#21389,.F.);
#22383=ADVANCED_FACE('',(#3602),#21390,.T.);
#22384=ADVANCED_FACE('',(#3603,#2155,#2156,#2157,#2158),#2615,.T.);
#22385=ADVANCED_FACE('',(#3604,#2159,#2160,#2161,#2162),#2616,.F.);
#22386=ADVANCED_FACE('',(#3605),#21391,.F.);
#22387=ADVANCED_FACE('',(#3606),#21392,.F.);
#22388=ADVANCED_FACE('',(#3607),#21393,.F.);
#22389=ADVANCED_FACE('',(#3608),#21394,.F.);
#22390=ADVANCED_FACE('',(#3609,#2163),#2617,.T.);
#22391=ADVANCED_FACE('',(#3610),#21395,.F.);
#22392=ADVANCED_FACE('',(#3611),#21396,.F.);
#22393=ADVANCED_FACE('',(#3612),#2618,.F.);
#22394=ADVANCED_FACE('',(#3613),#21397,.F.);
#22395=ADVANCED_FACE('',(#3614),#2619,.F.);
#22396=ADVANCED_FACE('',(#3615),#2620,.T.);
#22397=ADVANCED_FACE('',(#3616,#2164,#2165,#2166,#2167),#2621,.T.);
#22398=ADVANCED_FACE('',(#3617),#2622,.T.);
#22399=ADVANCED_FACE('',(#3618,#2168,#2169,#2170,#2171),#2623,.T.);
#22400=ADVANCED_FACE('',(#3619),#2624,.T.);
#22401=ADVANCED_FACE('',(#3620,#2172,#2173),#2625,.F.);
#22402=ADVANCED_FACE('',(#3621),#21398,.F.);
#22403=ADVANCED_FACE('',(#3622),#21399,.F.);
#22404=ADVANCED_FACE('',(#3623),#21400,.F.);
#22405=ADVANCED_FACE('',(#3624),#2626,.F.);
#22406=ADVANCED_FACE('',(#3625,#2174,#2175,#2176,#2177),#2627,.F.);
#22407=ADVANCED_FACE('',(#3626),#21401,.T.);
#22408=ADVANCED_FACE('',(#3627),#21402,.T.);
#22409=ADVANCED_FACE('',(#3628,#2178),#2628,.F.);
#22410=ADVANCED_FACE('',(#3629),#21403,.F.);
#22411=ADVANCED_FACE('',(#3630,#2179,#2180,#2181,#2182),#2629,.T.);
#22412=ADVANCED_FACE('',(#3631),#21404,.F.);
#22413=ADVANCED_FACE('',(#3632,#2183),#2630,.T.);
#22414=ADVANCED_FACE('',(#3633),#21405,.F.);
#22415=ADVANCED_FACE('',(#3634),#2631,.T.);
#22416=ADVANCED_FACE('',(#3635),#2632,.T.);
#22417=ADVANCED_FACE('',(#3636),#2633,.T.);
#22418=ADVANCED_FACE('',(#3637),#2634,.T.);
#22419=ADVANCED_FACE('',(#3638,#2184),#2635,.T.);
#22420=ADVANCED_FACE('',(#3639,#2185),#2636,.F.);
#22421=ADVANCED_FACE('',(#3640),#21406,.F.);
#22422=ADVANCED_FACE('',(#3641,#2186),#2637,.T.);
#22423=ADVANCED_FACE('',(#3642),#21407,.F.);
#22424=ADVANCED_FACE('',(#3643),#2638,.T.);
#22425=ADVANCED_FACE('',(#3644),#2639,.T.);
#22426=ADVANCED_FACE('',(#3645),#2640,.T.);
#22427=ADVANCED_FACE('',(#3646),#2641,.T.);
#22428=ADVANCED_FACE('',(#3647,#2187),#2642,.T.);
#22429=ADVANCED_FACE('',(#3648,#2188),#2643,.F.);
#22430=ADVANCED_FACE('',(#3649),#21408,.F.);
#22431=ADVANCED_FACE('',(#3650,#2189),#2644,.T.);
#22432=ADVANCED_FACE('',(#3651),#21409,.F.);
#22433=ADVANCED_FACE('',(#3652,#2190),#2645,.T.);
#22434=ADVANCED_FACE('',(#3653),#21410,.F.);
#22435=ADVANCED_FACE('',(#3654,#2191),#2646,.T.);
#22436=ADVANCED_FACE('',(#3655),#21411,.F.);
#22437=ADVANCED_FACE('',(#3656,#2192),#2647,.T.);
#22438=ADVANCED_FACE('',(#3657),#21412,.F.);
#22439=ADVANCED_FACE('',(#3658),#21413,.F.);
#22440=ADVANCED_FACE('',(#3659),#21414,.F.);
#22441=ADVANCED_FACE('',(#3660),#21415,.F.);
#22442=ADVANCED_FACE('',(#3661),#2648,.T.);
#22443=ADVANCED_FACE('',(#3662),#2649,.T.);
#22444=ADVANCED_FACE('',(#3663),#2650,.T.);
#22445=ADVANCED_FACE('',(#3664),#2651,.T.);
#22446=ADVANCED_FACE('',(#3665,#2193,#2194,#2195,#2196),#2652,.T.);
#22447=ADVANCED_FACE('',(#3666),#2653,.T.);
#22448=ADVANCED_FACE('',(#3667),#2654,.T.);
#22449=ADVANCED_FACE('',(#3668),#2655,.T.);
#22450=ADVANCED_FACE('',(#3669),#2656,.T.);
#22451=ADVANCED_FACE('',(#3670),#2657,.T.);
#22452=ADVANCED_FACE('',(#3671,#2197,#2198,#2199,#2200),#2658,.T.);
#22453=ADVANCED_FACE('',(#3672),#2659,.T.);
#22454=ADVANCED_FACE('',(#3673),#2660,.T.);
#22455=ADVANCED_FACE('',(#3674),#2661,.F.);
#22456=ADVANCED_FACE('',(#3675),#1500,.F.);
#22457=ADVANCED_FACE('',(#3676),#21416,.T.);
#22458=ADVANCED_FACE('',(#3677),#21417,.F.);
#22459=ADVANCED_FACE('',(#3678),#1467,.F.);
#22460=ADVANCED_FACE('',(#3679,#2201),#2662,.T.);
#22461=ADVANCED_FACE('',(#3680),#21418,.T.);
#22462=ADVANCED_FACE('',(#3681,#2202),#2663,.T.);
#22463=ADVANCED_FACE('',(#3682),#1468,.F.);
#22464=ADVANCED_FACE('',(#3683),#1501,.F.);
#22465=ADVANCED_FACE('',(#3684),#21419,.F.);
#22466=ADVANCED_FACE('',(#3685,#2203),#2664,.T.);
#22467=ADVANCED_FACE('',(#3686),#1469,.T.);
#22468=ADVANCED_FACE('',(#3687),#21420,.T.);
#22469=ADVANCED_FACE('',(#3688),#1470,.T.);
#22470=ADVANCED_FACE('',(#3689,#2204),#2665,.T.);
#22471=ADVANCED_FACE('',(#3690),#21421,.F.);
#22472=ADVANCED_FACE('',(#3691),#1411,.T.);
#22473=ADVANCED_FACE('',(#3692),#1412,.T.);
#22474=ADVANCED_FACE('',(#3693),#1413,.T.);
#22475=ADVANCED_FACE('',(#3694),#1414,.T.);
#22476=ADVANCED_FACE('',(#3695),#1415,.T.);
#22477=ADVANCED_FACE('',(#3696),#1416,.T.);
#22478=ADVANCED_FACE('',(#3697),#1417,.T.);
#22479=ADVANCED_FACE('',(#3698),#1418,.F.);
#22480=ADVANCED_FACE('',(#3699),#21422,.T.);
#22481=ADVANCED_FACE('',(#3700),#2666,.T.);
#22482=ADVANCED_FACE('',(#3701),#1419,.F.);
#22483=ADVANCED_FACE('',(#3702),#2667,.T.);
#22484=ADVANCED_FACE('',(#3703),#1420,.F.);
#22485=ADVANCED_FACE('',(#3704),#2668,.T.);
#22486=ADVANCED_FACE('',(#3705),#1421,.F.);
#22487=ADVANCED_FACE('',(#3706),#2669,.T.);
#22488=ADVANCED_FACE('',(#3707),#1422,.F.);
#22489=ADVANCED_FACE('',(#3708),#2670,.T.);
#22490=ADVANCED_FACE('',(#3709),#1423,.F.);
#22491=ADVANCED_FACE('',(#3710),#21423,.F.);
#22492=ADVANCED_FACE('',(#3711),#2671,.T.);
#22493=ADVANCED_FACE('',(#3712),#1424,.F.);
#22494=ADVANCED_FACE('',(#3713,#2205),#2672,.T.);
#22495=ADVANCED_FACE('',(#3714),#2673,.T.);
#22496=ADVANCED_FACE('',(#3715,#2206),#2674,.T.);
#22497=ADVANCED_FACE('',(#3716),#21424,.T.);
#22498=ADVANCED_FACE('',(#3717,#2207),#2675,.T.);
#22499=ADVANCED_FACE('',(#3718),#21425,.F.);
#22500=ADVANCED_FACE('',(#3719,#2208),#2676,.T.);
#22501=ADVANCED_FACE('',(#3720),#21426,.T.);
#22502=ADVANCED_FACE('',(#3721,#2209),#2677,.T.);
#22503=ADVANCED_FACE('',(#3722),#21427,.F.);
#22504=ADVANCED_FACE('',(#3723),#1502,.F.);
#22505=ADVANCED_FACE('',(#3724),#21428,.T.);
#22506=ADVANCED_FACE('',(#3725),#21429,.F.);
#22507=ADVANCED_FACE('',(#3726),#1471,.F.);
#22508=ADVANCED_FACE('',(#3727,#2210),#2678,.T.);
#22509=ADVANCED_FACE('',(#3728),#21430,.T.);
#22510=ADVANCED_FACE('',(#3729,#2211),#2679,.T.);
#22511=ADVANCED_FACE('',(#3730),#1472,.F.);
#22512=ADVANCED_FACE('',(#3731),#1503,.F.);
#22513=ADVANCED_FACE('',(#3732),#21431,.F.);
#22514=ADVANCED_FACE('',(#3733,#2212),#2680,.T.);
#22515=ADVANCED_FACE('',(#3734),#1473,.T.);
#22516=ADVANCED_FACE('',(#3735),#21432,.T.);
#22517=ADVANCED_FACE('',(#3736),#1474,.T.);
#22518=ADVANCED_FACE('',(#3737,#2213),#2681,.T.);
#22519=ADVANCED_FACE('',(#3738),#21433,.F.);
#22520=ADVANCED_FACE('',(#3739),#1425,.T.);
#22521=ADVANCED_FACE('',(#3740),#1426,.T.);
#22522=ADVANCED_FACE('',(#3741),#1427,.T.);
#22523=ADVANCED_FACE('',(#3742),#1428,.T.);
#22524=ADVANCED_FACE('',(#3743),#1429,.T.);
#22525=ADVANCED_FACE('',(#3744),#1430,.T.);
#22526=ADVANCED_FACE('',(#3745),#1431,.T.);
#22527=ADVANCED_FACE('',(#3746),#1432,.T.);
#22528=ADVANCED_FACE('',(#3747),#1433,.F.);
#22529=ADVANCED_FACE('',(#3748),#21434,.T.);
#22530=ADVANCED_FACE('',(#3749),#2682,.T.);
#22531=ADVANCED_FACE('',(#3750),#1434,.F.);
#22532=ADVANCED_FACE('',(#3751),#2683,.T.);
#22533=ADVANCED_FACE('',(#3752),#1435,.F.);
#22534=ADVANCED_FACE('',(#3753),#2684,.T.);
#22535=ADVANCED_FACE('',(#3754),#1436,.F.);
#22536=ADVANCED_FACE('',(#3755),#2685,.T.);
#22537=ADVANCED_FACE('',(#3756),#1437,.F.);
#22538=ADVANCED_FACE('',(#3757),#2686,.T.);
#22539=ADVANCED_FACE('',(#3758),#1438,.F.);
#22540=ADVANCED_FACE('',(#3759),#2687,.T.);
#22541=ADVANCED_FACE('',(#3760),#1439,.F.);
#22542=ADVANCED_FACE('',(#3761),#21435,.F.);
#22543=ADVANCED_FACE('',(#3762),#2688,.T.);
#22544=ADVANCED_FACE('',(#3763),#1440,.F.);
#22545=ADVANCED_FACE('',(#3764,#2214),#2689,.T.);
#22546=ADVANCED_FACE('',(#3765),#2690,.T.);
#22547=ADVANCED_FACE('',(#3766,#2215),#2691,.T.);
#22548=ADVANCED_FACE('',(#3767),#21436,.T.);
#22549=ADVANCED_FACE('',(#3768,#2216),#2692,.T.);
#22550=ADVANCED_FACE('',(#3769),#21437,.F.);
#22551=ADVANCED_FACE('',(#3770,#2217),#2693,.T.);
#22552=ADVANCED_FACE('',(#3771),#21438,.T.);
#22553=ADVANCED_FACE('',(#3772,#2218),#2694,.T.);
#22554=ADVANCED_FACE('',(#3773),#21439,.F.);
#22555=ADVANCED_FACE('',(#3774),#2695,.F.);
#22556=ADVANCED_FACE('',(#3775),#2696,.F.);
#22557=ADVANCED_FACE('',(#3776),#2697,.F.);
#22558=ADVANCED_FACE('',(#3777),#2698,.F.);
#22559=ADVANCED_FACE('',(#3778),#2699,.F.);
#22560=ADVANCED_FACE('',(#3779),#2700,.F.);
#22561=ADVANCED_FACE('',(#3780),#2701,.F.);
#22562=ADVANCED_FACE('',(#3781),#2702,.F.);
#22563=ADVANCED_FACE('',(#3782),#2703,.F.);
#22564=ADVANCED_FACE('',(#3783),#2704,.T.);
#22565=ADVANCED_FACE('',(#3784),#1475,.T.);
#22566=ADVANCED_FACE('',(#3785),#21440,.T.);
#22567=ADVANCED_FACE('',(#3786),#1476,.T.);
#22568=ADVANCED_FACE('',(#3787,#2219),#2705,.T.);
#22569=ADVANCED_FACE('',(#3788),#1477,.T.);
#22570=ADVANCED_FACE('',(#3789),#21441,.T.);
#22571=ADVANCED_FACE('',(#3790),#21442,.F.);
#22572=ADVANCED_FACE('',(#3791),#21443,.F.);
#22573=ADVANCED_FACE('',(#3792),#21444,.F.);
#22574=ADVANCED_FACE('',(#3793),#21445,.F.);
#22575=ADVANCED_FACE('',(#3794),#2706,.T.);
#22576=ADVANCED_FACE('',(#3795),#2707,.T.);
#22577=ADVANCED_FACE('',(#3796),#2708,.T.);
#22578=ADVANCED_FACE('',(#3797),#2709,.T.);
#22579=ADVANCED_FACE('',(#3798,#2220,#2221,#2222,#2223),#2710,.T.);
#22580=ADVANCED_FACE('',(#3799,#2224,#2225,#2226,#2227),#2711,.F.);
#22581=ADVANCED_FACE('',(#3800),#21446,.F.);
#22582=ADVANCED_FACE('',(#3801),#21447,.F.);
#22583=ADVANCED_FACE('',(#3802),#21448,.F.);
#22584=ADVANCED_FACE('',(#3803),#21449,.F.);
#22585=ADVANCED_FACE('',(#3804),#21450,.F.);
#22586=ADVANCED_FACE('',(#3805),#21451,.F.);
#22587=ADVANCED_FACE('',(#3806),#21452,.F.);
#22588=ADVANCED_FACE('',(#3807),#21453,.F.);
#22589=ADVANCED_FACE('',(#3808),#2712,.T.);
#22590=ADVANCED_FACE('',(#3809),#2713,.T.);
#22591=ADVANCED_FACE('',(#3810),#2714,.T.);
#22592=ADVANCED_FACE('',(#3811),#2715,.T.);
#22593=ADVANCED_FACE('',(#3812,#2228,#2229,#2230,#2231,#2232,#2233,#2234,
#2235),#2716,.T.);
#22594=ADVANCED_FACE('',(#3813,#2236,#2237,#2238,#2239,#2240,#2241,#2242,
#2243),#2717,.F.);
#22595=ADVANCED_FACE('',(#3814),#21454,.F.);
#22596=ADVANCED_FACE('',(#3815),#2718,.T.);
#22597=ADVANCED_FACE('',(#3816),#21455,.F.);
#22598=ADVANCED_FACE('',(#3817),#2719,.T.);
#22599=ADVANCED_FACE('',(#3818),#21456,.F.);
#22600=ADVANCED_FACE('',(#3819),#2720,.T.);
#22601=ADVANCED_FACE('',(#3820),#21457,.F.);
#22602=ADVANCED_FACE('',(#3821),#2721,.T.);
#22603=ADVANCED_FACE('',(#3822),#21458,.F.);
#22604=ADVANCED_FACE('',(#3823),#2722,.T.);
#22605=ADVANCED_FACE('',(#3824),#21459,.F.);
#22606=ADVANCED_FACE('',(#3825),#2723,.T.);
#22607=ADVANCED_FACE('',(#3826),#21460,.F.);
#22608=ADVANCED_FACE('',(#3827),#2724,.T.);
#22609=ADVANCED_FACE('',(#3828),#21461,.F.);
#22610=ADVANCED_FACE('',(#3829),#2725,.T.);
#22611=ADVANCED_FACE('',(#3830,#2244,#2245,#2246,#2247),#2726,.T.);
#22612=ADVANCED_FACE('',(#3831),#2727,.T.);
#22613=ADVANCED_FACE('',(#3832,#2248),#2728,.T.);
#22614=ADVANCED_FACE('',(#3833,#2249,#2250,#2251,#2252),#2729,.T.);
#22615=ADVANCED_FACE('',(#3834),#2730,.F.);
#22616=ADVANCED_FACE('',(#3835),#2731,.T.);
#22617=ADVANCED_FACE('',(#3836),#21462,.F.);
#22618=ADVANCED_FACE('',(#3837),#2732,.T.);
#22619=ADVANCED_FACE('',(#3838),#21463,.F.);
#22620=ADVANCED_FACE('',(#3839),#2733,.T.);
#22621=ADVANCED_FACE('',(#3840),#21464,.F.);
#22622=ADVANCED_FACE('',(#3841),#2734,.T.);
#22623=ADVANCED_FACE('',(#3842),#21465,.F.);
#22624=ADVANCED_FACE('',(#3843),#2735,.T.);
#22625=ADVANCED_FACE('',(#3844),#2736,.T.);
#22626=ADVANCED_FACE('',(#3845),#2737,.T.);
#22627=ADVANCED_FACE('',(#3846),#2738,.T.);
#22628=ADVANCED_FACE('',(#3847),#2739,.T.);
#22629=ADVANCED_FACE('',(#3848,#2253,#2254,#2255,#2256),#2740,.T.);
#22630=ADVANCED_FACE('',(#3849),#2741,.T.);
#22631=ADVANCED_FACE('',(#3850),#2742,.T.);
#22632=ADVANCED_FACE('',(#3851),#2743,.T.);
#22633=ADVANCED_FACE('',(#3852),#2744,.T.);
#22634=ADVANCED_FACE('',(#3853),#2745,.T.);
#22635=ADVANCED_FACE('',(#3854),#2746,.T.);
#22636=ADVANCED_FACE('',(#3855),#2747,.T.);
#22637=ADVANCED_FACE('',(#3856),#2748,.T.);
#22638=ADVANCED_FACE('',(#3857),#2749,.T.);
#22639=ADVANCED_FACE('',(#3858),#2750,.T.);
#22640=ADVANCED_FACE('',(#3859),#2751,.T.);
#22641=ADVANCED_FACE('',(#3860),#2752,.T.);
#22642=ADVANCED_FACE('',(#3861),#2753,.T.);
#22643=ADVANCED_FACE('',(#3862),#2754,.T.);
#22644=ADVANCED_FACE('',(#3863),#2755,.T.);
#22645=ADVANCED_FACE('',(#3864),#2756,.T.);
#22646=ADVANCED_FACE('',(#3865),#2757,.T.);
#22647=ADVANCED_FACE('',(#3866),#2758,.F.);
#22648=ADVANCED_FACE('',(#3867),#2759,.T.);
#22649=ADVANCED_FACE('',(#3868),#2760,.T.);
#22650=ADVANCED_FACE('',(#3869),#2761,.T.);
#22651=ADVANCED_FACE('',(#3870),#2762,.T.);
#22652=ADVANCED_FACE('',(#3871),#2763,.T.);
#22653=ADVANCED_FACE('',(#3872),#2764,.T.);
#22654=ADVANCED_FACE('',(#3873),#2765,.T.);
#22655=ADVANCED_FACE('',(#3874),#2766,.T.);
#22656=ADVANCED_FACE('',(#3875),#2767,.T.);
#22657=ADVANCED_FACE('',(#3876),#2768,.T.);
#22658=ADVANCED_FACE('',(#3877),#1478,.F.);
#22659=ADVANCED_FACE('',(#3878),#21466,.F.);
#22660=ADVANCED_FACE('',(#3879,#2257),#2769,.T.);
#22661=ADVANCED_FACE('',(#3880),#21467,.T.);
#22662=ADVANCED_FACE('',(#3881,#2258),#2770,.F.);
#22663=ADVANCED_FACE('',(#3882),#2771,.F.);
#22664=ADVANCED_FACE('',(#3883),#2772,.F.);
#22665=ADVANCED_FACE('',(#3884),#2773,.F.);
#22666=ADVANCED_FACE('',(#3885),#2774,.F.);
#22667=ADVANCED_FACE('',(#3886),#2775,.F.);
#22668=ADVANCED_FACE('',(#3887),#2776,.F.);
#22669=ADVANCED_FACE('',(#3888),#2777,.F.);
#22670=ADVANCED_FACE('',(#3889),#2778,.F.);
#22671=ADVANCED_FACE('',(#3890,#2259),#2779,.T.);
#22672=ADVANCED_FACE('',(#3891),#21468,.T.);
#22673=ADVANCED_FACE('',(#3892),#2780,.F.);
#22674=ADVANCED_FACE('',(#3893),#2781,.T.);
#22675=ADVANCED_FACE('',(#3894),#1479,.T.);
#22676=ADVANCED_FACE('',(#3895),#21469,.T.);
#22677=ADVANCED_FACE('',(#3896),#1480,.T.);
#22678=ADVANCED_FACE('',(#3897,#2260),#2782,.T.);
#22679=ADVANCED_FACE('',(#3898),#1481,.T.);
#22680=ADVANCED_FACE('',(#3899),#21470,.T.);
#22681=ADVANCED_FACE('',(#3900),#21471,.F.);
#22682=ADVANCED_FACE('',(#3901),#21472,.F.);
#22683=ADVANCED_FACE('',(#3902),#21473,.F.);
#22684=ADVANCED_FACE('',(#3903),#21474,.F.);
#22685=ADVANCED_FACE('',(#3904),#21475,.F.);
#22686=ADVANCED_FACE('',(#3905),#21476,.F.);
#22687=ADVANCED_FACE('',(#3906),#21477,.F.);
#22688=ADVANCED_FACE('',(#3907),#21478,.F.);
#22689=ADVANCED_FACE('',(#3908),#21479,.F.);
#22690=ADVANCED_FACE('',(#3909),#21480,.F.);
#22691=ADVANCED_FACE('',(#3910),#21481,.F.);
#22692=ADVANCED_FACE('',(#3911),#21482,.F.);
#22693=ADVANCED_FACE('',(#3912),#21483,.F.);
#22694=ADVANCED_FACE('',(#3913),#21484,.F.);
#22695=ADVANCED_FACE('',(#3914),#21485,.F.);
#22696=ADVANCED_FACE('',(#3915),#21486,.F.);
#22697=ADVANCED_FACE('',(#3916),#21487,.F.);
#22698=ADVANCED_FACE('',(#3917),#21488,.F.);
#22699=ADVANCED_FACE('',(#3918),#21489,.F.);
#22700=ADVANCED_FACE('',(#3919),#15,.F.);
#22701=ADVANCED_FACE('',(#3920),#16,.F.);
#22702=ADVANCED_FACE('',(#3921,#2261,#2262,#2263,#2264),#2783,.T.);
#22703=ADVANCED_FACE('',(#3922),#21490,.F.);
#22704=ADVANCED_FACE('',(#3923),#21491,.F.);
#22705=ADVANCED_FACE('',(#3924),#21492,.F.);
#22706=ADVANCED_FACE('',(#3925),#2784,.F.);
#22707=ADVANCED_FACE('',(#3926,#2265,#2266,#2267,#2268),#2785,.F.);
#22708=ADVANCED_FACE('',(#3927),#21493,.T.);
#22709=ADVANCED_FACE('',(#3928),#21494,.F.);
#22710=ADVANCED_FACE('',(#3929),#21495,.T.);
#22711=ADVANCED_FACE('',(#3930,#2269),#2786,.F.);
#22712=ADVANCED_FACE('',(#3931),#2787,.T.);
#22713=ADVANCED_FACE('',(#3932),#1482,.T.);
#22714=ADVANCED_FACE('',(#3933),#21496,.T.);
#22715=ADVANCED_FACE('',(#3934),#1483,.T.);
#22716=ADVANCED_FACE('',(#3935,#2270),#2788,.T.);
#22717=ADVANCED_FACE('',(#3936),#1484,.T.);
#22718=ADVANCED_FACE('',(#3937),#21497,.T.);
#22719=ADVANCED_FACE('',(#3938),#1485,.T.);
#22720=ADVANCED_FACE('',(#3939),#2789,.T.);
#22721=ADVANCED_FACE('',(#3940),#2790,.F.);
#22722=ADVANCED_FACE('',(#3941),#2791,.F.);
#22723=ADVANCED_FACE('',(#3942),#2792,.F.);
#22724=ADVANCED_FACE('',(#3943),#2793,.F.);
#22725=ADVANCED_FACE('',(#3944),#2794,.F.);
#22726=ADVANCED_FACE('',(#3945),#2795,.F.);
#22727=ADVANCED_FACE('',(#3946),#2796,.F.);
#22728=ADVANCED_FACE('',(#3947),#2797,.F.);
#22729=ADVANCED_FACE('',(#3948),#2798,.T.);
#22730=ADVANCED_FACE('',(#3949),#1486,.T.);
#22731=ADVANCED_FACE('',(#3950),#21498,.T.);
#22732=ADVANCED_FACE('',(#3951),#1487,.T.);
#22733=ADVANCED_FACE('',(#3952,#2271),#2799,.T.);
#22734=ADVANCED_FACE('',(#3953),#1488,.T.);
#22735=ADVANCED_FACE('',(#3954),#21499,.T.);
#22736=ADVANCED_FACE('',(#3955),#1489,.T.);
#22737=ADVANCED_FACE('',(#3956),#2800,.T.);
#22738=ADVANCED_FACE('',(#3957),#2801,.F.);
#22739=ADVANCED_FACE('',(#3958),#2802,.F.);
#22740=ADVANCED_FACE('',(#3959),#2803,.F.);
#22741=ADVANCED_FACE('',(#3960),#2804,.F.);
#22742=ADVANCED_FACE('',(#3961),#2805,.F.);
#22743=ADVANCED_FACE('',(#3962),#2806,.F.);
#22744=ADVANCED_FACE('',(#3963),#2807,.F.);
#22745=ADVANCED_FACE('',(#3964),#2808,.F.);
#22746=ADVANCED_FACE('',(#3965),#21500,.T.);
#22747=ADVANCED_FACE('',(#3966),#21501,.T.);
#22748=ADVANCED_FACE('',(#3967),#21502,.T.);
#22749=ADVANCED_FACE('',(#3968),#21503,.T.);
#22750=ADVANCED_FACE('',(#3969),#21504,.T.);
#22751=ADVANCED_FACE('',(#3970),#21505,.T.);
#22752=ADVANCED_FACE('',(#3971),#21506,.T.);
#22753=ADVANCED_FACE('',(#3972),#21507,.T.);
#22754=ADVANCED_FACE('',(#3973),#21508,.T.);
#22755=ADVANCED_FACE('',(#3974),#21509,.T.);
#22756=ADVANCED_FACE('',(#3975),#21510,.T.);
#22757=ADVANCED_FACE('',(#3976),#21511,.T.);
#22758=ADVANCED_FACE('',(#3977),#21512,.T.);
#22759=ADVANCED_FACE('',(#3978),#21513,.T.);
#22760=ADVANCED_FACE('',(#3979),#21514,.T.);
#22761=ADVANCED_FACE('',(#3980),#21515,.T.);
#22762=ADVANCED_FACE('',(#3981),#21516,.T.);
#22763=ADVANCED_FACE('',(#3982),#21517,.T.);
#22764=ADVANCED_FACE('',(#3983),#21518,.T.);
#22765=ADVANCED_FACE('',(#3984),#21519,.T.);
#22766=ADVANCED_FACE('',(#3985),#21520,.T.);
#22767=ADVANCED_FACE('',(#3986),#21521,.T.);
#22768=ADVANCED_FACE('',(#3987),#21522,.T.);
#22769=ADVANCED_FACE('',(#3988),#21523,.T.);
#22770=ADVANCED_FACE('',(#3989),#21524,.T.);
#22771=ADVANCED_FACE('',(#3990),#21525,.T.);
#22772=ADVANCED_FACE('',(#3991),#21526,.T.);
#22773=ADVANCED_FACE('',(#3992),#21527,.T.);
#22774=ADVANCED_FACE('',(#3993),#21528,.T.);
#22775=ADVANCED_FACE('',(#3994),#21529,.T.);
#22776=ADVANCED_FACE('',(#3995),#21530,.T.);
#22777=ADVANCED_FACE('',(#3996),#21531,.T.);
#22778=ADVANCED_FACE('',(#3997),#21532,.T.);
#22779=ADVANCED_FACE('',(#3998),#21533,.T.);
#22780=ADVANCED_FACE('',(#3999),#21534,.T.);
#22781=ADVANCED_FACE('',(#4000),#21535,.T.);
#22782=ADVANCED_FACE('',(#4001),#21536,.T.);
#22783=ADVANCED_FACE('',(#4002),#21537,.T.);
#22784=ADVANCED_FACE('',(#4003),#21538,.T.);
#22785=ADVANCED_FACE('',(#4004),#21539,.T.);
#22786=ADVANCED_FACE('',(#4005),#21540,.T.);
#22787=ADVANCED_FACE('',(#4006),#21541,.T.);
#22788=ADVANCED_FACE('',(#4007),#21542,.T.);
#22789=ADVANCED_FACE('',(#4008),#21543,.T.);
#22790=ADVANCED_FACE('',(#4009),#21544,.T.);
#22791=ADVANCED_FACE('',(#4010),#21545,.T.);
#22792=ADVANCED_FACE('',(#4011),#21546,.T.);
#22793=ADVANCED_FACE('',(#4012),#21547,.T.);
#22794=ADVANCED_FACE('',(#4013),#21548,.T.);
#22795=ADVANCED_FACE('',(#4014),#21549,.T.);
#22796=ADVANCED_FACE('',(#4015),#21550,.T.);
#22797=ADVANCED_FACE('',(#4016),#21551,.T.);
#22798=ADVANCED_FACE('',(#4017),#21552,.T.);
#22799=ADVANCED_FACE('',(#4018),#21553,.T.);
#22800=ADVANCED_FACE('',(#4019),#21554,.T.);
#22801=ADVANCED_FACE('',(#4020),#21555,.T.);
#22802=ADVANCED_FACE('',(#4021),#21556,.T.);
#22803=ADVANCED_FACE('',(#4022),#21557,.T.);
#22804=ADVANCED_FACE('',(#4023),#21558,.T.);
#22805=ADVANCED_FACE('',(#4024),#21559,.T.);
#22806=ADVANCED_FACE('',(#4025),#21560,.T.);
#22807=ADVANCED_FACE('',(#4026),#21561,.T.);
#22808=ADVANCED_FACE('',(#4027),#21562,.T.);
#22809=ADVANCED_FACE('',(#4028),#21563,.T.);
#22810=ADVANCED_FACE('',(#4029),#21564,.T.);
#22811=ADVANCED_FACE('',(#4030),#21565,.T.);
#22812=ADVANCED_FACE('',(#4031),#21566,.T.);
#22813=ADVANCED_FACE('',(#4032),#21567,.T.);
#22814=ADVANCED_FACE('',(#4033),#21568,.T.);
#22815=ADVANCED_FACE('',(#4034),#21569,.T.);
#22816=ADVANCED_FACE('',(#4035),#21570,.T.);
#22817=ADVANCED_FACE('',(#4036),#21571,.T.);
#22818=ADVANCED_FACE('',(#4037),#21572,.T.);
#22819=ADVANCED_FACE('',(#4038),#21573,.T.);
#22820=ADVANCED_FACE('',(#4039),#21574,.T.);
#22821=ADVANCED_FACE('',(#4040),#21575,.T.);
#22822=ADVANCED_FACE('',(#4041),#21576,.T.);
#22823=ADVANCED_FACE('',(#4042),#21577,.T.);
#22824=ADVANCED_FACE('',(#4043),#21578,.T.);
#22825=ADVANCED_FACE('',(#4044),#21579,.T.);
#22826=ADVANCED_FACE('',(#4045),#21580,.T.);
#22827=ADVANCED_FACE('',(#4046),#21581,.T.);
#22828=ADVANCED_FACE('',(#4047),#21582,.T.);
#22829=ADVANCED_FACE('',(#4048),#21583,.T.);
#22830=ADVANCED_FACE('',(#4049),#21584,.T.);
#22831=ADVANCED_FACE('',(#4050),#21585,.T.);
#22832=ADVANCED_FACE('',(#4051),#21586,.T.);
#22833=ADVANCED_FACE('',(#4052),#21587,.T.);
#22834=ADVANCED_FACE('',(#4053),#21588,.T.);
#22835=ADVANCED_FACE('',(#4054),#21589,.T.);
#22836=ADVANCED_FACE('',(#4055),#21590,.T.);
#22837=ADVANCED_FACE('',(#4056),#21591,.T.);
#22838=ADVANCED_FACE('',(#4057),#21592,.T.);
#22839=ADVANCED_FACE('',(#4058),#21593,.T.);
#22840=ADVANCED_FACE('',(#4059),#21594,.T.);
#22841=ADVANCED_FACE('',(#4060),#21595,.T.);
#22842=ADVANCED_FACE('',(#4061),#21596,.T.);
#22843=ADVANCED_FACE('',(#4062),#21597,.T.);
#22844=ADVANCED_FACE('',(#4063),#21598,.T.);
#22845=ADVANCED_FACE('',(#4064),#21599,.T.);
#22846=ADVANCED_FACE('',(#4065),#21600,.T.);
#22847=ADVANCED_FACE('',(#4066),#21601,.T.);
#22848=ADVANCED_FACE('',(#4067),#21602,.T.);
#22849=ADVANCED_FACE('',(#4068),#21603,.T.);
#22850=ADVANCED_FACE('',(#4069),#21604,.T.);
#22851=ADVANCED_FACE('',(#4070),#21605,.T.);
#22852=ADVANCED_FACE('',(#4071),#21606,.T.);
#22853=ADVANCED_FACE('',(#4072),#21607,.T.);
#22854=ADVANCED_FACE('',(#4073),#21608,.T.);
#22855=ADVANCED_FACE('',(#4074),#21609,.T.);
#22856=ADVANCED_FACE('',(#4075),#21610,.T.);
#22857=ADVANCED_FACE('',(#4076),#21611,.T.);
#22858=ADVANCED_FACE('',(#4077),#21612,.T.);
#22859=ADVANCED_FACE('',(#4078),#21613,.T.);
#22860=ADVANCED_FACE('',(#4079),#21614,.T.);
#22861=ADVANCED_FACE('',(#4080),#21615,.T.);
#22862=ADVANCED_FACE('',(#4081),#21616,.T.);
#22863=ADVANCED_FACE('',(#4082),#21617,.T.);
#22864=ADVANCED_FACE('',(#4083),#21618,.T.);
#22865=ADVANCED_FACE('',(#4084),#21619,.T.);
#22866=ADVANCED_FACE('',(#4085),#21620,.T.);
#22867=ADVANCED_FACE('',(#4086),#21621,.T.);
#22868=ADVANCED_FACE('',(#4087),#21622,.T.);
#22869=ADVANCED_FACE('',(#4088),#21623,.T.);
#22870=ADVANCED_FACE('',(#4089),#21624,.T.);
#22871=ADVANCED_FACE('',(#4090),#21625,.T.);
#22872=ADVANCED_FACE('',(#4091,#2272),#2809,.T.);
#22873=ADVANCED_FACE('',(#4092),#21626,.T.);
#22874=ADVANCED_FACE('',(#4093),#2810,.F.);
#22875=ADVANCED_FACE('',(#4094),#17,.F.);
#22876=ADVANCED_FACE('',(#4095),#21627,.T.);
#22877=ADVANCED_FACE('',(#4096),#18,.F.);
#22878=ADVANCED_FACE('',(#4097),#2811,.F.);
#22879=ADVANCED_FACE('',(#4098),#2812,.T.);
#22880=ADVANCED_FACE('',(#4099),#2813,.F.);
#22881=ADVANCED_FACE('',(#4100),#2814,.F.);
#22882=ADVANCED_FACE('',(#4101),#2815,.F.);
#22883=ADVANCED_FACE('',(#4102,#2273),#21628,.T.);
#22884=ADVANCED_FACE('',(#4103),#2816,.T.);
#22885=ADVANCED_FACE('',(#4104,#2274),#2817,.F.);
#22886=ADVANCED_FACE('',(#4105),#21629,.T.);
#22887=ADVANCED_FACE('',(#4106,#2275),#2818,.T.);
#22888=ADVANCED_FACE('',(#4107),#21630,.T.);
#22889=ADVANCED_FACE('',(#4108),#21631,.F.);
#22890=ADVANCED_FACE('',(#4109),#21632,.T.);
#22891=ADVANCED_FACE('',(#4110,#2276),#2819,.T.);
#22892=ADVANCED_FACE('',(#4111,#2277),#2820,.F.);
#22893=ADVANCED_FACE('',(#4112),#2821,.T.);
#22894=ADVANCED_FACE('',(#4113),#21633,.F.);
#22895=ADVANCED_FACE('',(#4114),#2822,.T.);
#22896=ADVANCED_FACE('',(#4115,#2278),#21634,.F.);
#22897=ADVANCED_FACE('',(#4116,#2279),#21635,.T.);
#22898=ADVANCED_FACE('',(#4117,#2280),#2823,.T.);
#22899=ADVANCED_FACE('',(#4118,#2281),#2824,.F.);
#22900=ADVANCED_FACE('',(#4119),#21636,.F.);
#22901=ADVANCED_FACE('',(#4120),#2825,.T.);
#22902=ADVANCED_FACE('',(#4121),#21637,.F.);
#22903=ADVANCED_FACE('',(#4122),#2826,.T.);
#22904=ADVANCED_FACE('',(#4123),#2827,.F.);
#22905=ADVANCED_FACE('',(#4124),#2828,.F.);
#22906=ADVANCED_FACE('',(#4125),#2829,.F.);
#22907=ADVANCED_FACE('',(#4126,#2282,#2283),#2830,.T.);
#22908=ADVANCED_FACE('',(#4127,#2284,#2285),#2831,.F.);
#22909=ADVANCED_FACE('',(#4128),#21638,.T.);
#22910=ADVANCED_FACE('',(#4129,#2286),#21639,.F.);
#22911=ADVANCED_FACE('',(#4130,#2287),#21640,.T.);
#22912=ADVANCED_FACE('',(#4131),#2832,.F.);
#22913=ADVANCED_FACE('',(#4132),#21641,.F.);
#22914=ADVANCED_FACE('',(#4133),#21642,.T.);
#22915=ADVANCED_FACE('',(#4134,#2288),#2833,.T.);
#22916=ADVANCED_FACE('',(#4135,#2289),#2834,.F.);
#22917=ADVANCED_FACE('',(#4136),#21643,.F.);
#22918=ADVANCED_FACE('',(#4137),#21644,.T.);
#22919=ADVANCED_FACE('',(#4138,#2290),#2835,.T.);
#22920=ADVANCED_FACE('',(#4139,#2291),#2836,.F.);
#22921=ADVANCED_FACE('',(#4140),#2837,.F.);
#22922=ADVANCED_FACE('',(#4141),#2838,.T.);
#22923=ADVANCED_FACE('',(#4142),#2839,.T.);
#22924=ADVANCED_FACE('',(#4143),#2840,.T.);
#22925=ADVANCED_FACE('',(#4144),#2841,.T.);
#22926=ADVANCED_FACE('',(#4145),#2842,.T.);
#22927=ADVANCED_FACE('',(#4146),#2843,.F.);
#22928=ADVANCED_FACE('',(#4147),#2844,.T.);
#22929=ADVANCED_FACE('',(#4148),#2845,.T.);
#22930=ADVANCED_FACE('',(#4149),#2846,.T.);
#22931=ADVANCED_FACE('',(#4150),#2847,.F.);
#22932=ADVANCED_FACE('',(#4151),#2848,.F.);
#22933=ADVANCED_FACE('',(#4152),#2849,.F.);
#22934=ADVANCED_FACE('',(#4153),#2850,.F.);
#22935=ADVANCED_FACE('',(#4154),#2851,.F.);
#22936=ADVANCED_FACE('',(#4155),#2852,.F.);
#22937=ADVANCED_FACE('',(#4156),#2853,.F.);
#22938=ADVANCED_FACE('',(#4157,#2292),#2854,.T.);
#22939=ADVANCED_FACE('',(#4158),#1490,.T.);
#22940=ADVANCED_FACE('',(#4159),#21645,.T.);
#22941=ADVANCED_FACE('',(#4160),#1491,.T.);
#22942=ADVANCED_FACE('',(#4161),#2855,.T.);
#22943=ADVANCED_FACE('',(#4162),#21646,.F.);
#22944=ADVANCED_FACE('',(#4163),#21647,.T.);
#22945=ADVANCED_FACE('',(#4164,#2293),#2856,.T.);
#22946=ADVANCED_FACE('',(#4165,#2294),#2857,.F.);
#22947=ADVANCED_FACE('',(#4166),#2858,.T.);
#22948=ADVANCED_FACE('',(#4167),#1492,.T.);
#22949=ADVANCED_FACE('',(#4168),#21648,.T.);
#22950=ADVANCED_FACE('',(#4169),#1493,.T.);
#22951=ADVANCED_FACE('',(#4170,#2295),#2859,.T.);
#22952=ADVANCED_FACE('',(#4171),#1494,.T.);
#22953=ADVANCED_FACE('',(#4172),#21649,.T.);
#22954=ADVANCED_FACE('',(#4173),#1495,.T.);
#22955=ADVANCED_FACE('',(#4174),#2860,.T.);
#22956=ADVANCED_FACE('',(#4175),#2861,.F.);
#22957=ADVANCED_FACE('',(#4176),#2862,.F.);
#22958=ADVANCED_FACE('',(#4177),#2863,.F.);
#22959=ADVANCED_FACE('',(#4178),#2864,.F.);
#22960=ADVANCED_FACE('',(#4179),#2865,.F.);
#22961=ADVANCED_FACE('',(#4180),#2866,.F.);
#22962=ADVANCED_FACE('',(#4181),#2867,.F.);
#22963=ADVANCED_FACE('',(#4182),#2868,.F.);
#22964=CLOSED_SHELL('',(#21650,#21651,#21652,#21653,#21654,#21655,#21656,
#21657,#21658,#21659,#21660,#21661,#21662,#21663,#21664,#21665));
#22965=CLOSED_SHELL('',(#21666,#21667,#21668,#21669,#21670,#21671));
#22966=CLOSED_SHELL('',(#21672,#21673,#21674,#21675,#21676,#21677));
#22967=CLOSED_SHELL('',(#21678,#21679,#21680,#21681,#21682,#21683,#21684,
#21685,#21686,#21687,#21688,#21689,#21690,#21691,#21692,#21693,#21694,#21695,
#21696,#21697,#21698,#21699,#21700,#21701));
#22968=CLOSED_SHELL('',(#21702,#21703,#21704,#21705,#21706,#21707,#21708,
#21709,#21710,#21711,#21712,#21713,#21714,#21715,#21716,#21717));
#22969=CLOSED_SHELL('',(#21718,#21719,#21720,#21721,#21722,#21723,#21724,
#21725,#21726));
#22970=CLOSED_SHELL('',(#21727,#21728,#21729,#21730,#21731,#21732,#21733,
#21734,#21735,#21736,#21737,#21738,#21739,#21740,#21741,#21742));
#22971=CLOSED_SHELL('',(#21743,#21744,#21745,#21746,#21747,#21748,#21749,
#21750,#21751,#21752));
#22972=CLOSED_SHELL('',(#21753,#21754,#21755,#21756,#21757,#21758,#21759,
#21760,#21761));
#22973=CLOSED_SHELL('',(#21762,#21763,#21764,#21765,#21766,#21767,#21768,
#21769,#21770));
#22974=CLOSED_SHELL('',(#21771,#21772,#21773,#21774,#21775,#21776,#21777,
#21778,#21779,#21780,#21781,#21782,#21783,#21784,#21785,#21786,#21787,#21788,
#21789,#21790,#21791,#21792,#21793,#21794,#21795,#21796));
#22975=CLOSED_SHELL('',(#21797,#21798,#21799,#21800,#21801,#21802,#21803,
#21804));
#22976=CLOSED_SHELL('',(#21805,#21806,#21807,#21808,#21809,#21810,#21811,
#21812));
#22977=CLOSED_SHELL('',(#21813));
#22978=CLOSED_SHELL('',(#21814));
#22979=CLOSED_SHELL('',(#21815));
#22980=CLOSED_SHELL('',(#21816));
#22981=CLOSED_SHELL('',(#21817));
#22982=CLOSED_SHELL('',(#21818));
#22983=CLOSED_SHELL('',(#21819));
#22984=CLOSED_SHELL('',(#21820,#21821,#21822,#21823,#21824,#21825,#21826,
#21827,#21828,#21829,#21830,#21831,#21832,#21833,#21834,#21835,#21836));
#22985=CLOSED_SHELL('',(#21837,#21838,#21839,#21840));
#22986=CLOSED_SHELL('',(#21841,#21842,#21843,#21844));
#22987=CLOSED_SHELL('',(#21845,#21846,#21847,#21848,#21849,#21850,#21851,
#21852));
#22988=CLOSED_SHELL('',(#21853,#21854,#21855,#21856,#21857,#21858,#21859,
#21860));
#22989=CLOSED_SHELL('',(#21861));
#22990=CLOSED_SHELL('',(#21862));
#22991=CLOSED_SHELL('',(#21863));
#22992=CLOSED_SHELL('',(#21864));
#22993=CLOSED_SHELL('',(#21865));
#22994=CLOSED_SHELL('',(#21866));
#22995=CLOSED_SHELL('',(#21867));
#22996=CLOSED_SHELL('',(#21868));
#22997=CLOSED_SHELL('',(#21869,#21870,#21871,#21872,#21873,#21874,#21875,
#21876,#21877,#21878,#21879,#21880,#21881,#21882,#21883,#21884,#21885,#21886,
#21887));
#22998=CLOSED_SHELL('',(#21888,#21889,#21890,#21891));
#22999=CLOSED_SHELL('',(#21892,#21893,#21894,#21895));
#23000=CLOSED_SHELL('',(#21896,#21897,#21898,#21899,#21900,#21901,#21902,
#21903,#21904,#21905));
#23001=CLOSED_SHELL('',(#21906,#21907,#21908,#21909,#21910,#21911,#21912,
#21913,#21914,#21915,#21916,#21917,#21918,#21919,#21920,#21921,#21922,#21923));
#23002=CLOSED_SHELL('',(#21924,#21925,#21926,#21927,#21928,#21929,#21930,
#21931,#21932,#21933,#21934,#21935,#21936,#21937,#21938,#21939,#21940,#21941,
#21942,#21943,#21944));
#23003=CLOSED_SHELL('',(#21945,#21946,#21947,#21948,#21949,#21950,#21951,
#21952,#21953,#21954,#21955,#21956,#21957,#21958,#21959,#21960,#21961,#21962,
#21963,#21964,#21965,#21966));
#23004=CLOSED_SHELL('',(#21967,#21968,#21969,#21970,#21971,#21972,#21973,
#21974,#21975,#21976));
#23005=CLOSED_SHELL('',(#21977,#21978,#21979,#21980,#21981,#21982,#21983,
#21984,#21985,#21986));
#23006=CLOSED_SHELL('',(#21987,#21988,#21989,#21990,#21991));
#23007=CLOSED_SHELL('',(#21992,#21993,#21994,#21995,#21996,#21997,#21998,
#21999));
#23008=CLOSED_SHELL('',(#22000,#22001,#22002,#22003,#22004,#22005,#22006,
#22007,#22008,#22009));
#23009=CLOSED_SHELL('',(#22010,#22011,#22012,#22013,#22014,#22015,#22016,
#22017,#22018,#22019,#22020,#22021,#22022,#22023,#22024,#22025,#22026,#22027,
#22028,#22029,#22030,#22031,#22032,#22033,#22034,#22035,#22036,#22037,#22038,
#22039,#22040));
#23010=CLOSED_SHELL('',(#22041,#22042,#22043,#22044,#22045,#22046,#22047,
#22048,#22049));
#23011=CLOSED_SHELL('',(#22050,#22051,#22052,#22053,#22054,#22055,#22056,
#22057));
#23012=CLOSED_SHELL('',(#22058,#22059,#22060,#22061,#22062,#22063,#22064,
#22065,#22066));
#23013=CLOSED_SHELL('',(#22067,#22068,#22069,#22070,#22071,#22072,#22073,
#22074));
#23014=CLOSED_SHELL('',(#22075,#22076,#22077,#22078,#22079,#22080,#22081,
#22082,#22083,#22084,#22085,#22086,#22087,#22088,#22089,#22090,#22091,#22092,
#22093,#22094,#22095,#22096,#22097,#22098,#22099,#22100,#22101,#22102,#22103,
#22104,#22105,#22106,#22107,#22108,#22109,#22110,#22111,#22112,#22113,#22114,
#22115,#22116,#22117,#22118,#22119,#22120,#22121,#22122,#22123,#22124,#22125,
#22126,#22127,#22128,#22129,#22130,#22131,#22132,#22133,#22134,#22135,#22136,
#22137,#22138,#22139,#22140,#22141,#22142,#22143,#22144,#22145,#22146,#22147,
#22148,#22149,#22150,#22151,#22152,#22153,#22154,#22155,#22156,#22157,#22158,
#22159,#22160,#22161,#22162,#22163,#22164,#22165,#22166,#22167,#22168,#22169,
#22170,#22171,#22172,#22173,#22174,#22175,#22176,#22177,#22178,#22179,#22180,
#22181,#22182,#22183,#22184,#22185,#22186,#22187,#22188,#22189,#22190,#22191,
#22192,#22193,#22194,#22195,#22196,#22197,#22198,#22199,#22200,#22201,#22202,
#22203,#22204,#22205,#22206,#22207,#22208,#22209,#22210,#22211,#22212,#22213,
#22214,#22215,#22216,#22217));
#23015=CLOSED_SHELL('',(#22218,#22219,#22220,#22221));
#23016=CLOSED_SHELL('',(#22222,#22223,#22224,#22225,#22226,#22227,#22228));
#23017=CLOSED_SHELL('',(#22229,#22230,#22231,#22232,#22233,#22234,#22235,
#22236,#22237,#22238,#22239,#22240,#22241));
#23018=CLOSED_SHELL('',(#22242,#22243,#22244,#22245));
#23019=CLOSED_SHELL('',(#22246,#22247,#22248,#22249));
#23020=CLOSED_SHELL('',(#22250,#22251,#22252,#22253,#22254,#22255,#22256,
#22257,#22258,#22259));
#23021=CLOSED_SHELL('',(#22260,#22261,#22262,#22263,#22264,#22265,#22266,
#22267,#22268,#22269,#22270,#22271));
#23022=CLOSED_SHELL('',(#22272,#22273,#22274,#22275));
#23023=CLOSED_SHELL('',(#22276,#22277,#22278,#22279,#22280,#22281,#22282,
#22283,#22284));
#23024=CLOSED_SHELL('',(#22285,#22286,#22287,#22288,#22289,#22290,#22291,
#22292));
#23025=CLOSED_SHELL('',(#22293,#22294,#22295,#22296,#22297,#22298,#22299,
#22300,#22301,#22302,#22303,#22304,#22305,#22306,#22307,#22308,#22309,#22310,
#22311,#22312,#22313,#22314,#22315,#22316,#22317,#22318,#22319,#22320,#22321,
#22322,#22323,#22324,#22325,#22326,#22327,#22328,#22329,#22330,#22331,#22332,
#22333,#22334,#22335,#22336));
#23026=CLOSED_SHELL('',(#22337,#22338,#22339,#22340,#22341,#22342,#22343,
#22344,#22345,#22346,#22347,#22348,#22349,#22350,#22351,#22352,#22353,#22354,
#22355,#22356,#22357,#22358,#22359,#22360));
#23027=CLOSED_SHELL('',(#22361,#22362,#22363,#22364,#22365,#22366,#22367,
#22368,#22369,#22370,#22371,#22372,#22373,#22374,#22375,#22376));
#23028=CLOSED_SHELL('',(#22377,#22378,#22379,#22380,#22381,#22382,#22383,
#22384,#22385));
#23029=CLOSED_SHELL('',(#22386,#22387,#22388,#22389,#22390,#22391,#22392,
#22393,#22394,#22395,#22396,#22397,#22398,#22399,#22400,#22401));
#23030=CLOSED_SHELL('',(#22402,#22403,#22404,#22405,#22406,#22407,#22408,
#22409,#22410,#22411));
#23031=CLOSED_SHELL('',(#22412,#22413,#22414,#22415,#22416,#22417,#22418,
#22419,#22420));
#23032=CLOSED_SHELL('',(#22421,#22422,#22423,#22424,#22425,#22426,#22427,
#22428,#22429));
#23033=CLOSED_SHELL('',(#22430,#22431,#22432,#22433,#22434,#22435,#22436,
#22437,#22438,#22439,#22440,#22441,#22442,#22443,#22444,#22445,#22446,#22447,
#22448,#22449,#22450,#22451,#22452,#22453,#22454,#22455));
#23034=CLOSED_SHELL('',(#22456,#22457,#22458,#22459,#22460,#22461,#22462,
#22463));
#23035=CLOSED_SHELL('',(#22464,#22465,#22466,#22467,#22468,#22469,#22470,
#22471));
#23036=CLOSED_SHELL('',(#22472));
#23037=CLOSED_SHELL('',(#22473));
#23038=CLOSED_SHELL('',(#22474));
#23039=CLOSED_SHELL('',(#22475));
#23040=CLOSED_SHELL('',(#22476));
#23041=CLOSED_SHELL('',(#22477));
#23042=CLOSED_SHELL('',(#22478));
#23043=CLOSED_SHELL('',(#22479,#22480,#22481,#22482,#22483,#22484,#22485,
#22486,#22487,#22488,#22489,#22490,#22491,#22492,#22493,#22494,#22495));
#23044=CLOSED_SHELL('',(#22496,#22497,#22498,#22499));
#23045=CLOSED_SHELL('',(#22500,#22501,#22502,#22503));
#23046=CLOSED_SHELL('',(#22504,#22505,#22506,#22507,#22508,#22509,#22510,
#22511));
#23047=CLOSED_SHELL('',(#22512,#22513,#22514,#22515,#22516,#22517,#22518,
#22519));
#23048=CLOSED_SHELL('',(#22520));
#23049=CLOSED_SHELL('',(#22521));
#23050=CLOSED_SHELL('',(#22522));
#23051=CLOSED_SHELL('',(#22523));
#23052=CLOSED_SHELL('',(#22524));
#23053=CLOSED_SHELL('',(#22525));
#23054=CLOSED_SHELL('',(#22526));
#23055=CLOSED_SHELL('',(#22527));
#23056=CLOSED_SHELL('',(#22528,#22529,#22530,#22531,#22532,#22533,#22534,
#22535,#22536,#22537,#22538,#22539,#22540,#22541,#22542,#22543,#22544,#22545,
#22546));
#23057=CLOSED_SHELL('',(#22547,#22548,#22549,#22550));
#23058=CLOSED_SHELL('',(#22551,#22552,#22553,#22554));
#23059=CLOSED_SHELL('',(#22555,#22556,#22557,#22558,#22559,#22560,#22561,
#22562));
#23060=CLOSED_SHELL('',(#22563,#22564,#22565,#22566,#22567,#22568,#22569,
#22570));
#23061=CLOSED_SHELL('',(#22571,#22572,#22573,#22574,#22575,#22576,#22577,
#22578,#22579,#22580));
#23062=CLOSED_SHELL('',(#22581,#22582,#22583,#22584,#22585,#22586,#22587,
#22588,#22589,#22590,#22591,#22592,#22593,#22594));
#23063=CLOSED_SHELL('',(#22595,#22596,#22597,#22598,#22599,#22600,#22601,
#22602,#22603,#22604,#22605,#22606,#22607,#22608,#22609,#22610,#22611,#22612,
#22613,#22614,#22615));
#23064=CLOSED_SHELL('',(#22616,#22617,#22618,#22619,#22620,#22621,#22622,
#22623,#22624,#22625,#22626,#22627,#22628,#22629,#22630,#22631,#22632,#22633,
#22634,#22635,#22636,#22637));
#23065=CLOSED_SHELL('',(#22638,#22639,#22640,#22641,#22642,#22643,#22644,
#22645,#22646,#22647));
#23066=CLOSED_SHELL('',(#22648,#22649,#22650,#22651,#22652,#22653,#22654,
#22655,#22656,#22657));
#23067=CLOSED_SHELL('',(#22658,#22659,#22660,#22661,#22662));
#23068=CLOSED_SHELL('',(#22663,#22664,#22665,#22666,#22667,#22668,#22669,
#22670));
#23069=CLOSED_SHELL('',(#22671,#22672,#22673,#22674,#22675,#22676,#22677,
#22678,#22679,#22680));
#23070=CLOSED_SHELL('',(#22681,#22682,#22683,#22684,#22685,#22686,#22687,
#22688,#22689,#22690,#22691,#22692,#22693,#22694,#22695,#22696,#22697,#22698,
#22699,#22700,#22701,#22702,#22703,#22704,#22705,#22706,#22707,#22708,#22709,
#22710,#22711));
#23071=CLOSED_SHELL('',(#22712,#22713,#22714,#22715,#22716,#22717,#22718,
#22719,#22720));
#23072=CLOSED_SHELL('',(#22721,#22722,#22723,#22724,#22725,#22726,#22727,
#22728));
#23073=CLOSED_SHELL('',(#22729,#22730,#22731,#22732,#22733,#22734,#22735,
#22736,#22737));
#23074=CLOSED_SHELL('',(#22738,#22739,#22740,#22741,#22742,#22743,#22744,
#22745));
#23075=CLOSED_SHELL('',(#22746,#22747,#22748,#22749,#22750,#22751,#22752,
#22753,#22754,#22755,#22756,#22757,#22758,#22759,#22760,#22761,#22762,#22763,
#22764,#22765,#22766,#22767,#22768,#22769,#22770,#22771,#22772,#22773,#22774,
#22775,#22776,#22777,#22778,#22779,#22780,#22781,#22782,#22783,#22784,#22785,
#22786,#22787,#22788,#22789,#22790,#22791,#22792,#22793,#22794,#22795,#22796,
#22797,#22798,#22799,#22800,#22801,#22802,#22803,#22804,#22805,#22806,#22807,
#22808,#22809,#22810,#22811,#22812,#22813,#22814,#22815,#22816,#22817,#22818,
#22819,#22820,#22821,#22822,#22823,#22824,#22825,#22826,#22827,#22828,#22829,
#22830,#22831,#22832,#22833,#22834,#22835,#22836,#22837,#22838,#22839,#22840,
#22841,#22842,#22843,#22844,#22845,#22846,#22847,#22848,#22849,#22850,#22851,
#22852,#22853,#22854,#22855,#22856,#22857,#22858,#22859,#22860,#22861,#22862,
#22863,#22864,#22865,#22866,#22867,#22868,#22869,#22870,#22871,#22872,#22873,
#22874,#22875,#22876,#22877,#22878,#22879,#22880,#22881,#22882,#22883,#22884,
#22885,#22886,#22887,#22888));
#23076=CLOSED_SHELL('',(#22889,#22890,#22891,#22892));
#23077=CLOSED_SHELL('',(#22893,#22894,#22895,#22896,#22897,#22898,#22899));
#23078=CLOSED_SHELL('',(#22900,#22901,#22902,#22903,#22904,#22905,#22906,
#22907,#22908,#22909,#22910,#22911,#22912));
#23079=CLOSED_SHELL('',(#22913,#22914,#22915,#22916));
#23080=CLOSED_SHELL('',(#22917,#22918,#22919,#22920));
#23081=CLOSED_SHELL('',(#22921,#22922,#22923,#22924,#22925,#22926,#22927,
#22928,#22929,#22930));
#23082=CLOSED_SHELL('',(#22931,#22932,#22933,#22934,#22935,#22936,#22937,
#22938,#22939,#22940,#22941,#22942));
#23083=CLOSED_SHELL('',(#22943,#22944,#22945,#22946));
#23084=CLOSED_SHELL('',(#22947,#22948,#22949,#22950,#22951,#22952,#22953,
#22954,#22955));
#23085=CLOSED_SHELL('',(#22956,#22957,#22958,#22959,#22960,#22961,#22962,
#22963));
#23086=DERIVED_UNIT_ELEMENT(#23252,1.);
#23087=DERIVED_UNIT_ELEMENT(#62986,-3.);
#23088=DERIVED_UNIT_ELEMENT(#23252,1.);
#23089=DERIVED_UNIT_ELEMENT(#62986,-3.);
#23090=DERIVED_UNIT_ELEMENT(#23252,1.);
#23091=DERIVED_UNIT_ELEMENT(#62986,-3.);
#23092=DERIVED_UNIT_ELEMENT(#23252,1.);
#23093=DERIVED_UNIT_ELEMENT(#62986,-3.);
#23094=DERIVED_UNIT_ELEMENT(#23252,1.);
#23095=DERIVED_UNIT_ELEMENT(#62986,-3.);
#23096=DERIVED_UNIT_ELEMENT(#23252,1.);
#23097=DERIVED_UNIT_ELEMENT(#62986,-3.);
#23098=DERIVED_UNIT_ELEMENT(#23252,1.);
#23099=DERIVED_UNIT_ELEMENT(#62986,-3.);
#23100=DERIVED_UNIT_ELEMENT(#23252,1.);
#23101=DERIVED_UNIT_ELEMENT(#62986,-3.);
#23102=DERIVED_UNIT_ELEMENT(#23252,1.);
#23103=DERIVED_UNIT_ELEMENT(#62986,-3.);
#23104=DERIVED_UNIT_ELEMENT(#23252,1.);
#23105=DERIVED_UNIT_ELEMENT(#62986,-3.);
#23106=DERIVED_UNIT_ELEMENT(#23252,1.);
#23107=DERIVED_UNIT_ELEMENT(#62986,-3.);
#23108=DERIVED_UNIT_ELEMENT(#23252,1.);
#23109=DERIVED_UNIT_ELEMENT(#62986,-3.);
#23110=DERIVED_UNIT_ELEMENT(#23252,1.);
#23111=DERIVED_UNIT_ELEMENT(#62986,-3.);
#23112=DERIVED_UNIT_ELEMENT(#23252,1.);
#23113=DERIVED_UNIT_ELEMENT(#62986,-3.);
#23114=DERIVED_UNIT_ELEMENT(#23252,1.);
#23115=DERIVED_UNIT_ELEMENT(#62986,-3.);
#23116=DERIVED_UNIT_ELEMENT(#23252,1.);
#23117=DERIVED_UNIT_ELEMENT(#62986,-3.);
#23118=DERIVED_UNIT_ELEMENT(#23252,1.);
#23119=DERIVED_UNIT_ELEMENT(#62986,-3.);
#23120=DERIVED_UNIT_ELEMENT(#23252,1.);
#23121=DERIVED_UNIT_ELEMENT(#62986,-3.);
#23122=DERIVED_UNIT_ELEMENT(#23252,1.);
#23123=DERIVED_UNIT_ELEMENT(#62986,-3.);
#23124=DERIVED_UNIT_ELEMENT(#23252,1.);
#23125=DERIVED_UNIT_ELEMENT(#62986,-3.);
#23126=DERIVED_UNIT_ELEMENT(#23252,1.);
#23127=DERIVED_UNIT_ELEMENT(#62986,-3.);
#23128=DERIVED_UNIT_ELEMENT(#23252,1.);
#23129=DERIVED_UNIT_ELEMENT(#62986,-3.);
#23130=DERIVED_UNIT_ELEMENT(#23252,1.);
#23131=DERIVED_UNIT_ELEMENT(#62986,-3.);
#23132=DERIVED_UNIT_ELEMENT(#23252,1.);
#23133=DERIVED_UNIT_ELEMENT(#62986,-3.);
#23134=DERIVED_UNIT_ELEMENT(#23252,1.);
#23135=DERIVED_UNIT_ELEMENT(#62986,-3.);
#23136=DERIVED_UNIT_ELEMENT(#23252,1.);
#23137=DERIVED_UNIT_ELEMENT(#62986,-3.);
#23138=DERIVED_UNIT_ELEMENT(#23252,1.);
#23139=DERIVED_UNIT_ELEMENT(#62986,-3.);
#23140=DERIVED_UNIT_ELEMENT(#23252,1.);
#23141=DERIVED_UNIT_ELEMENT(#62986,-3.);
#23142=DERIVED_UNIT_ELEMENT(#23252,1.);
#23143=DERIVED_UNIT_ELEMENT(#62986,-3.);
#23144=DERIVED_UNIT_ELEMENT(#23252,1.);
#23145=DERIVED_UNIT_ELEMENT(#62986,-3.);
#23146=DERIVED_UNIT_ELEMENT(#23252,1.);
#23147=DERIVED_UNIT_ELEMENT(#62986,-3.);
#23148=DERIVED_UNIT_ELEMENT(#23252,1.);
#23149=DERIVED_UNIT_ELEMENT(#62986,-3.);
#23150=DERIVED_UNIT_ELEMENT(#23252,1.);
#23151=DERIVED_UNIT_ELEMENT(#62986,-3.);
#23152=DERIVED_UNIT_ELEMENT(#23252,1.);
#23153=DERIVED_UNIT_ELEMENT(#62986,-3.);
#23154=DERIVED_UNIT_ELEMENT(#23252,1.);
#23155=DERIVED_UNIT_ELEMENT(#62986,-3.);
#23156=DERIVED_UNIT_ELEMENT(#23252,1.);
#23157=DERIVED_UNIT_ELEMENT(#62986,-3.);
#23158=DERIVED_UNIT_ELEMENT(#23252,1.);
#23159=DERIVED_UNIT_ELEMENT(#62986,-3.);
#23160=DERIVED_UNIT_ELEMENT(#23252,1.);
#23161=DERIVED_UNIT_ELEMENT(#62986,-3.);
#23162=DERIVED_UNIT_ELEMENT(#23252,1.);
#23163=DERIVED_UNIT_ELEMENT(#62986,-3.);
#23164=DERIVED_UNIT_ELEMENT(#23252,1.);
#23165=DERIVED_UNIT_ELEMENT(#62986,-3.);
#23166=DERIVED_UNIT_ELEMENT(#23252,1.);
#23167=DERIVED_UNIT_ELEMENT(#62986,-3.);
#23168=DERIVED_UNIT_ELEMENT(#23252,1.);
#23169=DERIVED_UNIT_ELEMENT(#62986,-3.);
#23170=DERIVED_UNIT_ELEMENT(#23252,1.);
#23171=DERIVED_UNIT_ELEMENT(#62986,-3.);
#23172=DERIVED_UNIT_ELEMENT(#23252,1.);
#23173=DERIVED_UNIT_ELEMENT(#62986,-3.);
#23174=DERIVED_UNIT_ELEMENT(#23252,1.);
#23175=DERIVED_UNIT_ELEMENT(#62986,-3.);
#23176=DERIVED_UNIT_ELEMENT(#23252,1.);
#23177=DERIVED_UNIT_ELEMENT(#62986,-3.);
#23178=DERIVED_UNIT_ELEMENT(#23252,1.);
#23179=DERIVED_UNIT_ELEMENT(#62986,-3.);
#23180=DERIVED_UNIT_ELEMENT(#23252,1.);
#23181=DERIVED_UNIT_ELEMENT(#62986,-3.);
#23182=DERIVED_UNIT_ELEMENT(#23252,1.);
#23183=DERIVED_UNIT_ELEMENT(#62986,-3.);
#23184=DERIVED_UNIT_ELEMENT(#23252,1.);
#23185=DERIVED_UNIT_ELEMENT(#62986,-3.);
#23186=DERIVED_UNIT_ELEMENT(#23252,1.);
#23187=DERIVED_UNIT_ELEMENT(#62986,-3.);
#23188=DERIVED_UNIT_ELEMENT(#23252,1.);
#23189=DERIVED_UNIT_ELEMENT(#62986,-3.);
#23190=DERIVED_UNIT_ELEMENT(#23252,1.);
#23191=DERIVED_UNIT_ELEMENT(#62986,-3.);
#23192=DERIVED_UNIT_ELEMENT(#23252,1.);
#23193=DERIVED_UNIT_ELEMENT(#62986,-3.);
#23194=DERIVED_UNIT_ELEMENT(#23252,1.);
#23195=DERIVED_UNIT_ELEMENT(#62986,-3.);
#23196=DERIVED_UNIT_ELEMENT(#23252,1.);
#23197=DERIVED_UNIT_ELEMENT(#62986,-3.);
#23198=DERIVED_UNIT_ELEMENT(#23252,1.);
#23199=DERIVED_UNIT_ELEMENT(#62986,-3.);
#23200=DERIVED_UNIT_ELEMENT(#23252,1.);
#23201=DERIVED_UNIT_ELEMENT(#62986,-3.);
#23202=DERIVED_UNIT_ELEMENT(#23252,1.);
#23203=DERIVED_UNIT_ELEMENT(#62986,-3.);
#23204=DERIVED_UNIT_ELEMENT(#23252,1.);
#23205=DERIVED_UNIT_ELEMENT(#62986,-3.);
#23206=DERIVED_UNIT_ELEMENT(#23252,1.);
#23207=DERIVED_UNIT_ELEMENT(#62986,-3.);
#23208=DERIVED_UNIT_ELEMENT(#23252,1.);
#23209=DERIVED_UNIT_ELEMENT(#62986,-3.);
#23210=DERIVED_UNIT_ELEMENT(#23252,1.);
#23211=DERIVED_UNIT_ELEMENT(#62986,-3.);
#23212=DERIVED_UNIT_ELEMENT(#23252,1.);
#23213=DERIVED_UNIT_ELEMENT(#62986,-3.);
#23214=DERIVED_UNIT_ELEMENT(#23252,1.);
#23215=DERIVED_UNIT_ELEMENT(#62986,-3.);
#23216=DERIVED_UNIT_ELEMENT(#23252,1.);
#23217=DERIVED_UNIT_ELEMENT(#62986,-3.);
#23218=DERIVED_UNIT_ELEMENT(#23252,1.);
#23219=DERIVED_UNIT_ELEMENT(#62986,-3.);
#23220=DERIVED_UNIT_ELEMENT(#23252,1.);
#23221=DERIVED_UNIT_ELEMENT(#62986,-3.);
#23222=DERIVED_UNIT_ELEMENT(#23252,1.);
#23223=DERIVED_UNIT_ELEMENT(#62986,-3.);
#23224=DERIVED_UNIT_ELEMENT(#23252,1.);
#23225=DERIVED_UNIT_ELEMENT(#62986,-3.);
#23226=DERIVED_UNIT_ELEMENT(#23252,1.);
#23227=DERIVED_UNIT_ELEMENT(#62986,-3.);
#23228=DERIVED_UNIT_ELEMENT(#23252,1.);
#23229=DERIVED_UNIT_ELEMENT(#62986,-3.);
#23230=DERIVED_UNIT_ELEMENT(#23252,1.);
#23231=DERIVED_UNIT_ELEMENT(#62986,-3.);
#23232=DERIVED_UNIT_ELEMENT(#23252,1.);
#23233=DERIVED_UNIT_ELEMENT(#62986,-3.);
#23234=DERIVED_UNIT_ELEMENT(#23252,1.);
#23235=DERIVED_UNIT_ELEMENT(#62986,-3.);
#23236=DERIVED_UNIT_ELEMENT(#23252,1.);
#23237=DERIVED_UNIT_ELEMENT(#62986,-3.);
#23238=DERIVED_UNIT_ELEMENT(#23252,1.);
#23239=DERIVED_UNIT_ELEMENT(#62986,-3.);
#23240=DERIVED_UNIT_ELEMENT(#23252,1.);
#23241=DERIVED_UNIT_ELEMENT(#62986,-3.);
#23242=DERIVED_UNIT_ELEMENT(#23252,1.);
#23243=DERIVED_UNIT_ELEMENT(#62986,-3.);
#23244=DERIVED_UNIT_ELEMENT(#23252,1.);
#23245=DERIVED_UNIT_ELEMENT(#62986,-3.);
#23246=DERIVED_UNIT_ELEMENT(#23252,1.);
#23247=DERIVED_UNIT_ELEMENT(#62986,-3.);
#23248=DERIVED_UNIT_ELEMENT(#23252,1.);
#23249=DERIVED_UNIT_ELEMENT(#62986,-3.);
#23250=DERIVED_UNIT_ELEMENT(#23252,1.);
#23251=DERIVED_UNIT_ELEMENT(#62986,-3.);
#23252=(
MASS_UNIT()
NAMED_UNIT(*)
SI_UNIT(.KILO.,.GRAM.)
);
#23253=DERIVED_UNIT((#23086,#23087));
#23254=DERIVED_UNIT((#23088,#23089));
#23255=DERIVED_UNIT((#23090,#23091));
#23256=DERIVED_UNIT((#23092,#23093));
#23257=DERIVED_UNIT((#23094,#23095));
#23258=DERIVED_UNIT((#23096,#23097));
#23259=DERIVED_UNIT((#23098,#23099));
#23260=DERIVED_UNIT((#23100,#23101));
#23261=DERIVED_UNIT((#23102,#23103));
#23262=DERIVED_UNIT((#23104,#23105));
#23263=DERIVED_UNIT((#23106,#23107));
#23264=DERIVED_UNIT((#23108,#23109));
#23265=DERIVED_UNIT((#23110,#23111));
#23266=DERIVED_UNIT((#23112,#23113));
#23267=DERIVED_UNIT((#23114,#23115));
#23268=DERIVED_UNIT((#23116,#23117));
#23269=DERIVED_UNIT((#23118,#23119));
#23270=DERIVED_UNIT((#23120,#23121));
#23271=DERIVED_UNIT((#23122,#23123));
#23272=DERIVED_UNIT((#23124,#23125));
#23273=DERIVED_UNIT((#23126,#23127));
#23274=DERIVED_UNIT((#23128,#23129));
#23275=DERIVED_UNIT((#23130,#23131));
#23276=DERIVED_UNIT((#23132,#23133));
#23277=DERIVED_UNIT((#23134,#23135));
#23278=DERIVED_UNIT((#23136,#23137));
#23279=DERIVED_UNIT((#23138,#23139));
#23280=DERIVED_UNIT((#23140,#23141));
#23281=DERIVED_UNIT((#23142,#23143));
#23282=DERIVED_UNIT((#23144,#23145));
#23283=DERIVED_UNIT((#23146,#23147));
#23284=DERIVED_UNIT((#23148,#23149));
#23285=DERIVED_UNIT((#23150,#23151));
#23286=DERIVED_UNIT((#23152,#23153));
#23287=DERIVED_UNIT((#23154,#23155));
#23288=DERIVED_UNIT((#23156,#23157));
#23289=DERIVED_UNIT((#23158,#23159));
#23290=DERIVED_UNIT((#23160,#23161));
#23291=DERIVED_UNIT((#23162,#23163));
#23292=DERIVED_UNIT((#23164,#23165));
#23293=DERIVED_UNIT((#23166,#23167));
#23294=DERIVED_UNIT((#23168,#23169));
#23295=DERIVED_UNIT((#23170,#23171));
#23296=DERIVED_UNIT((#23172,#23173));
#23297=DERIVED_UNIT((#23174,#23175));
#23298=DERIVED_UNIT((#23176,#23177));
#23299=DERIVED_UNIT((#23178,#23179));
#23300=DERIVED_UNIT((#23180,#23181));
#23301=DERIVED_UNIT((#23182,#23183));
#23302=DERIVED_UNIT((#23184,#23185));
#23303=DERIVED_UNIT((#23186,#23187));
#23304=DERIVED_UNIT((#23188,#23189));
#23305=DERIVED_UNIT((#23190,#23191));
#23306=DERIVED_UNIT((#23192,#23193));
#23307=DERIVED_UNIT((#23194,#23195));
#23308=DERIVED_UNIT((#23196,#23197));
#23309=DERIVED_UNIT((#23198,#23199));
#23310=DERIVED_UNIT((#23200,#23201));
#23311=DERIVED_UNIT((#23202,#23203));
#23312=DERIVED_UNIT((#23204,#23205));
#23313=DERIVED_UNIT((#23206,#23207));
#23314=DERIVED_UNIT((#23208,#23209));
#23315=DERIVED_UNIT((#23210,#23211));
#23316=DERIVED_UNIT((#23212,#23213));
#23317=DERIVED_UNIT((#23214,#23215));
#23318=DERIVED_UNIT((#23216,#23217));
#23319=DERIVED_UNIT((#23218,#23219));
#23320=DERIVED_UNIT((#23220,#23221));
#23321=DERIVED_UNIT((#23222,#23223));
#23322=DERIVED_UNIT((#23224,#23225));
#23323=DERIVED_UNIT((#23226,#23227));
#23324=DERIVED_UNIT((#23228,#23229));
#23325=DERIVED_UNIT((#23230,#23231));
#23326=DERIVED_UNIT((#23232,#23233));
#23327=DERIVED_UNIT((#23234,#23235));
#23328=DERIVED_UNIT((#23236,#23237));
#23329=DERIVED_UNIT((#23238,#23239));
#23330=DERIVED_UNIT((#23240,#23241));
#23331=DERIVED_UNIT((#23242,#23243));
#23332=DERIVED_UNIT((#23244,#23245));
#23333=DERIVED_UNIT((#23246,#23247));
#23334=DERIVED_UNIT((#23248,#23249));
#23335=DERIVED_UNIT((#23250,#23251));
#23336=MEASURE_REPRESENTATION_ITEM('density measure',
POSITIVE_RATIO_MEASURE(7850.),#23253);
#23337=MEASURE_REPRESENTATION_ITEM('density measure',
POSITIVE_RATIO_MEASURE(7850.),#23254);
#23338=MEASURE_REPRESENTATION_ITEM('density measure',
POSITIVE_RATIO_MEASURE(7850.),#23255);
#23339=MEASURE_REPRESENTATION_ITEM('density measure',
POSITIVE_RATIO_MEASURE(7850.),#23256);
#23340=MEASURE_REPRESENTATION_ITEM('density measure',
POSITIVE_RATIO_MEASURE(7850.),#23257);
#23341=MEASURE_REPRESENTATION_ITEM('density measure',
POSITIVE_RATIO_MEASURE(7850.),#23258);
#23342=MEASURE_REPRESENTATION_ITEM('density measure',
POSITIVE_RATIO_MEASURE(7850.),#23259);
#23343=MEASURE_REPRESENTATION_ITEM('density measure',
POSITIVE_RATIO_MEASURE(7850.),#23260);
#23344=MEASURE_REPRESENTATION_ITEM('density measure',
POSITIVE_RATIO_MEASURE(7850.),#23261);
#23345=MEASURE_REPRESENTATION_ITEM('density measure',
POSITIVE_RATIO_MEASURE(7850.),#23262);
#23346=MEASURE_REPRESENTATION_ITEM('density measure',
POSITIVE_RATIO_MEASURE(7850.),#23263);
#23347=MEASURE_REPRESENTATION_ITEM('density measure',
POSITIVE_RATIO_MEASURE(7850.),#23264);
#23348=MEASURE_REPRESENTATION_ITEM('density measure',
POSITIVE_RATIO_MEASURE(7850.),#23265);
#23349=MEASURE_REPRESENTATION_ITEM('density measure',
POSITIVE_RATIO_MEASURE(7850.),#23266);
#23350=MEASURE_REPRESENTATION_ITEM('density measure',
POSITIVE_RATIO_MEASURE(7850.),#23267);
#23351=MEASURE_REPRESENTATION_ITEM('density measure',
POSITIVE_RATIO_MEASURE(7850.),#23268);
#23352=MEASURE_REPRESENTATION_ITEM('density measure',
POSITIVE_RATIO_MEASURE(7850.),#23269);
#23353=MEASURE_REPRESENTATION_ITEM('density measure',
POSITIVE_RATIO_MEASURE(7850.),#23270);
#23354=MEASURE_REPRESENTATION_ITEM('density measure',
POSITIVE_RATIO_MEASURE(7850.),#23271);
#23355=MEASURE_REPRESENTATION_ITEM('density measure',
POSITIVE_RATIO_MEASURE(7850.),#23272);
#23356=MEASURE_REPRESENTATION_ITEM('density measure',
POSITIVE_RATIO_MEASURE(7850.),#23273);
#23357=MEASURE_REPRESENTATION_ITEM('density measure',
POSITIVE_RATIO_MEASURE(7850.),#23274);
#23358=MEASURE_REPRESENTATION_ITEM('density measure',
POSITIVE_RATIO_MEASURE(7850.),#23275);
#23359=MEASURE_REPRESENTATION_ITEM('density measure',
POSITIVE_RATIO_MEASURE(7850.),#23276);
#23360=MEASURE_REPRESENTATION_ITEM('density measure',
POSITIVE_RATIO_MEASURE(7850.),#23277);
#23361=MEASURE_REPRESENTATION_ITEM('density measure',
POSITIVE_RATIO_MEASURE(7850.),#23278);
#23362=MEASURE_REPRESENTATION_ITEM('density measure',
POSITIVE_RATIO_MEASURE(7850.),#23279);
#23363=MEASURE_REPRESENTATION_ITEM('density measure',
POSITIVE_RATIO_MEASURE(7850.),#23280);
#23364=MEASURE_REPRESENTATION_ITEM('density measure',
POSITIVE_RATIO_MEASURE(7850.),#23281);
#23365=MEASURE_REPRESENTATION_ITEM('density measure',
POSITIVE_RATIO_MEASURE(7850.),#23282);
#23366=MEASURE_REPRESENTATION_ITEM('density measure',
POSITIVE_RATIO_MEASURE(7850.),#23283);
#23367=MEASURE_REPRESENTATION_ITEM('density measure',
POSITIVE_RATIO_MEASURE(7850.),#23284);
#23368=MEASURE_REPRESENTATION_ITEM('density measure',
POSITIVE_RATIO_MEASURE(7850.),#23285);
#23369=MEASURE_REPRESENTATION_ITEM('density measure',
POSITIVE_RATIO_MEASURE(7850.),#23286);
#23370=MEASURE_REPRESENTATION_ITEM('density measure',
POSITIVE_RATIO_MEASURE(7850.),#23287);
#23371=MEASURE_REPRESENTATION_ITEM('density measure',
POSITIVE_RATIO_MEASURE(7850.),#23288);
#23372=MEASURE_REPRESENTATION_ITEM('density measure',
POSITIVE_RATIO_MEASURE(7850.),#23289);
#23373=MEASURE_REPRESENTATION_ITEM('density measure',
POSITIVE_RATIO_MEASURE(7850.),#23290);
#23374=MEASURE_REPRESENTATION_ITEM('density measure',
POSITIVE_RATIO_MEASURE(7850.),#23291);
#23375=MEASURE_REPRESENTATION_ITEM('density measure',
POSITIVE_RATIO_MEASURE(7850.),#23292);
#23376=MEASURE_REPRESENTATION_ITEM('density measure',
POSITIVE_RATIO_MEASURE(7850.),#23293);
#23377=MEASURE_REPRESENTATION_ITEM('density measure',
POSITIVE_RATIO_MEASURE(7850.),#23294);
#23378=MEASURE_REPRESENTATION_ITEM('density measure',
POSITIVE_RATIO_MEASURE(7850.),#23295);
#23379=MEASURE_REPRESENTATION_ITEM('density measure',
POSITIVE_RATIO_MEASURE(7850.),#23296);
#23380=MEASURE_REPRESENTATION_ITEM('density measure',
POSITIVE_RATIO_MEASURE(7850.),#23297);
#23381=MEASURE_REPRESENTATION_ITEM('density measure',
POSITIVE_RATIO_MEASURE(7850.),#23298);
#23382=MEASURE_REPRESENTATION_ITEM('density measure',
POSITIVE_RATIO_MEASURE(7850.),#23299);
#23383=MEASURE_REPRESENTATION_ITEM('density measure',
POSITIVE_RATIO_MEASURE(7850.),#23300);
#23384=MEASURE_REPRESENTATION_ITEM('density measure',
POSITIVE_RATIO_MEASURE(7850.),#23301);
#23385=MEASURE_REPRESENTATION_ITEM('density measure',
POSITIVE_RATIO_MEASURE(7850.),#23302);
#23386=MEASURE_REPRESENTATION_ITEM('density measure',
POSITIVE_RATIO_MEASURE(7850.),#23303);
#23387=MEASURE_REPRESENTATION_ITEM('density measure',
POSITIVE_RATIO_MEASURE(7850.),#23304);
#23388=MEASURE_REPRESENTATION_ITEM('density measure',
POSITIVE_RATIO_MEASURE(7850.),#23305);
#23389=MEASURE_REPRESENTATION_ITEM('density measure',
POSITIVE_RATIO_MEASURE(7850.),#23306);
#23390=MEASURE_REPRESENTATION_ITEM('density measure',
POSITIVE_RATIO_MEASURE(7850.),#23307);
#23391=MEASURE_REPRESENTATION_ITEM('density measure',
POSITIVE_RATIO_MEASURE(7850.),#23308);
#23392=MEASURE_REPRESENTATION_ITEM('density measure',
POSITIVE_RATIO_MEASURE(7850.),#23309);
#23393=MEASURE_REPRESENTATION_ITEM('density measure',
POSITIVE_RATIO_MEASURE(7850.),#23310);
#23394=MEASURE_REPRESENTATION_ITEM('density measure',
POSITIVE_RATIO_MEASURE(7850.),#23311);
#23395=MEASURE_REPRESENTATION_ITEM('density measure',
POSITIVE_RATIO_MEASURE(7850.),#23312);
#23396=MEASURE_REPRESENTATION_ITEM('density measure',
POSITIVE_RATIO_MEASURE(7850.),#23313);
#23397=MEASURE_REPRESENTATION_ITEM('density measure',
POSITIVE_RATIO_MEASURE(7850.),#23314);
#23398=MEASURE_REPRESENTATION_ITEM('density measure',
POSITIVE_RATIO_MEASURE(7850.),#23315);
#23399=MEASURE_REPRESENTATION_ITEM('density measure',
POSITIVE_RATIO_MEASURE(7850.),#23316);
#23400=MEASURE_REPRESENTATION_ITEM('density measure',
POSITIVE_RATIO_MEASURE(7850.),#23317);
#23401=MEASURE_REPRESENTATION_ITEM('density measure',
POSITIVE_RATIO_MEASURE(7850.),#23318);
#23402=MEASURE_REPRESENTATION_ITEM('density measure',
POSITIVE_RATIO_MEASURE(7850.),#23319);
#23403=MEASURE_REPRESENTATION_ITEM('density measure',
POSITIVE_RATIO_MEASURE(7850.),#23320);
#23404=MEASURE_REPRESENTATION_ITEM('density measure',
POSITIVE_RATIO_MEASURE(7850.),#23321);
#23405=MEASURE_REPRESENTATION_ITEM('density measure',
POSITIVE_RATIO_MEASURE(7850.),#23322);
#23406=MEASURE_REPRESENTATION_ITEM('density measure',
POSITIVE_RATIO_MEASURE(7850.),#23323);
#23407=MEASURE_REPRESENTATION_ITEM('density measure',
POSITIVE_RATIO_MEASURE(7850.),#23324);
#23408=MEASURE_REPRESENTATION_ITEM('density measure',
POSITIVE_RATIO_MEASURE(7850.),#23325);
#23409=MEASURE_REPRESENTATION_ITEM('density measure',
POSITIVE_RATIO_MEASURE(7850.),#23326);
#23410=MEASURE_REPRESENTATION_ITEM('density measure',
POSITIVE_RATIO_MEASURE(7850.),#23327);
#23411=MEASURE_REPRESENTATION_ITEM('density measure',
POSITIVE_RATIO_MEASURE(7850.),#23328);
#23412=MEASURE_REPRESENTATION_ITEM('density measure',
POSITIVE_RATIO_MEASURE(7850.),#23329);
#23413=MEASURE_REPRESENTATION_ITEM('density measure',
POSITIVE_RATIO_MEASURE(7850.),#23330);
#23414=MEASURE_REPRESENTATION_ITEM('density measure',
POSITIVE_RATIO_MEASURE(7850.),#23331);
#23415=MEASURE_REPRESENTATION_ITEM('density measure',
POSITIVE_RATIO_MEASURE(7850.),#23332);
#23416=MEASURE_REPRESENTATION_ITEM('density measure',
POSITIVE_RATIO_MEASURE(7850.),#23333);
#23417=MEASURE_REPRESENTATION_ITEM('density measure',
POSITIVE_RATIO_MEASURE(7850.),#23334);
#23418=MEASURE_REPRESENTATION_ITEM('density measure',
POSITIVE_RATIO_MEASURE(7850.),#23335);
#23419=PROPERTY_DEFINITION_REPRESENTATION(#23834,#23585);
#23420=PROPERTY_DEFINITION_REPRESENTATION(#23835,#23586);
#23421=PROPERTY_DEFINITION_REPRESENTATION(#23836,#23587);
#23422=PROPERTY_DEFINITION_REPRESENTATION(#23837,#23588);
#23423=PROPERTY_DEFINITION_REPRESENTATION(#23838,#23589);
#23424=PROPERTY_DEFINITION_REPRESENTATION(#23839,#23590);
#23425=PROPERTY_DEFINITION_REPRESENTATION(#23840,#23591);
#23426=PROPERTY_DEFINITION_REPRESENTATION(#23841,#23592);
#23427=PROPERTY_DEFINITION_REPRESENTATION(#23842,#23593);
#23428=PROPERTY_DEFINITION_REPRESENTATION(#23843,#23594);
#23429=PROPERTY_DEFINITION_REPRESENTATION(#23844,#23595);
#23430=PROPERTY_DEFINITION_REPRESENTATION(#23845,#23596);
#23431=PROPERTY_DEFINITION_REPRESENTATION(#23846,#23597);
#23432=PROPERTY_DEFINITION_REPRESENTATION(#23847,#23598);
#23433=PROPERTY_DEFINITION_REPRESENTATION(#23848,#23599);
#23434=PROPERTY_DEFINITION_REPRESENTATION(#23849,#23600);
#23435=PROPERTY_DEFINITION_REPRESENTATION(#23850,#23601);
#23436=PROPERTY_DEFINITION_REPRESENTATION(#23851,#23602);
#23437=PROPERTY_DEFINITION_REPRESENTATION(#23852,#23603);
#23438=PROPERTY_DEFINITION_REPRESENTATION(#23853,#23604);
#23439=PROPERTY_DEFINITION_REPRESENTATION(#23854,#23605);
#23440=PROPERTY_DEFINITION_REPRESENTATION(#23855,#23606);
#23441=PROPERTY_DEFINITION_REPRESENTATION(#23856,#23607);
#23442=PROPERTY_DEFINITION_REPRESENTATION(#23857,#23608);
#23443=PROPERTY_DEFINITION_REPRESENTATION(#23858,#23609);
#23444=PROPERTY_DEFINITION_REPRESENTATION(#23859,#23610);
#23445=PROPERTY_DEFINITION_REPRESENTATION(#23860,#23611);
#23446=PROPERTY_DEFINITION_REPRESENTATION(#23861,#23612);
#23447=PROPERTY_DEFINITION_REPRESENTATION(#23862,#23613);
#23448=PROPERTY_DEFINITION_REPRESENTATION(#23863,#23614);
#23449=PROPERTY_DEFINITION_REPRESENTATION(#23864,#23615);
#23450=PROPERTY_DEFINITION_REPRESENTATION(#23865,#23616);
#23451=PROPERTY_DEFINITION_REPRESENTATION(#23866,#23617);
#23452=PROPERTY_DEFINITION_REPRESENTATION(#23867,#23618);
#23453=PROPERTY_DEFINITION_REPRESENTATION(#23868,#23619);
#23454=PROPERTY_DEFINITION_REPRESENTATION(#23869,#23620);
#23455=PROPERTY_DEFINITION_REPRESENTATION(#23870,#23621);
#23456=PROPERTY_DEFINITION_REPRESENTATION(#23871,#23622);
#23457=PROPERTY_DEFINITION_REPRESENTATION(#23872,#23623);
#23458=PROPERTY_DEFINITION_REPRESENTATION(#23873,#23624);
#23459=PROPERTY_DEFINITION_REPRESENTATION(#23874,#23625);
#23460=PROPERTY_DEFINITION_REPRESENTATION(#23875,#23626);
#23461=PROPERTY_DEFINITION_REPRESENTATION(#23876,#23627);
#23462=PROPERTY_DEFINITION_REPRESENTATION(#23877,#23628);
#23463=PROPERTY_DEFINITION_REPRESENTATION(#23878,#23629);
#23464=PROPERTY_DEFINITION_REPRESENTATION(#23879,#23630);
#23465=PROPERTY_DEFINITION_REPRESENTATION(#23880,#23631);
#23466=PROPERTY_DEFINITION_REPRESENTATION(#23881,#23632);
#23467=PROPERTY_DEFINITION_REPRESENTATION(#23882,#23633);
#23468=PROPERTY_DEFINITION_REPRESENTATION(#23883,#23634);
#23469=PROPERTY_DEFINITION_REPRESENTATION(#23884,#23635);
#23470=PROPERTY_DEFINITION_REPRESENTATION(#23885,#23636);
#23471=PROPERTY_DEFINITION_REPRESENTATION(#23886,#23637);
#23472=PROPERTY_DEFINITION_REPRESENTATION(#23887,#23638);
#23473=PROPERTY_DEFINITION_REPRESENTATION(#23888,#23639);
#23474=PROPERTY_DEFINITION_REPRESENTATION(#23889,#23640);
#23475=PROPERTY_DEFINITION_REPRESENTATION(#23890,#23641);
#23476=PROPERTY_DEFINITION_REPRESENTATION(#23891,#23642);
#23477=PROPERTY_DEFINITION_REPRESENTATION(#23892,#23643);
#23478=PROPERTY_DEFINITION_REPRESENTATION(#23893,#23644);
#23479=PROPERTY_DEFINITION_REPRESENTATION(#23894,#23645);
#23480=PROPERTY_DEFINITION_REPRESENTATION(#23895,#23646);
#23481=PROPERTY_DEFINITION_REPRESENTATION(#23896,#23647);
#23482=PROPERTY_DEFINITION_REPRESENTATION(#23897,#23648);
#23483=PROPERTY_DEFINITION_REPRESENTATION(#23898,#23649);
#23484=PROPERTY_DEFINITION_REPRESENTATION(#23899,#23650);
#23485=PROPERTY_DEFINITION_REPRESENTATION(#23900,#23651);
#23486=PROPERTY_DEFINITION_REPRESENTATION(#23901,#23652);
#23487=PROPERTY_DEFINITION_REPRESENTATION(#23902,#23653);
#23488=PROPERTY_DEFINITION_REPRESENTATION(#23903,#23654);
#23489=PROPERTY_DEFINITION_REPRESENTATION(#23904,#23655);
#23490=PROPERTY_DEFINITION_REPRESENTATION(#23905,#23656);
#23491=PROPERTY_DEFINITION_REPRESENTATION(#23906,#23657);
#23492=PROPERTY_DEFINITION_REPRESENTATION(#23907,#23658);
#23493=PROPERTY_DEFINITION_REPRESENTATION(#23908,#23659);
#23494=PROPERTY_DEFINITION_REPRESENTATION(#23909,#23660);
#23495=PROPERTY_DEFINITION_REPRESENTATION(#23910,#23661);
#23496=PROPERTY_DEFINITION_REPRESENTATION(#23911,#23662);
#23497=PROPERTY_DEFINITION_REPRESENTATION(#23912,#23663);
#23498=PROPERTY_DEFINITION_REPRESENTATION(#23913,#23664);
#23499=PROPERTY_DEFINITION_REPRESENTATION(#23914,#23665);
#23500=PROPERTY_DEFINITION_REPRESENTATION(#23915,#23666);
#23501=PROPERTY_DEFINITION_REPRESENTATION(#23916,#23667);
#23502=PROPERTY_DEFINITION_REPRESENTATION(#23917,#23668);
#23503=PROPERTY_DEFINITION_REPRESENTATION(#23918,#23669);
#23504=PROPERTY_DEFINITION_REPRESENTATION(#23919,#23670);
#23505=PROPERTY_DEFINITION_REPRESENTATION(#23920,#23671);
#23506=PROPERTY_DEFINITION_REPRESENTATION(#23921,#23672);
#23507=PROPERTY_DEFINITION_REPRESENTATION(#23922,#23673);
#23508=PROPERTY_DEFINITION_REPRESENTATION(#23923,#23674);
#23509=PROPERTY_DEFINITION_REPRESENTATION(#23924,#23675);
#23510=PROPERTY_DEFINITION_REPRESENTATION(#23925,#23676);
#23511=PROPERTY_DEFINITION_REPRESENTATION(#23926,#23677);
#23512=PROPERTY_DEFINITION_REPRESENTATION(#23927,#23678);
#23513=PROPERTY_DEFINITION_REPRESENTATION(#23928,#23679);
#23514=PROPERTY_DEFINITION_REPRESENTATION(#23929,#23680);
#23515=PROPERTY_DEFINITION_REPRESENTATION(#23930,#23681);
#23516=PROPERTY_DEFINITION_REPRESENTATION(#23931,#23682);
#23517=PROPERTY_DEFINITION_REPRESENTATION(#23932,#23683);
#23518=PROPERTY_DEFINITION_REPRESENTATION(#23933,#23684);
#23519=PROPERTY_DEFINITION_REPRESENTATION(#23934,#23685);
#23520=PROPERTY_DEFINITION_REPRESENTATION(#23935,#23686);
#23521=PROPERTY_DEFINITION_REPRESENTATION(#23936,#23687);
#23522=PROPERTY_DEFINITION_REPRESENTATION(#23937,#23688);
#23523=PROPERTY_DEFINITION_REPRESENTATION(#23938,#23689);
#23524=PROPERTY_DEFINITION_REPRESENTATION(#23939,#23690);
#23525=PROPERTY_DEFINITION_REPRESENTATION(#23940,#23691);
#23526=PROPERTY_DEFINITION_REPRESENTATION(#23941,#23692);
#23527=PROPERTY_DEFINITION_REPRESENTATION(#23942,#23693);
#23528=PROPERTY_DEFINITION_REPRESENTATION(#23943,#23694);
#23529=PROPERTY_DEFINITION_REPRESENTATION(#23944,#23695);
#23530=PROPERTY_DEFINITION_REPRESENTATION(#23945,#23696);
#23531=PROPERTY_DEFINITION_REPRESENTATION(#23946,#23697);
#23532=PROPERTY_DEFINITION_REPRESENTATION(#23947,#23698);
#23533=PROPERTY_DEFINITION_REPRESENTATION(#23948,#23699);
#23534=PROPERTY_DEFINITION_REPRESENTATION(#23949,#23700);
#23535=PROPERTY_DEFINITION_REPRESENTATION(#23950,#23701);
#23536=PROPERTY_DEFINITION_REPRESENTATION(#23951,#23702);
#23537=PROPERTY_DEFINITION_REPRESENTATION(#23952,#23703);
#23538=PROPERTY_DEFINITION_REPRESENTATION(#23953,#23704);
#23539=PROPERTY_DEFINITION_REPRESENTATION(#23954,#23705);
#23540=PROPERTY_DEFINITION_REPRESENTATION(#23955,#23706);
#23541=PROPERTY_DEFINITION_REPRESENTATION(#23956,#23707);
#23542=PROPERTY_DEFINITION_REPRESENTATION(#23957,#23708);
#23543=PROPERTY_DEFINITION_REPRESENTATION(#23958,#23709);
#23544=PROPERTY_DEFINITION_REPRESENTATION(#23959,#23710);
#23545=PROPERTY_DEFINITION_REPRESENTATION(#23960,#23711);
#23546=PROPERTY_DEFINITION_REPRESENTATION(#23961,#23712);
#23547=PROPERTY_DEFINITION_REPRESENTATION(#23962,#23713);
#23548=PROPERTY_DEFINITION_REPRESENTATION(#23963,#23714);
#23549=PROPERTY_DEFINITION_REPRESENTATION(#23964,#23715);
#23550=PROPERTY_DEFINITION_REPRESENTATION(#23965,#23716);
#23551=PROPERTY_DEFINITION_REPRESENTATION(#23966,#23717);
#23552=PROPERTY_DEFINITION_REPRESENTATION(#23967,#23718);
#23553=PROPERTY_DEFINITION_REPRESENTATION(#23968,#23719);
#23554=PROPERTY_DEFINITION_REPRESENTATION(#23969,#23720);
#23555=PROPERTY_DEFINITION_REPRESENTATION(#23970,#23721);
#23556=PROPERTY_DEFINITION_REPRESENTATION(#23971,#23722);
#23557=PROPERTY_DEFINITION_REPRESENTATION(#23972,#23723);
#23558=PROPERTY_DEFINITION_REPRESENTATION(#23973,#23724);
#23559=PROPERTY_DEFINITION_REPRESENTATION(#23974,#23725);
#23560=PROPERTY_DEFINITION_REPRESENTATION(#23975,#23726);
#23561=PROPERTY_DEFINITION_REPRESENTATION(#23976,#23727);
#23562=PROPERTY_DEFINITION_REPRESENTATION(#23977,#23728);
#23563=PROPERTY_DEFINITION_REPRESENTATION(#23978,#23729);
#23564=PROPERTY_DEFINITION_REPRESENTATION(#23979,#23730);
#23565=PROPERTY_DEFINITION_REPRESENTATION(#23980,#23731);
#23566=PROPERTY_DEFINITION_REPRESENTATION(#23981,#23732);
#23567=PROPERTY_DEFINITION_REPRESENTATION(#23982,#23733);
#23568=PROPERTY_DEFINITION_REPRESENTATION(#23983,#23734);
#23569=PROPERTY_DEFINITION_REPRESENTATION(#23984,#23735);
#23570=PROPERTY_DEFINITION_REPRESENTATION(#23985,#23736);
#23571=PROPERTY_DEFINITION_REPRESENTATION(#23986,#23737);
#23572=PROPERTY_DEFINITION_REPRESENTATION(#23987,#23738);
#23573=PROPERTY_DEFINITION_REPRESENTATION(#23988,#23739);
#23574=PROPERTY_DEFINITION_REPRESENTATION(#23989,#23740);
#23575=PROPERTY_DEFINITION_REPRESENTATION(#23990,#23741);
#23576=PROPERTY_DEFINITION_REPRESENTATION(#23991,#23742);
#23577=PROPERTY_DEFINITION_REPRESENTATION(#23992,#23743);
#23578=PROPERTY_DEFINITION_REPRESENTATION(#23993,#23744);
#23579=PROPERTY_DEFINITION_REPRESENTATION(#23994,#23745);
#23580=PROPERTY_DEFINITION_REPRESENTATION(#23995,#23746);
#23581=PROPERTY_DEFINITION_REPRESENTATION(#23996,#23747);
#23582=PROPERTY_DEFINITION_REPRESENTATION(#23997,#23748);
#23583=PROPERTY_DEFINITION_REPRESENTATION(#23998,#23749);
#23584=PROPERTY_DEFINITION_REPRESENTATION(#23999,#23750);
#23585=REPRESENTATION('material name',(#23751),#62889);
#23586=REPRESENTATION('density',(#23336),#62889);
#23587=REPRESENTATION('material name',(#23752),#62890);
#23588=REPRESENTATION('density',(#23337),#62890);
#23589=REPRESENTATION('material name',(#23753),#62891);
#23590=REPRESENTATION('density',(#23338),#62891);
#23591=REPRESENTATION('material name',(#23754),#62892);
#23592=REPRESENTATION('density',(#23339),#62892);
#23593=REPRESENTATION('material name',(#23755),#62893);
#23594=REPRESENTATION('density',(#23340),#62893);
#23595=REPRESENTATION('material name',(#23756),#62894);
#23596=REPRESENTATION('density',(#23341),#62894);
#23597=REPRESENTATION('material name',(#23757),#62895);
#23598=REPRESENTATION('density',(#23342),#62895);
#23599=REPRESENTATION('material name',(#23758),#62896);
#23600=REPRESENTATION('density',(#23343),#62896);
#23601=REPRESENTATION('material name',(#23759),#62897);
#23602=REPRESENTATION('density',(#23344),#62897);
#23603=REPRESENTATION('material name',(#23760),#62898);
#23604=REPRESENTATION('density',(#23345),#62898);
#23605=REPRESENTATION('material name',(#23761),#62899);
#23606=REPRESENTATION('density',(#23346),#62899);
#23607=REPRESENTATION('material name',(#23762),#62901);
#23608=REPRESENTATION('density',(#23347),#62901);
#23609=REPRESENTATION('material name',(#23763),#62902);
#23610=REPRESENTATION('density',(#23348),#62902);
#23611=REPRESENTATION('material name',(#23764),#62903);
#23612=REPRESENTATION('density',(#23349),#62903);
#23613=REPRESENTATION('material name',(#23765),#62904);
#23614=REPRESENTATION('density',(#23350),#62904);
#23615=REPRESENTATION('material name',(#23766),#62905);
#23616=REPRESENTATION('density',(#23351),#62905);
#23617=REPRESENTATION('material name',(#23767),#62907);
#23618=REPRESENTATION('density',(#23352),#62907);
#23619=REPRESENTATION('material name',(#23768),#62908);
#23620=REPRESENTATION('density',(#23353),#62908);
#23621=REPRESENTATION('material name',(#23769),#62909);
#23622=REPRESENTATION('density',(#23354),#62909);
#23623=REPRESENTATION('material name',(#23770),#62910);
#23624=REPRESENTATION('density',(#23355),#62910);
#23625=REPRESENTATION('material name',(#23771),#62911);
#23626=REPRESENTATION('density',(#23356),#62911);
#23627=REPRESENTATION('material name',(#23772),#62913);
#23628=REPRESENTATION('density',(#23357),#62913);
#23629=REPRESENTATION('material name',(#23773),#62914);
#23630=REPRESENTATION('density',(#23358),#62914);
#23631=REPRESENTATION('material name',(#23774),#62915);
#23632=REPRESENTATION('density',(#23359),#62915);
#23633=REPRESENTATION('material name',(#23775),#62917);
#23634=REPRESENTATION('density',(#23360),#62917);
#23635=REPRESENTATION('material name',(#23776),#62918);
#23636=REPRESENTATION('density',(#23361),#62918);
#23637=REPRESENTATION('material name',(#23777),#62919);
#23638=REPRESENTATION('density',(#23362),#62919);
#23639=REPRESENTATION('material name',(#23778),#62920);
#23640=REPRESENTATION('density',(#23363),#62920);
#23641=REPRESENTATION('material name',(#23779),#62921);
#23642=REPRESENTATION('density',(#23364),#62921);
#23643=REPRESENTATION('material name',(#23780),#62922);
#23644=REPRESENTATION('density',(#23365),#62922);
#23645=REPRESENTATION('material name',(#23781),#62923);
#23646=REPRESENTATION('density',(#23366),#62923);
#23647=REPRESENTATION('material name',(#23782),#62924);
#23648=REPRESENTATION('density',(#23367),#62924);
#23649=REPRESENTATION('material name',(#23783),#62926);
#23650=REPRESENTATION('density',(#23368),#62926);
#23651=REPRESENTATION('material name',(#23784),#62927);
#23652=REPRESENTATION('density',(#23369),#62927);
#23653=REPRESENTATION('material name',(#23785),#62928);
#23654=REPRESENTATION('density',(#23370),#62928);
#23655=REPRESENTATION('material name',(#23786),#62929);
#23656=REPRESENTATION('density',(#23371),#62929);
#23657=REPRESENTATION('material name',(#23787),#62930);
#23658=REPRESENTATION('density',(#23372),#62930);
#23659=REPRESENTATION('material name',(#23788),#62931);
#23660=REPRESENTATION('density',(#23373),#62931);
#23661=REPRESENTATION('material name',(#23789),#62932);
#23662=REPRESENTATION('density',(#23374),#62932);
#23663=REPRESENTATION('material name',(#23790),#62933);
#23664=REPRESENTATION('density',(#23375),#62933);
#23665=REPRESENTATION('material name',(#23791),#62934);
#23666=REPRESENTATION('density',(#23376),#62934);
#23667=REPRESENTATION('material name',(#23792),#62935);
#23668=REPRESENTATION('density',(#23377),#62935);
#23669=REPRESENTATION('material name',(#23793),#62938);
#23670=REPRESENTATION('density',(#23378),#62938);
#23671=REPRESENTATION('material name',(#23794),#62939);
#23672=REPRESENTATION('density',(#23379),#62939);
#23673=REPRESENTATION('material name',(#23795),#62940);
#23674=REPRESENTATION('density',(#23380),#62940);
#23675=REPRESENTATION('material name',(#23796),#62941);
#23676=REPRESENTATION('density',(#23381),#62941);
#23677=REPRESENTATION('material name',(#23797),#62942);
#23678=REPRESENTATION('density',(#23382),#62942);
#23679=REPRESENTATION('material name',(#23798),#62943);
#23680=REPRESENTATION('density',(#23383),#62943);
#23681=REPRESENTATION('material name',(#23799),#62944);
#23682=REPRESENTATION('density',(#23384),#62944);
#23683=REPRESENTATION('material name',(#23800),#62945);
#23684=REPRESENTATION('density',(#23385),#62945);
#23685=REPRESENTATION('material name',(#23801),#62946);
#23686=REPRESENTATION('density',(#23386),#62946);
#23687=REPRESENTATION('material name',(#23802),#62948);
#23688=REPRESENTATION('density',(#23387),#62948);
#23689=REPRESENTATION('material name',(#23803),#62949);
#23690=REPRESENTATION('density',(#23388),#62949);
#23691=REPRESENTATION('material name',(#23804),#62950);
#23692=REPRESENTATION('density',(#23389),#62950);
#23693=REPRESENTATION('material name',(#23805),#62951);
#23694=REPRESENTATION('density',(#23390),#62951);
#23695=REPRESENTATION('material name',(#23806),#62952);
#23696=REPRESENTATION('density',(#23391),#62952);
#23697=REPRESENTATION('material name',(#23807),#62954);
#23698=REPRESENTATION('density',(#23392),#62954);
#23699=REPRESENTATION('material name',(#23808),#62955);
#23700=REPRESENTATION('density',(#23393),#62955);
#23701=REPRESENTATION('material name',(#23809),#62956);
#23702=REPRESENTATION('density',(#23394),#62956);
#23703=REPRESENTATION('material name',(#23810),#62957);
#23704=REPRESENTATION('density',(#23395),#62957);
#23705=REPRESENTATION('material name',(#23811),#62958);
#23706=REPRESENTATION('density',(#23396),#62958);
#23707=REPRESENTATION('material name',(#23812),#62959);
#23708=REPRESENTATION('density',(#23397),#62959);
#23709=REPRESENTATION('material name',(#23813),#62961);
#23710=REPRESENTATION('density',(#23398),#62961);
#23711=REPRESENTATION('material name',(#23814),#62962);
#23712=REPRESENTATION('density',(#23399),#62962);
#23713=REPRESENTATION('material name',(#23815),#62963);
#23714=REPRESENTATION('density',(#23400),#62963);
#23715=REPRESENTATION('material name',(#23816),#62965);
#23716=REPRESENTATION('density',(#23401),#62965);
#23717=REPRESENTATION('material name',(#23817),#62966);
#23718=REPRESENTATION('density',(#23402),#62966);
#23719=REPRESENTATION('material name',(#23818),#62967);
#23720=REPRESENTATION('density',(#23403),#62967);
#23721=REPRESENTATION('material name',(#23819),#62968);
#23722=REPRESENTATION('density',(#23404),#62968);
#23723=REPRESENTATION('material name',(#23820),#62969);
#23724=REPRESENTATION('density',(#23405),#62969);
#23725=REPRESENTATION('material name',(#23821),#62970);
#23726=REPRESENTATION('density',(#23406),#62970);
#23727=REPRESENTATION('material name',(#23822),#62971);
#23728=REPRESENTATION('density',(#23407),#62971);
#23729=REPRESENTATION('material name',(#23823),#62972);
#23730=REPRESENTATION('density',(#23408),#62972);
#23731=REPRESENTATION('material name',(#23824),#62974);
#23732=REPRESENTATION('density',(#23409),#62974);
#23733=REPRESENTATION('material name',(#23825),#62975);
#23734=REPRESENTATION('density',(#23410),#62975);
#23735=REPRESENTATION('material name',(#23826),#62976);
#23736=REPRESENTATION('density',(#23411),#62976);
#23737=REPRESENTATION('material name',(#23827),#62977);
#23738=REPRESENTATION('density',(#23412),#62977);
#23739=REPRESENTATION('material name',(#23828),#62978);
#23740=REPRESENTATION('density',(#23413),#62978);
#23741=REPRESENTATION('material name',(#23829),#62979);
#23742=REPRESENTATION('density',(#23414),#62979);
#23743=REPRESENTATION('material name',(#23830),#62980);
#23744=REPRESENTATION('density',(#23415),#62980);
#23745=REPRESENTATION('material name',(#23831),#62981);
#23746=REPRESENTATION('density',(#23416),#62981);
#23747=REPRESENTATION('material name',(#23832),#62982);
#23748=REPRESENTATION('density',(#23417),#62982);
#23749=REPRESENTATION('material name',(#23833),#62983);
#23750=REPRESENTATION('density',(#23418),#62983);
#23751=DESCRIPTIVE_REPRESENTATION_ITEM('Steel','Steel');
#23752=DESCRIPTIVE_REPRESENTATION_ITEM('Steel','Steel');
#23753=DESCRIPTIVE_REPRESENTATION_ITEM('Steel','Steel');
#23754=DESCRIPTIVE_REPRESENTATION_ITEM('Steel','Steel');
#23755=DESCRIPTIVE_REPRESENTATION_ITEM('Steel','Steel');
#23756=DESCRIPTIVE_REPRESENTATION_ITEM('Steel','Steel');
#23757=DESCRIPTIVE_REPRESENTATION_ITEM('Steel','Steel');
#23758=DESCRIPTIVE_REPRESENTATION_ITEM('Steel','Steel');
#23759=DESCRIPTIVE_REPRESENTATION_ITEM('Steel','Steel');
#23760=DESCRIPTIVE_REPRESENTATION_ITEM('Steel','Steel');
#23761=DESCRIPTIVE_REPRESENTATION_ITEM('Steel','Steel');
#23762=DESCRIPTIVE_REPRESENTATION_ITEM('Steel','Steel');
#23763=DESCRIPTIVE_REPRESENTATION_ITEM('Steel','Steel');
#23764=DESCRIPTIVE_REPRESENTATION_ITEM('Steel','Steel');
#23765=DESCRIPTIVE_REPRESENTATION_ITEM('Steel','Steel');
#23766=DESCRIPTIVE_REPRESENTATION_ITEM('Steel','Steel');
#23767=DESCRIPTIVE_REPRESENTATION_ITEM('Steel','Steel');
#23768=DESCRIPTIVE_REPRESENTATION_ITEM('Steel','Steel');
#23769=DESCRIPTIVE_REPRESENTATION_ITEM('Steel','Steel');
#23770=DESCRIPTIVE_REPRESENTATION_ITEM('Steel','Steel');
#23771=DESCRIPTIVE_REPRESENTATION_ITEM('Steel','Steel');
#23772=DESCRIPTIVE_REPRESENTATION_ITEM('Steel','Steel');
#23773=DESCRIPTIVE_REPRESENTATION_ITEM('Steel','Steel');
#23774=DESCRIPTIVE_REPRESENTATION_ITEM('Steel','Steel');
#23775=DESCRIPTIVE_REPRESENTATION_ITEM('Steel','Steel');
#23776=DESCRIPTIVE_REPRESENTATION_ITEM('Steel','Steel');
#23777=DESCRIPTIVE_REPRESENTATION_ITEM('Steel','Steel');
#23778=DESCRIPTIVE_REPRESENTATION_ITEM('Steel','Steel');
#23779=DESCRIPTIVE_REPRESENTATION_ITEM('Steel','Steel');
#23780=DESCRIPTIVE_REPRESENTATION_ITEM('Steel','Steel');
#23781=DESCRIPTIVE_REPRESENTATION_ITEM('Steel','Steel');
#23782=DESCRIPTIVE_REPRESENTATION_ITEM('Steel','Steel');
#23783=DESCRIPTIVE_REPRESENTATION_ITEM('Steel','Steel');
#23784=DESCRIPTIVE_REPRESENTATION_ITEM('Steel','Steel');
#23785=DESCRIPTIVE_REPRESENTATION_ITEM('Steel','Steel');
#23786=DESCRIPTIVE_REPRESENTATION_ITEM('Steel','Steel');
#23787=DESCRIPTIVE_REPRESENTATION_ITEM('Steel','Steel');
#23788=DESCRIPTIVE_REPRESENTATION_ITEM('Steel','Steel');
#23789=DESCRIPTIVE_REPRESENTATION_ITEM('Steel','Steel');
#23790=DESCRIPTIVE_REPRESENTATION_ITEM('Steel','Steel');
#23791=DESCRIPTIVE_REPRESENTATION_ITEM('Steel','Steel');
#23792=DESCRIPTIVE_REPRESENTATION_ITEM('Steel','Steel');
#23793=DESCRIPTIVE_REPRESENTATION_ITEM('Steel','Steel');
#23794=DESCRIPTIVE_REPRESENTATION_ITEM('Steel','Steel');
#23795=DESCRIPTIVE_REPRESENTATION_ITEM('Steel','Steel');
#23796=DESCRIPTIVE_REPRESENTATION_ITEM('Steel','Steel');
#23797=DESCRIPTIVE_REPRESENTATION_ITEM('Steel','Steel');
#23798=DESCRIPTIVE_REPRESENTATION_ITEM('Steel','Steel');
#23799=DESCRIPTIVE_REPRESENTATION_ITEM('Steel','Steel');
#23800=DESCRIPTIVE_REPRESENTATION_ITEM('Steel','Steel');
#23801=DESCRIPTIVE_REPRESENTATION_ITEM('Steel','Steel');
#23802=DESCRIPTIVE_REPRESENTATION_ITEM('Steel','Steel');
#23803=DESCRIPTIVE_REPRESENTATION_ITEM('Steel','Steel');
#23804=DESCRIPTIVE_REPRESENTATION_ITEM('Steel','Steel');
#23805=DESCRIPTIVE_REPRESENTATION_ITEM('Steel','Steel');
#23806=DESCRIPTIVE_REPRESENTATION_ITEM('Steel','Steel');
#23807=DESCRIPTIVE_REPRESENTATION_ITEM('Steel','Steel');
#23808=DESCRIPTIVE_REPRESENTATION_ITEM('Steel','Steel');
#23809=DESCRIPTIVE_REPRESENTATION_ITEM('Steel','Steel');
#23810=DESCRIPTIVE_REPRESENTATION_ITEM('Steel','Steel');
#23811=DESCRIPTIVE_REPRESENTATION_ITEM('Steel','Steel');
#23812=DESCRIPTIVE_REPRESENTATION_ITEM('Steel','Steel');
#23813=DESCRIPTIVE_REPRESENTATION_ITEM('Steel','Steel');
#23814=DESCRIPTIVE_REPRESENTATION_ITEM('Steel','Steel');
#23815=DESCRIPTIVE_REPRESENTATION_ITEM('Steel','Steel');
#23816=DESCRIPTIVE_REPRESENTATION_ITEM('Steel','Steel');
#23817=DESCRIPTIVE_REPRESENTATION_ITEM('Steel','Steel');
#23818=DESCRIPTIVE_REPRESENTATION_ITEM('Steel','Steel');
#23819=DESCRIPTIVE_REPRESENTATION_ITEM('Steel','Steel');
#23820=DESCRIPTIVE_REPRESENTATION_ITEM('Steel','Steel');
#23821=DESCRIPTIVE_REPRESENTATION_ITEM('Steel','Steel');
#23822=DESCRIPTIVE_REPRESENTATION_ITEM('Steel','Steel');
#23823=DESCRIPTIVE_REPRESENTATION_ITEM('Steel','Steel');
#23824=DESCRIPTIVE_REPRESENTATION_ITEM('Steel','Steel');
#23825=DESCRIPTIVE_REPRESENTATION_ITEM('Steel','Steel');
#23826=DESCRIPTIVE_REPRESENTATION_ITEM('Steel','Steel');
#23827=DESCRIPTIVE_REPRESENTATION_ITEM('Steel','Steel');
#23828=DESCRIPTIVE_REPRESENTATION_ITEM('Steel','Steel');
#23829=DESCRIPTIVE_REPRESENTATION_ITEM('Steel','Steel');
#23830=DESCRIPTIVE_REPRESENTATION_ITEM('Steel','Steel');
#23831=DESCRIPTIVE_REPRESENTATION_ITEM('Steel','Steel');
#23832=DESCRIPTIVE_REPRESENTATION_ITEM('Steel','Steel');
#23833=DESCRIPTIVE_REPRESENTATION_ITEM('Steel','Steel');
#23834=PROPERTY_DEFINITION('material property','material name',#63451);
#23835=PROPERTY_DEFINITION('material property','density of part',#63451);
#23836=PROPERTY_DEFINITION('material property','material name',#63452);
#23837=PROPERTY_DEFINITION('material property','density of part',#63452);
#23838=PROPERTY_DEFINITION('material property','material name',#63453);
#23839=PROPERTY_DEFINITION('material property','density of part',#63453);
#23840=PROPERTY_DEFINITION('material property','material name',#63454);
#23841=PROPERTY_DEFINITION('material property','density of part',#63454);
#23842=PROPERTY_DEFINITION('material property','material name',#63455);
#23843=PROPERTY_DEFINITION('material property','density of part',#63455);
#23844=PROPERTY_DEFINITION('material property','material name',#63456);
#23845=PROPERTY_DEFINITION('material property','density of part',#63456);
#23846=PROPERTY_DEFINITION('material property','material name',#63457);
#23847=PROPERTY_DEFINITION('material property','density of part',#63457);
#23848=PROPERTY_DEFINITION('material property','material name',#63458);
#23849=PROPERTY_DEFINITION('material property','density of part',#63458);
#23850=PROPERTY_DEFINITION('material property','material name',#63459);
#23851=PROPERTY_DEFINITION('material property','density of part',#63459);
#23852=PROPERTY_DEFINITION('material property','material name',#63460);
#23853=PROPERTY_DEFINITION('material property','density of part',#63460);
#23854=PROPERTY_DEFINITION('material property','material name',#63461);
#23855=PROPERTY_DEFINITION('material property','density of part',#63461);
#23856=PROPERTY_DEFINITION('material property','material name',#63463);
#23857=PROPERTY_DEFINITION('material property','density of part',#63463);
#23858=PROPERTY_DEFINITION('material property','material name',#63464);
#23859=PROPERTY_DEFINITION('material property','density of part',#63464);
#23860=PROPERTY_DEFINITION('material property','material name',#63465);
#23861=PROPERTY_DEFINITION('material property','density of part',#63465);
#23862=PROPERTY_DEFINITION('material property','material name',#63466);
#23863=PROPERTY_DEFINITION('material property','density of part',#63466);
#23864=PROPERTY_DEFINITION('material property','material name',#63467);
#23865=PROPERTY_DEFINITION('material property','density of part',#63467);
#23866=PROPERTY_DEFINITION('material property','material name',#63469);
#23867=PROPERTY_DEFINITION('material property','density of part',#63469);
#23868=PROPERTY_DEFINITION('material property','material name',#63470);
#23869=PROPERTY_DEFINITION('material property','density of part',#63470);
#23870=PROPERTY_DEFINITION('material property','material name',#63471);
#23871=PROPERTY_DEFINITION('material property','density of part',#63471);
#23872=PROPERTY_DEFINITION('material property','material name',#63472);
#23873=PROPERTY_DEFINITION('material property','density of part',#63472);
#23874=PROPERTY_DEFINITION('material property','material name',#63473);
#23875=PROPERTY_DEFINITION('material property','density of part',#63473);
#23876=PROPERTY_DEFINITION('material property','material name',#63475);
#23877=PROPERTY_DEFINITION('material property','density of part',#63475);
#23878=PROPERTY_DEFINITION('material property','material name',#63476);
#23879=PROPERTY_DEFINITION('material property','density of part',#63476);
#23880=PROPERTY_DEFINITION('material property','material name',#63477);
#23881=PROPERTY_DEFINITION('material property','density of part',#63477);
#23882=PROPERTY_DEFINITION('material property','material name',#63479);
#23883=PROPERTY_DEFINITION('material property','density of part',#63479);
#23884=PROPERTY_DEFINITION('material property','material name',#63480);
#23885=PROPERTY_DEFINITION('material property','density of part',#63480);
#23886=PROPERTY_DEFINITION('material property','material name',#63481);
#23887=PROPERTY_DEFINITION('material property','density of part',#63481);
#23888=PROPERTY_DEFINITION('material property','material name',#63482);
#23889=PROPERTY_DEFINITION('material property','density of part',#63482);
#23890=PROPERTY_DEFINITION('material property','material name',#63483);
#23891=PROPERTY_DEFINITION('material property','density of part',#63483);
#23892=PROPERTY_DEFINITION('material property','material name',#63484);
#23893=PROPERTY_DEFINITION('material property','density of part',#63484);
#23894=PROPERTY_DEFINITION('material property','material name',#63485);
#23895=PROPERTY_DEFINITION('material property','density of part',#63485);
#23896=PROPERTY_DEFINITION('material property','material name',#63486);
#23897=PROPERTY_DEFINITION('material property','density of part',#63486);
#23898=PROPERTY_DEFINITION('material property','material name',#63488);
#23899=PROPERTY_DEFINITION('material property','density of part',#63488);
#23900=PROPERTY_DEFINITION('material property','material name',#63489);
#23901=PROPERTY_DEFINITION('material property','density of part',#63489);
#23902=PROPERTY_DEFINITION('material property','material name',#63490);
#23903=PROPERTY_DEFINITION('material property','density of part',#63490);
#23904=PROPERTY_DEFINITION('material property','material name',#63491);
#23905=PROPERTY_DEFINITION('material property','density of part',#63491);
#23906=PROPERTY_DEFINITION('material property','material name',#63492);
#23907=PROPERTY_DEFINITION('material property','density of part',#63492);
#23908=PROPERTY_DEFINITION('material property','material name',#63493);
#23909=PROPERTY_DEFINITION('material property','density of part',#63493);
#23910=PROPERTY_DEFINITION('material property','material name',#63494);
#23911=PROPERTY_DEFINITION('material property','density of part',#63494);
#23912=PROPERTY_DEFINITION('material property','material name',#63495);
#23913=PROPERTY_DEFINITION('material property','density of part',#63495);
#23914=PROPERTY_DEFINITION('material property','material name',#63496);
#23915=PROPERTY_DEFINITION('material property','density of part',#63496);
#23916=PROPERTY_DEFINITION('material property','material name',#63497);
#23917=PROPERTY_DEFINITION('material property','density of part',#63497);
#23918=PROPERTY_DEFINITION('material property','material name',#63500);
#23919=PROPERTY_DEFINITION('material property','density of part',#63500);
#23920=PROPERTY_DEFINITION('material property','material name',#63501);
#23921=PROPERTY_DEFINITION('material property','density of part',#63501);
#23922=PROPERTY_DEFINITION('material property','material name',#63502);
#23923=PROPERTY_DEFINITION('material property','density of part',#63502);
#23924=PROPERTY_DEFINITION('material property','material name',#63503);
#23925=PROPERTY_DEFINITION('material property','density of part',#63503);
#23926=PROPERTY_DEFINITION('material property','material name',#63504);
#23927=PROPERTY_DEFINITION('material property','density of part',#63504);
#23928=PROPERTY_DEFINITION('material property','material name',#63505);
#23929=PROPERTY_DEFINITION('material property','density of part',#63505);
#23930=PROPERTY_DEFINITION('material property','material name',#63506);
#23931=PROPERTY_DEFINITION('material property','density of part',#63506);
#23932=PROPERTY_DEFINITION('material property','material name',#63507);
#23933=PROPERTY_DEFINITION('material property','density of part',#63507);
#23934=PROPERTY_DEFINITION('material property','material name',#63508);
#23935=PROPERTY_DEFINITION('material property','density of part',#63508);
#23936=PROPERTY_DEFINITION('material property','material name',#63510);
#23937=PROPERTY_DEFINITION('material property','density of part',#63510);
#23938=PROPERTY_DEFINITION('material property','material name',#63511);
#23939=PROPERTY_DEFINITION('material property','density of part',#63511);
#23940=PROPERTY_DEFINITION('material property','material name',#63512);
#23941=PROPERTY_DEFINITION('material property','density of part',#63512);
#23942=PROPERTY_DEFINITION('material property','material name',#63513);
#23943=PROPERTY_DEFINITION('material property','density of part',#63513);
#23944=PROPERTY_DEFINITION('material property','material name',#63514);
#23945=PROPERTY_DEFINITION('material property','density of part',#63514);
#23946=PROPERTY_DEFINITION('material property','material name',#63516);
#23947=PROPERTY_DEFINITION('material property','density of part',#63516);
#23948=PROPERTY_DEFINITION('material property','material name',#63517);
#23949=PROPERTY_DEFINITION('material property','density of part',#63517);
#23950=PROPERTY_DEFINITION('material property','material name',#63518);
#23951=PROPERTY_DEFINITION('material property','density of part',#63518);
#23952=PROPERTY_DEFINITION('material property','material name',#63519);
#23953=PROPERTY_DEFINITION('material property','density of part',#63519);
#23954=PROPERTY_DEFINITION('material property','material name',#63520);
#23955=PROPERTY_DEFINITION('material property','density of part',#63520);
#23956=PROPERTY_DEFINITION('material property','material name',#63521);
#23957=PROPERTY_DEFINITION('material property','density of part',#63521);
#23958=PROPERTY_DEFINITION('material property','material name',#63523);
#23959=PROPERTY_DEFINITION('material property','density of part',#63523);
#23960=PROPERTY_DEFINITION('material property','material name',#63524);
#23961=PROPERTY_DEFINITION('material property','density of part',#63524);
#23962=PROPERTY_DEFINITION('material property','material name',#63525);
#23963=PROPERTY_DEFINITION('material property','density of part',#63525);
#23964=PROPERTY_DEFINITION('material property','material name',#63527);
#23965=PROPERTY_DEFINITION('material property','density of part',#63527);
#23966=PROPERTY_DEFINITION('material property','material name',#63528);
#23967=PROPERTY_DEFINITION('material property','density of part',#63528);
#23968=PROPERTY_DEFINITION('material property','material name',#63529);
#23969=PROPERTY_DEFINITION('material property','density of part',#63529);
#23970=PROPERTY_DEFINITION('material property','material name',#63530);
#23971=PROPERTY_DEFINITION('material property','density of part',#63530);
#23972=PROPERTY_DEFINITION('material property','material name',#63531);
#23973=PROPERTY_DEFINITION('material property','density of part',#63531);
#23974=PROPERTY_DEFINITION('material property','material name',#63532);
#23975=PROPERTY_DEFINITION('material property','density of part',#63532);
#23976=PROPERTY_DEFINITION('material property','material name',#63533);
#23977=PROPERTY_DEFINITION('material property','density of part',#63533);
#23978=PROPERTY_DEFINITION('material property','material name',#63534);
#23979=PROPERTY_DEFINITION('material property','density of part',#63534);
#23980=PROPERTY_DEFINITION('material property','material name',#63536);
#23981=PROPERTY_DEFINITION('material property','density of part',#63536);
#23982=PROPERTY_DEFINITION('material property','material name',#63537);
#23983=PROPERTY_DEFINITION('material property','density of part',#63537);
#23984=PROPERTY_DEFINITION('material property','material name',#63538);
#23985=PROPERTY_DEFINITION('material property','density of part',#63538);
#23986=PROPERTY_DEFINITION('material property','material name',#63539);
#23987=PROPERTY_DEFINITION('material property','density of part',#63539);
#23988=PROPERTY_DEFINITION('material property','material name',#63540);
#23989=PROPERTY_DEFINITION('material property','density of part',#63540);
#23990=PROPERTY_DEFINITION('material property','material name',#63541);
#23991=PROPERTY_DEFINITION('material property','density of part',#63541);
#23992=PROPERTY_DEFINITION('material property','material name',#63542);
#23993=PROPERTY_DEFINITION('material property','density of part',#63542);
#23994=PROPERTY_DEFINITION('material property','material name',#63543);
#23995=PROPERTY_DEFINITION('material property','density of part',#63543);
#23996=PROPERTY_DEFINITION('material property','material name',#63544);
#23997=PROPERTY_DEFINITION('material property','density of part',#63544);
#23998=PROPERTY_DEFINITION('material property','material name',#63545);
#23999=PROPERTY_DEFINITION('material property','density of part',#63545);
#24000=AXIS2_PLACEMENT_3D('',#32870,#26461,#26462);
#24001=AXIS2_PLACEMENT_3D('',#32871,#26463,#26464);
#24002=AXIS2_PLACEMENT_3D('',#32872,#26465,#26466);
#24003=AXIS2_PLACEMENT_3D('',#32873,#26467,#26468);
#24004=AXIS2_PLACEMENT_3D('',#32874,#26469,#26470);
#24005=AXIS2_PLACEMENT_3D('',#32876,#26471,#26472);
#24006=AXIS2_PLACEMENT_3D('',#32879,#26474,#26475);
#24007=AXIS2_PLACEMENT_3D('',#32880,#26476,#26477);
#24008=AXIS2_PLACEMENT_3D('',#32882,#26478,#26479);
#24009=AXIS2_PLACEMENT_3D('',#32885,#26481,#26482);
#24010=AXIS2_PLACEMENT_3D('',#32886,#26483,#26484);
#24011=AXIS2_PLACEMENT_3D('',#32888,#26485,#26486);
#24012=AXIS2_PLACEMENT_3D('',#32891,#26488,#26489);
#24013=AXIS2_PLACEMENT_3D('',#32892,#26490,#26491);
#24014=AXIS2_PLACEMENT_3D('',#32894,#26492,#26493);
#24015=AXIS2_PLACEMENT_3D('',#32897,#26495,#26496);
#24016=AXIS2_PLACEMENT_3D('',#32898,#26497,#26498);
#24017=AXIS2_PLACEMENT_3D('',#32900,#26499,#26500);
#24018=AXIS2_PLACEMENT_3D('',#32903,#26502,#26503);
#24019=AXIS2_PLACEMENT_3D('',#32904,#26504,#26505);
#24020=AXIS2_PLACEMENT_3D('',#32906,#26506,#26507);
#24021=AXIS2_PLACEMENT_3D('',#32909,#26509,#26510);
#24022=AXIS2_PLACEMENT_3D('',#32910,#26511,#26512);
#24023=AXIS2_PLACEMENT_3D('',#32912,#26513,#26514);
#24024=AXIS2_PLACEMENT_3D('',#32915,#26516,#26517);
#24025=AXIS2_PLACEMENT_3D('',#32916,#26518,#26519);
#24026=AXIS2_PLACEMENT_3D('',#32918,#26520,#26521);
#24027=AXIS2_PLACEMENT_3D('',#32921,#26523,#26524);
#24028=AXIS2_PLACEMENT_3D('',#32922,#26525,#26526);
#24029=AXIS2_PLACEMENT_3D('',#32924,#26527,#26528);
#24030=AXIS2_PLACEMENT_3D('',#32927,#26530,#26531);
#24031=AXIS2_PLACEMENT_3D('',#32928,#26532,#26533);
#24032=AXIS2_PLACEMENT_3D('',#32930,#26534,#26535);
#24033=AXIS2_PLACEMENT_3D('',#32933,#26537,#26538);
#24034=AXIS2_PLACEMENT_3D('',#32934,#26539,#26540);
#24035=AXIS2_PLACEMENT_3D('',#32943,#26545,#26546);
#24036=AXIS2_PLACEMENT_3D('',#32949,#26550,#26551);
#24037=AXIS2_PLACEMENT_3D('',#32955,#26555,#26556);
#24038=AXIS2_PLACEMENT_3D('',#32958,#26559,#26560);
#24039=AXIS2_PLACEMENT_3D('',#32959,#26561,#26562);
#24040=AXIS2_PLACEMENT_3D('',#32960,#26563,#26564);
#24041=AXIS2_PLACEMENT_3D('',#32961,#26565,#26566);
#24042=AXIS2_PLACEMENT_3D('',#32970,#26571,#26572);
#24043=AXIS2_PLACEMENT_3D('',#32976,#26576,#26577);
#24044=AXIS2_PLACEMENT_3D('',#32982,#26581,#26582);
#24045=AXIS2_PLACEMENT_3D('',#32985,#26585,#26586);
#24046=AXIS2_PLACEMENT_3D('',#32986,#26587,#26588);
#24047=AXIS2_PLACEMENT_3D('',#32987,#26589,#26590);
#24048=AXIS2_PLACEMENT_3D('',#32988,#26591,#26592);
#24049=AXIS2_PLACEMENT_3D('',#32997,#26597,#26598);
#24050=AXIS2_PLACEMENT_3D('',#33003,#26602,#26603);
#24051=AXIS2_PLACEMENT_3D('',#33009,#26607,#26608);
#24052=AXIS2_PLACEMENT_3D('',#33012,#26611,#26612);
#24053=AXIS2_PLACEMENT_3D('',#33013,#26613,#26614);
#24054=AXIS2_PLACEMENT_3D('',#33014,#26615,#26616);
#24055=AXIS2_PLACEMENT_3D('',#33015,#26617,#26618);
#24056=AXIS2_PLACEMENT_3D('',#33020,#26620,#26621);
#24057=AXIS2_PLACEMENT_3D('',#33023,#26623,#26624);
#24058=AXIS2_PLACEMENT_3D('',#33024,#26625,#26626);
#24059=AXIS2_PLACEMENT_3D('',#33029,#26628,#26629);
#24060=AXIS2_PLACEMENT_3D('',#33032,#26631,#26632);
#24061=AXIS2_PLACEMENT_3D('',#33033,#26633,#26634);
#24062=AXIS2_PLACEMENT_3D('',#33035,#26635,#26636);
#24063=AXIS2_PLACEMENT_3D('',#33038,#26638,#26639);
#24064=AXIS2_PLACEMENT_3D('',#33039,#26640,#26641);
#24065=AXIS2_PLACEMENT_3D('',#33041,#26642,#26643);
#24066=AXIS2_PLACEMENT_3D('',#33044,#26645,#26646);
#24067=AXIS2_PLACEMENT_3D('',#33045,#26647,#26648);
#24068=AXIS2_PLACEMENT_3D('',#33047,#26649,#26650);
#24069=AXIS2_PLACEMENT_3D('',#33050,#26652,#26653);
#24070=AXIS2_PLACEMENT_3D('',#33051,#26654,#26655);
#24071=AXIS2_PLACEMENT_3D('',#33053,#26656,#26657);
#24072=AXIS2_PLACEMENT_3D('',#33056,#26659,#26660);
#24073=AXIS2_PLACEMENT_3D('',#33057,#26661,#26662);
#24074=AXIS2_PLACEMENT_3D('',#33059,#26663,#26664);
#24075=AXIS2_PLACEMENT_3D('',#33062,#26666,#26667);
#24076=AXIS2_PLACEMENT_3D('',#33063,#26668,#26669);
#24077=AXIS2_PLACEMENT_3D('',#33065,#26670,#26671);
#24078=AXIS2_PLACEMENT_3D('',#33066,#26672,#26673);
#24079=AXIS2_PLACEMENT_3D('',#33067,#26674,#26675);
#24080=AXIS2_PLACEMENT_3D('',#33069,#26677,#26678);
#24081=AXIS2_PLACEMENT_3D('',#33070,#26679,#26680);
#24082=AXIS2_PLACEMENT_3D('',#33072,#26681,#26682);
#24083=AXIS2_PLACEMENT_3D('',#33073,#26683,#26684);
#24084=AXIS2_PLACEMENT_3D('',#33075,#26685,#26686);
#24085=AXIS2_PLACEMENT_3D('',#33078,#26688,#26689);
#24086=AXIS2_PLACEMENT_3D('',#33079,#26690,#26691);
#24087=AXIS2_PLACEMENT_3D('',#33081,#26692,#26693);
#24088=AXIS2_PLACEMENT_3D('',#33082,#26694,#26695);
#24089=AXIS2_PLACEMENT_3D('',#33083,#26696,#26697);
#24090=AXIS2_PLACEMENT_3D('',#33085,#26699,#26700);
#24091=AXIS2_PLACEMENT_3D('',#33086,#26701,#26702);
#24092=AXIS2_PLACEMENT_3D('',#33088,#26703,#26704);
#24093=AXIS2_PLACEMENT_3D('',#33089,#26705,#26706);
#24094=AXIS2_PLACEMENT_3D('',#33100,#26713,#26714);
#24095=AXIS2_PLACEMENT_3D('',#33102,#26715,#26716);
#24096=AXIS2_PLACEMENT_3D('',#33104,#26718,#26719);
#24097=AXIS2_PLACEMENT_3D('',#33106,#26720,#26721);
#24098=AXIS2_PLACEMENT_3D('',#33108,#26723,#26724);
#24099=AXIS2_PLACEMENT_3D('',#33110,#26725,#26726);
#24100=AXIS2_PLACEMENT_3D('',#33112,#26728,#26729);
#24101=AXIS2_PLACEMENT_3D('',#33114,#26730,#26731);
#24102=AXIS2_PLACEMENT_3D('',#33116,#26733,#26734);
#24103=AXIS2_PLACEMENT_3D('',#33122,#26738,#26739);
#24104=AXIS2_PLACEMENT_3D('',#33126,#26742,#26743);
#24105=AXIS2_PLACEMENT_3D('',#33130,#26746,#26747);
#24106=AXIS2_PLACEMENT_3D('',#33132,#26749,#26750);
#24107=AXIS2_PLACEMENT_3D('',#33133,#26751,#26752);
#24108=AXIS2_PLACEMENT_3D('',#33134,#26753,#26754);
#24109=AXIS2_PLACEMENT_3D('',#33136,#26755,#26756);
#24110=AXIS2_PLACEMENT_3D('',#33139,#26758,#26759);
#24111=AXIS2_PLACEMENT_3D('',#33140,#26760,#26761);
#24112=AXIS2_PLACEMENT_3D('',#33142,#26762,#26763);
#24113=AXIS2_PLACEMENT_3D('',#33145,#26765,#26766);
#24114=AXIS2_PLACEMENT_3D('',#33146,#26767,#26768);
#24115=AXIS2_PLACEMENT_3D('',#33148,#26769,#26770);
#24116=AXIS2_PLACEMENT_3D('',#33151,#26772,#26773);
#24117=AXIS2_PLACEMENT_3D('',#33152,#26774,#26775);
#24118=AXIS2_PLACEMENT_3D('',#33154,#26776,#26777);
#24119=AXIS2_PLACEMENT_3D('',#33157,#26779,#26780);
#24120=AXIS2_PLACEMENT_3D('',#33158,#26781,#26782);
#24121=AXIS2_PLACEMENT_3D('',#33160,#26783,#26784);
#24122=AXIS2_PLACEMENT_3D('',#33161,#26785,#26786);
#24123=AXIS2_PLACEMENT_3D('',#33164,#26788,#26789);
#24124=AXIS2_PLACEMENT_3D('',#33165,#26790,#26791);
#24125=AXIS2_PLACEMENT_3D('',#33167,#26792,#26793);
#24126=AXIS2_PLACEMENT_3D('',#33170,#26795,#26796);
#24127=AXIS2_PLACEMENT_3D('',#33171,#26797,#26798);
#24128=AXIS2_PLACEMENT_3D('',#33172,#26799,#26800);
#24129=AXIS2_PLACEMENT_3D('',#33174,#26801,#26802);
#24130=AXIS2_PLACEMENT_3D('',#33177,#26804,#26805);
#24131=AXIS2_PLACEMENT_3D('',#33178,#26806,#26807);
#24132=AXIS2_PLACEMENT_3D('',#33179,#26808,#26809);
#24133=AXIS2_PLACEMENT_3D('',#33188,#26814,#26815);
#24134=AXIS2_PLACEMENT_3D('',#33194,#26819,#26820);
#24135=AXIS2_PLACEMENT_3D('',#33200,#26824,#26825);
#24136=AXIS2_PLACEMENT_3D('',#33203,#26828,#26829);
#24137=AXIS2_PLACEMENT_3D('',#33204,#26830,#26831);
#24138=AXIS2_PLACEMENT_3D('',#33205,#26832,#26833);
#24139=AXIS2_PLACEMENT_3D('',#33206,#26834,#26835);
#24140=AXIS2_PLACEMENT_3D('',#33208,#26836,#26837);
#24141=AXIS2_PLACEMENT_3D('',#33211,#26839,#26840);
#24142=AXIS2_PLACEMENT_3D('',#33212,#26841,#26842);
#24143=AXIS2_PLACEMENT_3D('',#33214,#26843,#26844);
#24144=AXIS2_PLACEMENT_3D('',#33217,#26846,#26847);
#24145=AXIS2_PLACEMENT_3D('',#33218,#26848,#26849);
#24146=AXIS2_PLACEMENT_3D('',#33220,#26850,#26851);
#24147=AXIS2_PLACEMENT_3D('',#33223,#26853,#26854);
#24148=AXIS2_PLACEMENT_3D('',#33224,#26855,#26856);
#24149=AXIS2_PLACEMENT_3D('',#33226,#26857,#26858);
#24150=AXIS2_PLACEMENT_3D('',#33229,#26860,#26861);
#24151=AXIS2_PLACEMENT_3D('',#33230,#26862,#26863);
#24152=AXIS2_PLACEMENT_3D('',#33232,#26864,#26865);
#24153=AXIS2_PLACEMENT_3D('',#33233,#26866,#26867);
#24154=AXIS2_PLACEMENT_3D('',#33236,#26869,#26870);
#24155=AXIS2_PLACEMENT_3D('',#33237,#26871,#26872);
#24156=AXIS2_PLACEMENT_3D('',#33239,#26873,#26874);
#24157=AXIS2_PLACEMENT_3D('',#33242,#26876,#26877);
#24158=AXIS2_PLACEMENT_3D('',#33243,#26878,#26879);
#24159=AXIS2_PLACEMENT_3D('',#33244,#26880,#26881);
#24160=AXIS2_PLACEMENT_3D('',#33245,#26882,#26883);
#24161=AXIS2_PLACEMENT_3D('',#33246,#26884,#26885);
#24162=AXIS2_PLACEMENT_3D('',#33248,#26886,#26887);
#24163=AXIS2_PLACEMENT_3D('',#33251,#26889,#26890);
#24164=AXIS2_PLACEMENT_3D('',#33252,#26891,#26892);
#24165=AXIS2_PLACEMENT_3D('',#33254,#26893,#26894);
#24166=AXIS2_PLACEMENT_3D('',#33257,#26896,#26897);
#24167=AXIS2_PLACEMENT_3D('',#33258,#26898,#26899);
#24168=AXIS2_PLACEMENT_3D('',#33260,#26900,#26901);
#24169=AXIS2_PLACEMENT_3D('',#33263,#26903,#26904);
#24170=AXIS2_PLACEMENT_3D('',#33264,#26905,#26906);
#24171=AXIS2_PLACEMENT_3D('',#33266,#26907,#26908);
#24172=AXIS2_PLACEMENT_3D('',#33269,#26910,#26911);
#24173=AXIS2_PLACEMENT_3D('',#33270,#26912,#26913);
#24174=AXIS2_PLACEMENT_3D('',#33272,#26914,#26915);
#24175=AXIS2_PLACEMENT_3D('',#33273,#26916,#26917);
#24176=AXIS2_PLACEMENT_3D('',#33275,#26918,#26919);
#24177=AXIS2_PLACEMENT_3D('',#33277,#26921,#26922);
#24178=AXIS2_PLACEMENT_3D('',#33279,#26923,#26924);
#24179=AXIS2_PLACEMENT_3D('',#33282,#26926,#26927);
#24180=AXIS2_PLACEMENT_3D('',#33283,#26928,#26929);
#24181=AXIS2_PLACEMENT_3D('',#33284,#26930,#26931);
#24182=AXIS2_PLACEMENT_3D('',#33286,#26932,#26933);
#24183=AXIS2_PLACEMENT_3D('',#33289,#26935,#26936);
#24184=AXIS2_PLACEMENT_3D('',#33290,#26937,#26938);
#24185=AXIS2_PLACEMENT_3D('',#33291,#26939,#26940);
#24186=AXIS2_PLACEMENT_3D('',#33300,#26945,#26946);
#24187=AXIS2_PLACEMENT_3D('',#33306,#26950,#26951);
#24188=AXIS2_PLACEMENT_3D('',#33312,#26955,#26956);
#24189=AXIS2_PLACEMENT_3D('',#33315,#26959,#26960);
#24190=AXIS2_PLACEMENT_3D('',#33316,#26961,#26962);
#24191=AXIS2_PLACEMENT_3D('',#33317,#26963,#26964);
#24192=AXIS2_PLACEMENT_3D('',#33318,#26965,#26966);
#24193=AXIS2_PLACEMENT_3D('',#33320,#26967,#26968);
#24194=AXIS2_PLACEMENT_3D('',#33323,#26970,#26971);
#24195=AXIS2_PLACEMENT_3D('',#33324,#26972,#26973);
#24196=AXIS2_PLACEMENT_3D('',#33326,#26974,#26975);
#24197=AXIS2_PLACEMENT_3D('',#33329,#26977,#26978);
#24198=AXIS2_PLACEMENT_3D('',#33330,#26979,#26980);
#24199=AXIS2_PLACEMENT_3D('',#33332,#26981,#26982);
#24200=AXIS2_PLACEMENT_3D('',#33335,#26984,#26985);
#24201=AXIS2_PLACEMENT_3D('',#33336,#26986,#26987);
#24202=AXIS2_PLACEMENT_3D('',#33345,#26992,#26993);
#24203=AXIS2_PLACEMENT_3D('',#33346,#26994,#26995);
#24204=AXIS2_PLACEMENT_3D('',#33348,#26996,#26997);
#24205=AXIS2_PLACEMENT_3D('',#33349,#26998,#26999);
#24206=AXIS2_PLACEMENT_3D('',#33350,#27000,#27001);
#24207=AXIS2_PLACEMENT_3D('',#33351,#27002,#27003);
#24208=AXIS2_PLACEMENT_3D('',#33354,#27005,#27006);
#24209=AXIS2_PLACEMENT_3D('',#33355,#27007,#27008);
#24210=AXIS2_PLACEMENT_3D('',#33357,#27009,#27010);
#24211=AXIS2_PLACEMENT_3D('',#33358,#27011,#27012);
#24212=AXIS2_PLACEMENT_3D('',#33360,#27013,#27014);
#24213=AXIS2_PLACEMENT_3D('',#33362,#27016,#27017);
#24214=AXIS2_PLACEMENT_3D('',#33363,#27018,#27019);
#24215=AXIS2_PLACEMENT_3D('',#33364,#27020,#27021);
#24216=AXIS2_PLACEMENT_3D('',#33366,#27022,#27023);
#24217=AXIS2_PLACEMENT_3D('',#33369,#27025,#27026);
#24218=AXIS2_PLACEMENT_3D('',#33370,#27027,#27028);
#24219=AXIS2_PLACEMENT_3D('',#33372,#27029,#27030);
#24220=AXIS2_PLACEMENT_3D('',#33373,#27031,#27032);
#24221=AXIS2_PLACEMENT_3D('',#33375,#27033,#27034);
#24222=AXIS2_PLACEMENT_3D('',#33377,#27036,#27037);
#24223=AXIS2_PLACEMENT_3D('',#33386,#27042,#27043);
#24224=AXIS2_PLACEMENT_3D('',#33392,#27047,#27048);
#24225=AXIS2_PLACEMENT_3D('',#33398,#27052,#27053);
#24226=AXIS2_PLACEMENT_3D('',#33401,#27056,#27057);
#24227=AXIS2_PLACEMENT_3D('',#33402,#27058,#27059);
#24228=AXIS2_PLACEMENT_3D('',#33403,#27060,#27061);
#24229=AXIS2_PLACEMENT_3D('',#33404,#27062,#27063);
#24230=AXIS2_PLACEMENT_3D('',#33406,#27064,#27065);
#24231=AXIS2_PLACEMENT_3D('',#33409,#27067,#27068);
#24232=AXIS2_PLACEMENT_3D('',#33410,#27069,#27070);
#24233=AXIS2_PLACEMENT_3D('',#33412,#27071,#27072);
#24234=AXIS2_PLACEMENT_3D('',#33413,#27073,#27074);
#24235=AXIS2_PLACEMENT_3D('',#33415,#27075,#27076);
#24236=AXIS2_PLACEMENT_3D('',#33417,#27078,#27079);
#24237=AXIS2_PLACEMENT_3D('',#33426,#27084,#27085);
#24238=AXIS2_PLACEMENT_3D('',#33432,#27089,#27090);
#24239=AXIS2_PLACEMENT_3D('',#33438,#27094,#27095);
#24240=AXIS2_PLACEMENT_3D('',#33441,#27098,#27099);
#24241=AXIS2_PLACEMENT_3D('',#33442,#27100,#27101);
#24242=AXIS2_PLACEMENT_3D('',#33443,#27102,#27103);
#24243=AXIS2_PLACEMENT_3D('',#33444,#27104,#27105);
#24244=AXIS2_PLACEMENT_3D('',#33446,#27106,#27107);
#24245=AXIS2_PLACEMENT_3D('',#33449,#27109,#27110);
#24246=AXIS2_PLACEMENT_3D('',#33450,#27111,#27112);
#24247=AXIS2_PLACEMENT_3D('',#33452,#27113,#27114);
#24248=AXIS2_PLACEMENT_3D('',#33453,#27115,#27116);
#24249=AXIS2_PLACEMENT_3D('',#33455,#27117,#27118);
#24250=AXIS2_PLACEMENT_3D('',#33458,#27120,#27121);
#24251=AXIS2_PLACEMENT_3D('',#33459,#27122,#27123);
#24252=AXIS2_PLACEMENT_3D('',#33461,#27124,#27125);
#24253=AXIS2_PLACEMENT_3D('',#33462,#27126,#27127);
#24254=AXIS2_PLACEMENT_3D('',#33464,#27128,#27129);
#24255=AXIS2_PLACEMENT_3D('',#33467,#27131,#27132);
#24256=AXIS2_PLACEMENT_3D('',#33468,#27133,#27134);
#24257=AXIS2_PLACEMENT_3D('',#33470,#27135,#27136);
#24258=AXIS2_PLACEMENT_3D('',#33471,#27137,#27138);
#24259=AXIS2_PLACEMENT_3D('',#33473,#27139,#27140);
#24260=AXIS2_PLACEMENT_3D('',#33476,#27142,#27143);
#24261=AXIS2_PLACEMENT_3D('',#33477,#27144,#27145);
#24262=AXIS2_PLACEMENT_3D('',#33479,#27146,#27147);
#24263=AXIS2_PLACEMENT_3D('',#33480,#27148,#27149);
#24264=AXIS2_PLACEMENT_3D('',#33482,#27150,#27151);
#24265=AXIS2_PLACEMENT_3D('',#33484,#27153,#27154);
#24266=AXIS2_PLACEMENT_3D('',#33486,#27155,#27156);
#24267=AXIS2_PLACEMENT_3D('',#33488,#27158,#27159);
#24268=AXIS2_PLACEMENT_3D('',#33490,#27160,#27161);
#24269=AXIS2_PLACEMENT_3D('',#33492,#27163,#27164);
#24270=AXIS2_PLACEMENT_3D('',#33494,#27165,#27166);
#24271=AXIS2_PLACEMENT_3D('',#33496,#27168,#27169);
#24272=AXIS2_PLACEMENT_3D('',#33505,#27174,#27175);
#24273=AXIS2_PLACEMENT_3D('',#33511,#27179,#27180);
#24274=AXIS2_PLACEMENT_3D('',#33517,#27184,#27185);
#24275=AXIS2_PLACEMENT_3D('',#33523,#27189,#27190);
#24276=AXIS2_PLACEMENT_3D('',#33529,#27194,#27195);
#24277=AXIS2_PLACEMENT_3D('',#33535,#27199,#27200);
#24278=AXIS2_PLACEMENT_3D('',#33541,#27204,#27205);
#24279=AXIS2_PLACEMENT_3D('',#33547,#27209,#27210);
#24280=AXIS2_PLACEMENT_3D('',#33553,#27214,#27215);
#24281=AXIS2_PLACEMENT_3D('',#33559,#27219,#27220);
#24282=AXIS2_PLACEMENT_3D('',#33565,#27224,#27225);
#24283=AXIS2_PLACEMENT_3D('',#33568,#27228,#27229);
#24284=AXIS2_PLACEMENT_3D('',#33569,#27230,#27231);
#24285=AXIS2_PLACEMENT_3D('',#33570,#27232,#27233);
#24286=AXIS2_PLACEMENT_3D('',#33571,#27234,#27235);
#24287=AXIS2_PLACEMENT_3D('',#33572,#27236,#27237);
#24288=AXIS2_PLACEMENT_3D('',#33575,#27238,#27239);
#24289=AXIS2_PLACEMENT_3D('',#33576,#27240,#27241);
#24290=AXIS2_PLACEMENT_3D('',#33578,#27242,#27243);
#24291=AXIS2_PLACEMENT_3D('',#33580,#27244,#27245);
#24292=AXIS2_PLACEMENT_3D('',#33581,#27246,#27247);
#24293=AXIS2_PLACEMENT_3D('',#33582,#27248,#27249);
#24294=AXIS2_PLACEMENT_3D('',#33585,#27251,#27252);
#24295=AXIS2_PLACEMENT_3D('',#33586,#27253,#27254);
#24296=AXIS2_PLACEMENT_3D('',#33588,#27255,#27256);
#24297=AXIS2_PLACEMENT_3D('',#33591,#27258,#27259);
#24298=AXIS2_PLACEMENT_3D('',#33592,#27260,#27261);
#24299=AXIS2_PLACEMENT_3D('',#33595,#27263,#27264);
#24300=AXIS2_PLACEMENT_3D('',#33596,#27265,#27266);
#24301=AXIS2_PLACEMENT_3D('',#33597,#27267,#27268);
#24302=AXIS2_PLACEMENT_3D('',#33599,#27269,#27270);
#24303=AXIS2_PLACEMENT_3D('',#33601,#27272,#27273);
#24304=AXIS2_PLACEMENT_3D('',#33603,#27274,#27275);
#24305=AXIS2_PLACEMENT_3D('',#33604,#27276,#27277);
#24306=AXIS2_PLACEMENT_3D('',#33606,#27279,#27280);
#24307=AXIS2_PLACEMENT_3D('',#33607,#27281,#27282);
#24308=AXIS2_PLACEMENT_3D('',#33610,#27283,#27284);
#24309=AXIS2_PLACEMENT_3D('',#33611,#27285,#27286);
#24310=AXIS2_PLACEMENT_3D('',#33613,#27287,#27288);
#24311=AXIS2_PLACEMENT_3D('',#33615,#27289,#27290);
#24312=AXIS2_PLACEMENT_3D('',#33616,#27291,#27292);
#24313=AXIS2_PLACEMENT_3D('',#33617,#27293,#27294);
#24314=AXIS2_PLACEMENT_3D('',#33619,#27295,#27296);
#24315=AXIS2_PLACEMENT_3D('',#33621,#27298,#27299);
#24316=AXIS2_PLACEMENT_3D('',#33623,#27300,#27301);
#24317=AXIS2_PLACEMENT_3D('',#33625,#27302,#27303);
#24318=AXIS2_PLACEMENT_3D('',#33626,#27304,#27305);
#24319=AXIS2_PLACEMENT_3D('',#33628,#27306,#27307);
#24320=AXIS2_PLACEMENT_3D('',#33630,#27309,#27310);
#24321=AXIS2_PLACEMENT_3D('',#33632,#27311,#27312);
#24322=AXIS2_PLACEMENT_3D('',#33634,#27314,#27315);
#24323=AXIS2_PLACEMENT_3D('',#33636,#27316,#27317);
#24324=AXIS2_PLACEMENT_3D('',#33638,#27319,#27320);
#24325=AXIS2_PLACEMENT_3D('',#33639,#27321,#27322);
#24326=AXIS2_PLACEMENT_3D('',#33641,#27324,#27325);
#24327=AXIS2_PLACEMENT_3D('',#33642,#27326,#27327);
#24328=AXIS2_PLACEMENT_3D('',#33645,#27328,#27329);
#24329=AXIS2_PLACEMENT_3D('',#33646,#27330,#27331);
#24330=AXIS2_PLACEMENT_3D('',#33649,#27332,#27333);
#24331=AXIS2_PLACEMENT_3D('',#33650,#27334,#27335);
#24332=AXIS2_PLACEMENT_3D('',#33653,#27336,#27337);
#24333=AXIS2_PLACEMENT_3D('',#33654,#27338,#27339);
#24334=AXIS2_PLACEMENT_3D('',#33657,#27340,#27341);
#24335=AXIS2_PLACEMENT_3D('',#33658,#27342,#27343);
#24336=AXIS2_PLACEMENT_3D('',#33661,#27344,#27345);
#24337=AXIS2_PLACEMENT_3D('',#33662,#27346,#27347);
#24338=AXIS2_PLACEMENT_3D('',#33665,#27348,#27349);
#24339=AXIS2_PLACEMENT_3D('',#33666,#27350,#27351);
#24340=AXIS2_PLACEMENT_3D('',#33669,#27352,#27353);
#24341=AXIS2_PLACEMENT_3D('',#33670,#27354,#27355);
#24342=AXIS2_PLACEMENT_3D('',#33671,#27356,#27357);
#24343=AXIS2_PLACEMENT_3D('',#33697,#27358,#27359);
#24344=AXIS2_PLACEMENT_3D('',#33721,#27360,#27361);
#24345=AXIS2_PLACEMENT_3D('',#33722,#27362,#27363);
#24346=AXIS2_PLACEMENT_3D('',#33724,#27364,#27365);
#24347=AXIS2_PLACEMENT_3D('',#33749,#27366,#27367);
#24348=AXIS2_PLACEMENT_3D('',#33774,#27368,#27369);
#24349=AXIS2_PLACEMENT_3D('',#33777,#27371,#27372);
#24350=AXIS2_PLACEMENT_3D('',#33779,#27373,#27374);
#24351=AXIS2_PLACEMENT_3D('',#33804,#27375,#27376);
#24352=AXIS2_PLACEMENT_3D('',#33829,#27377,#27378);
#24353=AXIS2_PLACEMENT_3D('',#33854,#27379,#27380);
#24354=AXIS2_PLACEMENT_3D('',#33878,#27381,#27382);
#24355=AXIS2_PLACEMENT_3D('',#33879,#27383,#27384);
#24356=AXIS2_PLACEMENT_3D('',#33881,#27385,#27386);
#24357=AXIS2_PLACEMENT_3D('',#33882,#27387,#27388);
#24358=AXIS2_PLACEMENT_3D('',#33883,#27389,#27390);
#24359=AXIS2_PLACEMENT_3D('',#33907,#27391,#27392);
#24360=AXIS2_PLACEMENT_3D('',#33908,#27393,#27394);
#24361=AXIS2_PLACEMENT_3D('',#33910,#27395,#27396);
#24362=AXIS2_PLACEMENT_3D('',#33911,#27397,#27398);
#24363=AXIS2_PLACEMENT_3D('',#33912,#27399,#27400);
#24364=AXIS2_PLACEMENT_3D('',#33936,#27401,#27402);
#24365=AXIS2_PLACEMENT_3D('',#33937,#27403,#27404);
#24366=AXIS2_PLACEMENT_3D('',#33939,#27405,#27406);
#24367=AXIS2_PLACEMENT_3D('',#33941,#27407,#27408);
#24368=AXIS2_PLACEMENT_3D('',#33942,#27409,#27410);
#24369=AXIS2_PLACEMENT_3D('',#33943,#27411,#27412);
#24370=AXIS2_PLACEMENT_3D('',#33967,#27413,#27414);
#24371=AXIS2_PLACEMENT_3D('',#33968,#27415,#27416);
#24372=AXIS2_PLACEMENT_3D('',#33970,#27417,#27418);
#24373=AXIS2_PLACEMENT_3D('',#33971,#27419,#27420);
#24374=AXIS2_PLACEMENT_3D('',#33972,#27421,#27422);
#24375=AXIS2_PLACEMENT_3D('',#33996,#27423,#27424);
#24376=AXIS2_PLACEMENT_3D('',#33997,#27425,#27426);
#24377=AXIS2_PLACEMENT_3D('',#33999,#27427,#27428);
#24378=AXIS2_PLACEMENT_3D('',#34000,#27429,#27430);
#24379=AXIS2_PLACEMENT_3D('',#34001,#27431,#27432);
#24380=AXIS2_PLACEMENT_3D('',#34025,#27433,#27434);
#24381=AXIS2_PLACEMENT_3D('',#34026,#27435,#27436);
#24382=AXIS2_PLACEMENT_3D('',#34028,#27437,#27438);
#24383=AXIS2_PLACEMENT_3D('',#34031,#27440,#27441);
#24384=AXIS2_PLACEMENT_3D('',#34055,#27442,#27443);
#24385=AXIS2_PLACEMENT_3D('',#34056,#27444,#27445);
#24386=AXIS2_PLACEMENT_3D('',#34057,#27446,#27447);
#24387=AXIS2_PLACEMENT_3D('',#34058,#27448,#27449);
#24388=AXIS2_PLACEMENT_3D('',#34059,#27450,#27451);
#24389=AXIS2_PLACEMENT_3D('',#34060,#27452,#27453);
#24390=AXIS2_PLACEMENT_3D('',#34061,#27454,#27455);
#24391=AXIS2_PLACEMENT_3D('',#34062,#27456,#27457);
#24392=AXIS2_PLACEMENT_3D('',#34063,#27458,#27459);
#24393=AXIS2_PLACEMENT_3D('',#34065,#27460,#27461);
#24394=AXIS2_PLACEMENT_3D('',#34067,#27462,#27463);
#24395=AXIS2_PLACEMENT_3D('',#34068,#27464,#27465);
#24396=AXIS2_PLACEMENT_3D('',#34070,#27466,#27467);
#24397=AXIS2_PLACEMENT_3D('',#34072,#27469,#27470);
#24398=AXIS2_PLACEMENT_3D('',#34074,#27471,#27472);
#24399=AXIS2_PLACEMENT_3D('',#34075,#27473,#27474);
#24400=AXIS2_PLACEMENT_3D('',#34077,#27476,#27477);
#24401=AXIS2_PLACEMENT_3D('',#34079,#27478,#27479);
#24402=AXIS2_PLACEMENT_3D('',#34081,#27480,#27481);
#24403=AXIS2_PLACEMENT_3D('',#34082,#27482,#27483);
#24404=AXIS2_PLACEMENT_3D('',#34084,#27484,#27485);
#24405=AXIS2_PLACEMENT_3D('',#34086,#27487,#27488);
#24406=AXIS2_PLACEMENT_3D('',#34088,#27489,#27490);
#24407=AXIS2_PLACEMENT_3D('',#34089,#27491,#27492);
#24408=AXIS2_PLACEMENT_3D('',#34091,#27494,#27495);
#24409=AXIS2_PLACEMENT_3D('',#34092,#27496,#27497);
#24410=AXIS2_PLACEMENT_3D('',#34093,#27498,#27499);
#24411=AXIS2_PLACEMENT_3D('',#34094,#27500,#27501);
#24412=AXIS2_PLACEMENT_3D('',#34095,#27502,#27503);
#24413=AXIS2_PLACEMENT_3D('',#34096,#27504,#27505);
#24414=AXIS2_PLACEMENT_3D('',#34097,#27506,#27507);
#24415=AXIS2_PLACEMENT_3D('',#34098,#27508,#27509);
#24416=AXIS2_PLACEMENT_3D('',#34101,#27510,#27511);
#24417=AXIS2_PLACEMENT_3D('',#34102,#27512,#27513);
#24418=AXIS2_PLACEMENT_3D('',#34104,#27514,#27515);
#24419=AXIS2_PLACEMENT_3D('',#34106,#27516,#27517);
#24420=AXIS2_PLACEMENT_3D('',#34107,#27518,#27519);
#24421=AXIS2_PLACEMENT_3D('',#34108,#27520,#27521);
#24422=AXIS2_PLACEMENT_3D('',#34111,#27523,#27524);
#24423=AXIS2_PLACEMENT_3D('',#34112,#27525,#27526);
#24424=AXIS2_PLACEMENT_3D('',#34114,#27527,#27528);
#24425=AXIS2_PLACEMENT_3D('',#34117,#27530,#27531);
#24426=AXIS2_PLACEMENT_3D('',#34118,#27532,#27533);
#24427=AXIS2_PLACEMENT_3D('',#34121,#27535,#27536);
#24428=AXIS2_PLACEMENT_3D('',#34122,#27537,#27538);
#24429=AXIS2_PLACEMENT_3D('',#34123,#27539,#27540);
#24430=AXIS2_PLACEMENT_3D('',#34125,#27541,#27542);
#24431=AXIS2_PLACEMENT_3D('',#34127,#27544,#27545);
#24432=AXIS2_PLACEMENT_3D('',#34129,#27546,#27547);
#24433=AXIS2_PLACEMENT_3D('',#34130,#27548,#27549);
#24434=AXIS2_PLACEMENT_3D('',#34132,#27551,#27552);
#24435=AXIS2_PLACEMENT_3D('',#34133,#27553,#27554);
#24436=AXIS2_PLACEMENT_3D('',#34136,#27555,#27556);
#24437=AXIS2_PLACEMENT_3D('',#34137,#27557,#27558);
#24438=AXIS2_PLACEMENT_3D('',#34139,#27559,#27560);
#24439=AXIS2_PLACEMENT_3D('',#34141,#27561,#27562);
#24440=AXIS2_PLACEMENT_3D('',#34142,#27563,#27564);
#24441=AXIS2_PLACEMENT_3D('',#34143,#27565,#27566);
#24442=AXIS2_PLACEMENT_3D('',#34145,#27567,#27568);
#24443=AXIS2_PLACEMENT_3D('',#34147,#27570,#27571);
#24444=AXIS2_PLACEMENT_3D('',#34149,#27572,#27573);
#24445=AXIS2_PLACEMENT_3D('',#34151,#27574,#27575);
#24446=AXIS2_PLACEMENT_3D('',#34152,#27576,#27577);
#24447=AXIS2_PLACEMENT_3D('',#34154,#27578,#27579);
#24448=AXIS2_PLACEMENT_3D('',#34156,#27581,#27582);
#24449=AXIS2_PLACEMENT_3D('',#34158,#27583,#27584);
#24450=AXIS2_PLACEMENT_3D('',#34160,#27586,#27587);
#24451=AXIS2_PLACEMENT_3D('',#34162,#27588,#27589);
#24452=AXIS2_PLACEMENT_3D('',#34164,#27591,#27592);
#24453=AXIS2_PLACEMENT_3D('',#34165,#27593,#27594);
#24454=AXIS2_PLACEMENT_3D('',#34167,#27596,#27597);
#24455=AXIS2_PLACEMENT_3D('',#34168,#27598,#27599);
#24456=AXIS2_PLACEMENT_3D('',#34171,#27600,#27601);
#24457=AXIS2_PLACEMENT_3D('',#34172,#27602,#27603);
#24458=AXIS2_PLACEMENT_3D('',#34175,#27604,#27605);
#24459=AXIS2_PLACEMENT_3D('',#34176,#27606,#27607);
#24460=AXIS2_PLACEMENT_3D('',#34179,#27608,#27609);
#24461=AXIS2_PLACEMENT_3D('',#34180,#27610,#27611);
#24462=AXIS2_PLACEMENT_3D('',#34183,#27612,#27613);
#24463=AXIS2_PLACEMENT_3D('',#34184,#27614,#27615);
#24464=AXIS2_PLACEMENT_3D('',#34187,#27616,#27617);
#24465=AXIS2_PLACEMENT_3D('',#34188,#27618,#27619);
#24466=AXIS2_PLACEMENT_3D('',#34191,#27620,#27621);
#24467=AXIS2_PLACEMENT_3D('',#34192,#27622,#27623);
#24468=AXIS2_PLACEMENT_3D('',#34195,#27624,#27625);
#24469=AXIS2_PLACEMENT_3D('',#34196,#27626,#27627);
#24470=AXIS2_PLACEMENT_3D('',#34199,#27628,#27629);
#24471=AXIS2_PLACEMENT_3D('',#34200,#27630,#27631);
#24472=AXIS2_PLACEMENT_3D('',#34201,#27632,#27633);
#24473=AXIS2_PLACEMENT_3D('',#34227,#27634,#27635);
#24474=AXIS2_PLACEMENT_3D('',#34251,#27636,#27637);
#24475=AXIS2_PLACEMENT_3D('',#34252,#27638,#27639);
#24476=AXIS2_PLACEMENT_3D('',#34254,#27640,#27641);
#24477=AXIS2_PLACEMENT_3D('',#34279,#27642,#27643);
#24478=AXIS2_PLACEMENT_3D('',#34304,#27644,#27645);
#24479=AXIS2_PLACEMENT_3D('',#34320,#27647,#27648);
#24480=AXIS2_PLACEMENT_3D('',#34335,#27649,#27650);
#24481=AXIS2_PLACEMENT_3D('',#34360,#27651,#27652);
#24482=AXIS2_PLACEMENT_3D('',#34385,#27653,#27654);
#24483=AXIS2_PLACEMENT_3D('',#34410,#27655,#27656);
#24484=AXIS2_PLACEMENT_3D('',#34434,#27657,#27658);
#24485=AXIS2_PLACEMENT_3D('',#34435,#27659,#27660);
#24486=AXIS2_PLACEMENT_3D('',#34437,#27661,#27662);
#24487=AXIS2_PLACEMENT_3D('',#34438,#27663,#27664);
#24488=AXIS2_PLACEMENT_3D('',#34439,#27665,#27666);
#24489=AXIS2_PLACEMENT_3D('',#34463,#27667,#27668);
#24490=AXIS2_PLACEMENT_3D('',#34464,#27669,#27670);
#24491=AXIS2_PLACEMENT_3D('',#34466,#27671,#27672);
#24492=AXIS2_PLACEMENT_3D('',#34467,#27673,#27674);
#24493=AXIS2_PLACEMENT_3D('',#34468,#27675,#27676);
#24494=AXIS2_PLACEMENT_3D('',#34492,#27677,#27678);
#24495=AXIS2_PLACEMENT_3D('',#34493,#27679,#27680);
#24496=AXIS2_PLACEMENT_3D('',#34495,#27681,#27682);
#24497=AXIS2_PLACEMENT_3D('',#34496,#27683,#27684);
#24498=AXIS2_PLACEMENT_3D('',#34497,#27685,#27686);
#24499=AXIS2_PLACEMENT_3D('',#34512,#27687,#27688);
#24500=AXIS2_PLACEMENT_3D('',#34525,#27689,#27690);
#24501=AXIS2_PLACEMENT_3D('',#34527,#27691,#27692);
#24502=AXIS2_PLACEMENT_3D('',#34528,#27693,#27694);
#24503=AXIS2_PLACEMENT_3D('',#34529,#27695,#27696);
#24504=AXIS2_PLACEMENT_3D('',#34553,#27697,#27698);
#24505=AXIS2_PLACEMENT_3D('',#34554,#27699,#27700);
#24506=AXIS2_PLACEMENT_3D('',#34556,#27701,#27702);
#24507=AXIS2_PLACEMENT_3D('',#34557,#27703,#27704);
#24508=AXIS2_PLACEMENT_3D('',#34558,#27705,#27706);
#24509=AXIS2_PLACEMENT_3D('',#34582,#27707,#27708);
#24510=AXIS2_PLACEMENT_3D('',#34583,#27709,#27710);
#24511=AXIS2_PLACEMENT_3D('',#34585,#27711,#27712);
#24512=AXIS2_PLACEMENT_3D('',#34586,#27713,#27714);
#24513=AXIS2_PLACEMENT_3D('',#34587,#27715,#27716);
#24514=AXIS2_PLACEMENT_3D('',#34611,#27717,#27718);
#24515=AXIS2_PLACEMENT_3D('',#34612,#27719,#27720);
#24516=AXIS2_PLACEMENT_3D('',#34614,#27721,#27722);
#24517=AXIS2_PLACEMENT_3D('',#34617,#27724,#27725);
#24518=AXIS2_PLACEMENT_3D('',#34641,#27726,#27727);
#24519=AXIS2_PLACEMENT_3D('',#34642,#27728,#27729);
#24520=AXIS2_PLACEMENT_3D('',#34643,#27730,#27731);
#24521=AXIS2_PLACEMENT_3D('',#34644,#27732,#27733);
#24522=AXIS2_PLACEMENT_3D('',#34645,#27734,#27735);
#24523=AXIS2_PLACEMENT_3D('',#34646,#27736,#27737);
#24524=AXIS2_PLACEMENT_3D('',#34647,#27738,#27739);
#24525=AXIS2_PLACEMENT_3D('',#34648,#27740,#27741);
#24526=AXIS2_PLACEMENT_3D('',#34649,#27742,#27743);
#24527=AXIS2_PLACEMENT_3D('',#34651,#27744,#27745);
#24528=AXIS2_PLACEMENT_3D('',#34653,#27746,#27747);
#24529=AXIS2_PLACEMENT_3D('',#34654,#27748,#27749);
#24530=AXIS2_PLACEMENT_3D('',#34656,#27750,#27751);
#24531=AXIS2_PLACEMENT_3D('',#34658,#27753,#27754);
#24532=AXIS2_PLACEMENT_3D('',#34660,#27755,#27756);
#24533=AXIS2_PLACEMENT_3D('',#34661,#27757,#27758);
#24534=AXIS2_PLACEMENT_3D('',#34663,#27760,#27761);
#24535=AXIS2_PLACEMENT_3D('',#34665,#27762,#27763);
#24536=AXIS2_PLACEMENT_3D('',#34667,#27764,#27765);
#24537=AXIS2_PLACEMENT_3D('',#34668,#27766,#27767);
#24538=AXIS2_PLACEMENT_3D('',#34670,#27768,#27769);
#24539=AXIS2_PLACEMENT_3D('',#34672,#27771,#27772);
#24540=AXIS2_PLACEMENT_3D('',#34674,#27773,#27774);
#24541=AXIS2_PLACEMENT_3D('',#34675,#27775,#27776);
#24542=AXIS2_PLACEMENT_3D('',#34677,#27778,#27779);
#24543=AXIS2_PLACEMENT_3D('',#34678,#27780,#27781);
#24544=AXIS2_PLACEMENT_3D('',#34679,#27782,#27783);
#24545=AXIS2_PLACEMENT_3D('',#34680,#27784,#27785);
#24546=AXIS2_PLACEMENT_3D('',#34681,#27786,#27787);
#24547=AXIS2_PLACEMENT_3D('',#34682,#27788,#27789);
#24548=AXIS2_PLACEMENT_3D('',#34683,#27790,#27791);
#24549=AXIS2_PLACEMENT_3D('',#34684,#27792,#27793);
#24550=AXIS2_PLACEMENT_3D('',#34686,#27794,#27795);
#24551=AXIS2_PLACEMENT_3D('',#34689,#27797,#27798);
#24552=AXIS2_PLACEMENT_3D('',#34690,#27799,#27800);
#24553=AXIS2_PLACEMENT_3D('',#34692,#27801,#27802);
#24554=AXIS2_PLACEMENT_3D('',#34695,#27804,#27805);
#24555=AXIS2_PLACEMENT_3D('',#34696,#27806,#27807);
#24556=AXIS2_PLACEMENT_3D('',#34698,#27808,#27809);
#24557=AXIS2_PLACEMENT_3D('',#34701,#27811,#27812);
#24558=AXIS2_PLACEMENT_3D('',#34702,#27813,#27814);
#24559=AXIS2_PLACEMENT_3D('',#34704,#27815,#27816);
#24560=AXIS2_PLACEMENT_3D('',#34707,#27818,#27819);
#24561=AXIS2_PLACEMENT_3D('',#34708,#27820,#27821);
#24562=AXIS2_PLACEMENT_3D('',#34717,#27826,#27827);
#24563=AXIS2_PLACEMENT_3D('',#34723,#27831,#27832);
#24564=AXIS2_PLACEMENT_3D('',#34729,#27836,#27837);
#24565=AXIS2_PLACEMENT_3D('',#34732,#27840,#27841);
#24566=AXIS2_PLACEMENT_3D('',#34733,#27842,#27843);
#24567=AXIS2_PLACEMENT_3D('',#34734,#27844,#27845);
#24568=AXIS2_PLACEMENT_3D('',#34735,#27846,#27847);
#24569=AXIS2_PLACEMENT_3D('',#34737,#27848,#27849);
#24570=AXIS2_PLACEMENT_3D('',#34740,#27851,#27852);
#24571=AXIS2_PLACEMENT_3D('',#34741,#27853,#27854);
#24572=AXIS2_PLACEMENT_3D('',#34743,#27855,#27856);
#24573=AXIS2_PLACEMENT_3D('',#34746,#27858,#27859);
#24574=AXIS2_PLACEMENT_3D('',#34747,#27860,#27861);
#24575=AXIS2_PLACEMENT_3D('',#34749,#27862,#27863);
#24576=AXIS2_PLACEMENT_3D('',#34752,#27865,#27866);
#24577=AXIS2_PLACEMENT_3D('',#34753,#27867,#27868);
#24578=AXIS2_PLACEMENT_3D('',#34755,#27869,#27870);
#24579=AXIS2_PLACEMENT_3D('',#34758,#27872,#27873);
#24580=AXIS2_PLACEMENT_3D('',#34759,#27874,#27875);
#24581=AXIS2_PLACEMENT_3D('',#34761,#27876,#27877);
#24582=AXIS2_PLACEMENT_3D('',#34764,#27879,#27880);
#24583=AXIS2_PLACEMENT_3D('',#34765,#27881,#27882);
#24584=AXIS2_PLACEMENT_3D('',#34767,#27883,#27884);
#24585=AXIS2_PLACEMENT_3D('',#34770,#27886,#27887);
#24586=AXIS2_PLACEMENT_3D('',#34771,#27888,#27889);
#24587=AXIS2_PLACEMENT_3D('',#34773,#27890,#27891);
#24588=AXIS2_PLACEMENT_3D('',#34776,#27893,#27894);
#24589=AXIS2_PLACEMENT_3D('',#34777,#27895,#27896);
#24590=AXIS2_PLACEMENT_3D('',#34779,#27897,#27898);
#24591=AXIS2_PLACEMENT_3D('',#34782,#27900,#27901);
#24592=AXIS2_PLACEMENT_3D('',#34783,#27902,#27903);
#24593=AXIS2_PLACEMENT_3D('',#34785,#27904,#27905);
#24594=AXIS2_PLACEMENT_3D('',#34788,#27907,#27908);
#24595=AXIS2_PLACEMENT_3D('',#34789,#27909,#27910);
#24596=AXIS2_PLACEMENT_3D('',#34791,#27911,#27912);
#24597=AXIS2_PLACEMENT_3D('',#34794,#27914,#27915);
#24598=AXIS2_PLACEMENT_3D('',#34795,#27916,#27917);
#24599=AXIS2_PLACEMENT_3D('',#34797,#27918,#27919);
#24600=AXIS2_PLACEMENT_3D('',#34800,#27921,#27922);
#24601=AXIS2_PLACEMENT_3D('',#34801,#27923,#27924);
#24602=AXIS2_PLACEMENT_3D('',#34803,#27925,#27926);
#24603=AXIS2_PLACEMENT_3D('',#34806,#27928,#27929);
#24604=AXIS2_PLACEMENT_3D('',#34807,#27930,#27931);
#24605=AXIS2_PLACEMENT_3D('',#34816,#27936,#27937);
#24606=AXIS2_PLACEMENT_3D('',#34822,#27941,#27942);
#24607=AXIS2_PLACEMENT_3D('',#34828,#27946,#27947);
#24608=AXIS2_PLACEMENT_3D('',#34831,#27950,#27951);
#24609=AXIS2_PLACEMENT_3D('',#34832,#27952,#27953);
#24610=AXIS2_PLACEMENT_3D('',#34833,#27954,#27955);
#24611=AXIS2_PLACEMENT_3D('',#34834,#27956,#27957);
#24612=AXIS2_PLACEMENT_3D('',#34836,#27958,#27959);
#24613=AXIS2_PLACEMENT_3D('',#34839,#27961,#27962);
#24614=AXIS2_PLACEMENT_3D('',#34840,#27963,#27964);
#24615=AXIS2_PLACEMENT_3D('',#34841,#27965,#27966);
#24616=AXIS2_PLACEMENT_3D('',#34843,#27967,#27968);
#24617=AXIS2_PLACEMENT_3D('',#34846,#27970,#27971);
#24618=AXIS2_PLACEMENT_3D('',#34847,#27972,#27973);
#24619=AXIS2_PLACEMENT_3D('',#34848,#27974,#27975);
#24620=AXIS2_PLACEMENT_3D('',#34850,#27976,#27977);
#24621=AXIS2_PLACEMENT_3D('',#34853,#27979,#27980);
#24622=AXIS2_PLACEMENT_3D('',#34854,#27981,#27982);
#24623=AXIS2_PLACEMENT_3D('',#34855,#27983,#27984);
#24624=AXIS2_PLACEMENT_3D('',#34857,#27985,#27986);
#24625=AXIS2_PLACEMENT_3D('',#34860,#27988,#27989);
#24626=AXIS2_PLACEMENT_3D('',#34861,#27990,#27991);
#24627=AXIS2_PLACEMENT_3D('',#34862,#27992,#27993);
#24628=AXIS2_PLACEMENT_3D('',#34864,#27994,#27995);
#24629=AXIS2_PLACEMENT_3D('',#34867,#27997,#27998);
#24630=AXIS2_PLACEMENT_3D('',#34868,#27999,#28000);
#24631=AXIS2_PLACEMENT_3D('',#34869,#28001,#28002);
#24632=AXIS2_PLACEMENT_3D('',#34871,#28003,#28004);
#24633=AXIS2_PLACEMENT_3D('',#34874,#28006,#28007);
#24634=AXIS2_PLACEMENT_3D('',#34875,#28008,#28009);
#24635=AXIS2_PLACEMENT_3D('',#34876,#28010,#28011);
#24636=AXIS2_PLACEMENT_3D('',#34878,#28012,#28013);
#24637=AXIS2_PLACEMENT_3D('',#34881,#28015,#28016);
#24638=AXIS2_PLACEMENT_3D('',#34882,#28017,#28018);
#24639=AXIS2_PLACEMENT_3D('',#34883,#28019,#28020);
#24640=AXIS2_PLACEMENT_3D('',#34885,#28021,#28022);
#24641=AXIS2_PLACEMENT_3D('',#34888,#28024,#28025);
#24642=AXIS2_PLACEMENT_3D('',#34889,#28026,#28027);
#24643=AXIS2_PLACEMENT_3D('',#34898,#28032,#28033);
#24644=AXIS2_PLACEMENT_3D('',#34904,#28037,#28038);
#24645=AXIS2_PLACEMENT_3D('',#34910,#28042,#28043);
#24646=AXIS2_PLACEMENT_3D('',#34913,#28046,#28047);
#24647=AXIS2_PLACEMENT_3D('',#34914,#28048,#28049);
#24648=AXIS2_PLACEMENT_3D('',#34915,#28050,#28051);
#24649=AXIS2_PLACEMENT_3D('',#34916,#28052,#28053);
#24650=AXIS2_PLACEMENT_3D('',#34917,#28054,#28055);
#24651=AXIS2_PLACEMENT_3D('',#34921,#28057,#28058);
#24652=AXIS2_PLACEMENT_3D('',#34922,#28059,#28060);
#24653=AXIS2_PLACEMENT_3D('',#34926,#28062,#28063);
#24654=AXIS2_PLACEMENT_3D('',#34929,#28065,#28066);
#24655=AXIS2_PLACEMENT_3D('',#34931,#28067,#28068);
#24656=AXIS2_PLACEMENT_3D('',#34933,#28070,#28071);
#24657=AXIS2_PLACEMENT_3D('',#34937,#28073,#28074);
#24658=AXIS2_PLACEMENT_3D('',#34938,#28075,#28076);
#24659=AXIS2_PLACEMENT_3D('',#34942,#28078,#28079);
#24660=AXIS2_PLACEMENT_3D('',#34945,#28081,#28082);
#24661=AXIS2_PLACEMENT_3D('',#34947,#28083,#28084);
#24662=AXIS2_PLACEMENT_3D('',#34949,#28086,#28087);
#24663=AXIS2_PLACEMENT_3D('',#34953,#28089,#28090);
#24664=AXIS2_PLACEMENT_3D('',#34954,#28091,#28092);
#24665=AXIS2_PLACEMENT_3D('',#34958,#28094,#28095);
#24666=AXIS2_PLACEMENT_3D('',#34961,#28097,#28098);
#24667=AXIS2_PLACEMENT_3D('',#34963,#28099,#28100);
#24668=AXIS2_PLACEMENT_3D('',#34965,#28102,#28103);
#24669=AXIS2_PLACEMENT_3D('',#34969,#28105,#28106);
#24670=AXIS2_PLACEMENT_3D('',#34970,#28107,#28108);
#24671=AXIS2_PLACEMENT_3D('',#34974,#28110,#28111);
#24672=AXIS2_PLACEMENT_3D('',#34977,#28113,#28114);
#24673=AXIS2_PLACEMENT_3D('',#34979,#28115,#28116);
#24674=AXIS2_PLACEMENT_3D('',#34981,#28118,#28119);
#24675=AXIS2_PLACEMENT_3D('',#34992,#28126,#28127);
#24676=AXIS2_PLACEMENT_3D('',#35003,#28134,#28135);
#24677=AXIS2_PLACEMENT_3D('',#35022,#28146,#28147);
#24678=AXIS2_PLACEMENT_3D('',#35026,#28150,#28151);
#24679=AXIS2_PLACEMENT_3D('',#35030,#28154,#28155);
#24680=AXIS2_PLACEMENT_3D('',#35034,#28158,#28159);
#24681=AXIS2_PLACEMENT_3D('',#35038,#28162,#28163);
#24682=AXIS2_PLACEMENT_3D('',#35040,#28165,#28166);
#24683=AXIS2_PLACEMENT_3D('',#35044,#28169,#28170);
#24684=AXIS2_PLACEMENT_3D('',#35048,#28173,#28174);
#24685=AXIS2_PLACEMENT_3D('',#35052,#28177,#28178);
#24686=AXIS2_PLACEMENT_3D('',#35056,#28181,#28182);
#24687=AXIS2_PLACEMENT_3D('',#35058,#28184,#28185);
#24688=AXIS2_PLACEMENT_3D('',#35059,#28186,#28187);
#24689=AXIS2_PLACEMENT_3D('',#35060,#28188,#28189);
#24690=AXIS2_PLACEMENT_3D('',#35069,#28194,#28195);
#24691=AXIS2_PLACEMENT_3D('',#35075,#28199,#28200);
#24692=AXIS2_PLACEMENT_3D('',#35081,#28204,#28205);
#24693=AXIS2_PLACEMENT_3D('',#35087,#28209,#28210);
#24694=AXIS2_PLACEMENT_3D('',#35093,#28214,#28215);
#24695=AXIS2_PLACEMENT_3D('',#35099,#28219,#28220);
#24696=AXIS2_PLACEMENT_3D('',#35105,#28224,#28225);
#24697=AXIS2_PLACEMENT_3D('',#35108,#28228,#28229);
#24698=AXIS2_PLACEMENT_3D('',#35109,#28230,#28231);
#24699=AXIS2_PLACEMENT_3D('',#35110,#28232,#28233);
#24700=AXIS2_PLACEMENT_3D('',#35111,#28234,#28235);
#24701=AXIS2_PLACEMENT_3D('',#35120,#28240,#28241);
#24702=AXIS2_PLACEMENT_3D('',#35126,#28245,#28246);
#24703=AXIS2_PLACEMENT_3D('',#35132,#28250,#28251);
#24704=AXIS2_PLACEMENT_3D('',#35138,#28255,#28256);
#24705=AXIS2_PLACEMENT_3D('',#35144,#28260,#28261);
#24706=AXIS2_PLACEMENT_3D('',#35150,#28265,#28266);
#24707=AXIS2_PLACEMENT_3D('',#35156,#28270,#28271);
#24708=AXIS2_PLACEMENT_3D('',#35159,#28274,#28275);
#24709=AXIS2_PLACEMENT_3D('',#35160,#28276,#28277);
#24710=AXIS2_PLACEMENT_3D('',#35161,#28278,#28279);
#24711=AXIS2_PLACEMENT_3D('',#35162,#28280,#28281);
#24712=AXIS2_PLACEMENT_3D('',#35163,#28282,#28283);
#24713=AXIS2_PLACEMENT_3D('',#35164,#28284,#28285);
#24714=AXIS2_PLACEMENT_3D('',#35165,#28286,#28287);
#24715=AXIS2_PLACEMENT_3D('',#35167,#28288,#28289);
#24716=AXIS2_PLACEMENT_3D('',#35170,#28291,#28292);
#24717=AXIS2_PLACEMENT_3D('',#35171,#28293,#28294);
#24718=AXIS2_PLACEMENT_3D('',#35174,#28296,#28297);
#24719=AXIS2_PLACEMENT_3D('',#35175,#28298,#28299);
#24720=AXIS2_PLACEMENT_3D('',#35177,#28300,#28301);
#24721=AXIS2_PLACEMENT_3D('',#35178,#28302,#28303);
#24722=AXIS2_PLACEMENT_3D('',#35181,#28305,#28306);
#24723=AXIS2_PLACEMENT_3D('',#35182,#28307,#28308);
#24724=AXIS2_PLACEMENT_3D('',#35183,#28309,#28310);
#24725=AXIS2_PLACEMENT_3D('',#35184,#28311,#28312);
#24726=AXIS2_PLACEMENT_3D('',#35193,#28317,#28318);
#24727=AXIS2_PLACEMENT_3D('',#35199,#28322,#28323);
#24728=AXIS2_PLACEMENT_3D('',#35205,#28327,#28328);
#24729=AXIS2_PLACEMENT_3D('',#35211,#28332,#28333);
#24730=AXIS2_PLACEMENT_3D('',#35217,#28337,#28338);
#24731=AXIS2_PLACEMENT_3D('',#35220,#28341,#28342);
#24732=AXIS2_PLACEMENT_3D('',#35221,#28343,#28344);
#24733=AXIS2_PLACEMENT_3D('',#35222,#28345,#28346);
#24734=AXIS2_PLACEMENT_3D('',#35224,#28347,#28348);
#24735=AXIS2_PLACEMENT_3D('',#35226,#28349,#28350);
#24736=AXIS2_PLACEMENT_3D('',#35227,#28351,#28352);
#24737=AXIS2_PLACEMENT_3D('',#35230,#28354,#28355);
#24738=AXIS2_PLACEMENT_3D('',#35231,#28356,#28357);
#24739=AXIS2_PLACEMENT_3D('',#35232,#28358,#28359);
#24740=AXIS2_PLACEMENT_3D('',#35234,#28360,#28361);
#24741=AXIS2_PLACEMENT_3D('',#35235,#28362,#28363);
#24742=AXIS2_PLACEMENT_3D('',#35237,#28364,#28365);
#24743=AXIS2_PLACEMENT_3D('',#35239,#28367,#28368);
#24744=AXIS2_PLACEMENT_3D('',#35241,#28369,#28370);
#24745=AXIS2_PLACEMENT_3D('',#35243,#28372,#28373);
#24746=AXIS2_PLACEMENT_3D('',#35245,#28374,#28375);
#24747=AXIS2_PLACEMENT_3D('',#35247,#28377,#28378);
#24748=AXIS2_PLACEMENT_3D('',#35249,#28379,#28380);
#24749=AXIS2_PLACEMENT_3D('',#35250,#28381,#28382);
#24750=AXIS2_PLACEMENT_3D('',#35252,#28383,#28384);
#24751=AXIS2_PLACEMENT_3D('',#35254,#28386,#28387);
#24752=AXIS2_PLACEMENT_3D('',#35256,#28389,#28390);
#24753=AXIS2_PLACEMENT_3D('',#35257,#28391,#28392);
#24754=AXIS2_PLACEMENT_3D('',#35288,#28394,#28395);
#24755=AXIS2_PLACEMENT_3D('',#35329,#28396,#28397);
#24756=AXIS2_PLACEMENT_3D('',#35416,#28399,#28400);
#24757=AXIS2_PLACEMENT_3D('',#35506,#28402,#28403);
#24758=AXIS2_PLACEMENT_3D('',#35593,#28405,#28406);
#24759=AXIS2_PLACEMENT_3D('',#35683,#28408,#28409);
#24760=AXIS2_PLACEMENT_3D('',#35770,#28411,#28412);
#24761=AXIS2_PLACEMENT_3D('',#35857,#28414,#28415);
#24762=AXIS2_PLACEMENT_3D('',#35947,#28417,#28418);
#24763=AXIS2_PLACEMENT_3D('',#35952,#28420,#28421);
#24764=AXIS2_PLACEMENT_3D('',#35963,#28422,#28423);
#24765=AXIS2_PLACEMENT_3D('',#35976,#28425,#28426);
#24766=AXIS2_PLACEMENT_3D('',#35989,#28427,#28428);
#24767=AXIS2_PLACEMENT_3D('',#36026,#28430,#28431);
#24768=AXIS2_PLACEMENT_3D('',#36063,#28433,#28434);
#24769=AXIS2_PLACEMENT_3D('',#36101,#28436,#28437);
#24770=AXIS2_PLACEMENT_3D('',#36138,#28439,#28440);
#24771=AXIS2_PLACEMENT_3D('',#36175,#28442,#28443);
#24772=AXIS2_PLACEMENT_3D('',#36213,#28445,#28446);
#24773=AXIS2_PLACEMENT_3D('',#36251,#28448,#28449);
#24774=AXIS2_PLACEMENT_3D('',#36262,#28451,#28452);
#24775=AXIS2_PLACEMENT_3D('',#36273,#28453,#28454);
#24776=AXIS2_PLACEMENT_3D('',#37416,#28455,#28456);
#24777=AXIS2_PLACEMENT_3D('',#37420,#28458,#28459);
#24778=AXIS2_PLACEMENT_3D('',#37421,#28460,#28461);
#24779=AXIS2_PLACEMENT_3D('',#37423,#28462,#28463);
#24780=AXIS2_PLACEMENT_3D('',#37425,#28464,#28465);
#24781=AXIS2_PLACEMENT_3D('',#37427,#28466,#28467);
#24782=AXIS2_PLACEMENT_3D('',#37428,#28468,#28469);
#24783=AXIS2_PLACEMENT_3D('',#37430,#28470,#28471);
#24784=AXIS2_PLACEMENT_3D('',#37432,#28473,#28474);
#24785=AXIS2_PLACEMENT_3D('',#37434,#28475,#28476);
#24786=AXIS2_PLACEMENT_3D('',#37436,#28478,#28479);
#24787=AXIS2_PLACEMENT_3D('',#37438,#28480,#28481);
#24788=AXIS2_PLACEMENT_3D('',#37440,#28483,#28484);
#24789=AXIS2_PLACEMENT_3D('',#37446,#28488,#28489);
#24790=AXIS2_PLACEMENT_3D('',#37447,#28490,#28491);
#24791=AXIS2_PLACEMENT_3D('',#37449,#28492,#28493);
#24792=AXIS2_PLACEMENT_3D('',#37450,#28494,#28495);
#24793=AXIS2_PLACEMENT_3D('',#37451,#28496,#28497);
#24794=AXIS2_PLACEMENT_3D('',#37452,#28498,#28499);
#24795=AXIS2_PLACEMENT_3D('',#37455,#28501,#28502);
#24796=AXIS2_PLACEMENT_3D('',#37456,#28503,#28504);
#24797=AXIS2_PLACEMENT_3D('',#37457,#28505,#28506);
#24798=AXIS2_PLACEMENT_3D('',#37458,#28507,#28508);
#24799=AXIS2_PLACEMENT_3D('',#37460,#28509,#28510);
#24800=AXIS2_PLACEMENT_3D('',#37461,#28511,#28512);
#24801=AXIS2_PLACEMENT_3D('',#37463,#28513,#28514);
#24802=AXIS2_PLACEMENT_3D('',#37465,#28516,#28517);
#24803=AXIS2_PLACEMENT_3D('',#37467,#28518,#28519);
#24804=AXIS2_PLACEMENT_3D('',#37469,#28521,#28522);
#24805=AXIS2_PLACEMENT_3D('',#37471,#28523,#28524);
#24806=AXIS2_PLACEMENT_3D('',#37473,#28526,#28527);
#24807=AXIS2_PLACEMENT_3D('',#37475,#28528,#28529);
#24808=AXIS2_PLACEMENT_3D('',#37476,#28530,#28531);
#24809=AXIS2_PLACEMENT_3D('',#37478,#28532,#28533);
#24810=AXIS2_PLACEMENT_3D('',#37480,#28535,#28536);
#24811=AXIS2_PLACEMENT_3D('',#37482,#28537,#28538);
#24812=AXIS2_PLACEMENT_3D('',#37484,#28540,#28541);
#24813=AXIS2_PLACEMENT_3D('',#37486,#28542,#28543);
#24814=AXIS2_PLACEMENT_3D('',#37488,#28545,#28546);
#24815=AXIS2_PLACEMENT_3D('',#37489,#28547,#28548);
#24816=AXIS2_PLACEMENT_3D('',#37498,#28553,#28554);
#24817=AXIS2_PLACEMENT_3D('',#37504,#28558,#28559);
#24818=AXIS2_PLACEMENT_3D('',#37510,#28563,#28564);
#24819=AXIS2_PLACEMENT_3D('',#37516,#28568,#28569);
#24820=AXIS2_PLACEMENT_3D('',#37522,#28573,#28574);
#24821=AXIS2_PLACEMENT_3D('',#37525,#28577,#28578);
#24822=AXIS2_PLACEMENT_3D('',#37526,#28579,#28580);
#24823=AXIS2_PLACEMENT_3D('',#37527,#28581,#28582);
#24824=AXIS2_PLACEMENT_3D('',#37528,#28583,#28584);
#24825=AXIS2_PLACEMENT_3D('',#37530,#28585,#28586);
#24826=AXIS2_PLACEMENT_3D('',#37531,#28587,#28588);
#24827=AXIS2_PLACEMENT_3D('',#37533,#28589,#28590);
#24828=AXIS2_PLACEMENT_3D('',#37535,#28592,#28593);
#24829=AXIS2_PLACEMENT_3D('',#37537,#28594,#28595);
#24830=AXIS2_PLACEMENT_3D('',#37539,#28597,#28598);
#24831=AXIS2_PLACEMENT_3D('',#37541,#28599,#28600);
#24832=AXIS2_PLACEMENT_3D('',#37543,#28602,#28603);
#24833=AXIS2_PLACEMENT_3D('',#37545,#28604,#28605);
#24834=AXIS2_PLACEMENT_3D('',#37546,#28606,#28607);
#24835=AXIS2_PLACEMENT_3D('',#37548,#28608,#28609);
#24836=AXIS2_PLACEMENT_3D('',#37550,#28611,#28612);
#24837=AXIS2_PLACEMENT_3D('',#37552,#28613,#28614);
#24838=AXIS2_PLACEMENT_3D('',#37554,#28616,#28617);
#24839=AXIS2_PLACEMENT_3D('',#37556,#28618,#28619);
#24840=AXIS2_PLACEMENT_3D('',#37558,#28621,#28622);
#24841=AXIS2_PLACEMENT_3D('',#37559,#28623,#28624);
#24842=AXIS2_PLACEMENT_3D('',#37568,#28629,#28630);
#24843=AXIS2_PLACEMENT_3D('',#37574,#28634,#28635);
#24844=AXIS2_PLACEMENT_3D('',#37580,#28639,#28640);
#24845=AXIS2_PLACEMENT_3D('',#37586,#28644,#28645);
#24846=AXIS2_PLACEMENT_3D('',#37592,#28649,#28650);
#24847=AXIS2_PLACEMENT_3D('',#37595,#28653,#28654);
#24848=AXIS2_PLACEMENT_3D('',#37596,#28655,#28656);
#24849=AXIS2_PLACEMENT_3D('',#37597,#28657,#28658);
#24850=AXIS2_PLACEMENT_3D('',#37598,#28659,#28660);
#24851=AXIS2_PLACEMENT_3D('',#37599,#28661,#28662);
#24852=AXIS2_PLACEMENT_3D('',#37600,#28663,#28664);
#24853=AXIS2_PLACEMENT_3D('',#37601,#28665,#28666);
#24854=AXIS2_PLACEMENT_3D('',#37602,#28667,#28668);
#24855=AXIS2_PLACEMENT_3D('',#37603,#28669,#28670);
#24856=AXIS2_PLACEMENT_3D('',#37604,#28671,#28672);
#24857=AXIS2_PLACEMENT_3D('',#37605,#28673,#28674);
#24858=AXIS2_PLACEMENT_3D('',#37606,#28675,#28676);
#24859=AXIS2_PLACEMENT_3D('',#37607,#28677,#28678);
#24860=AXIS2_PLACEMENT_3D('',#37608,#28679,#28680);
#24861=AXIS2_PLACEMENT_3D('',#37609,#28681,#28682);
#24862=AXIS2_PLACEMENT_3D('',#37610,#28683,#28684);
#24863=AXIS2_PLACEMENT_3D('',#37611,#28685,#28686);
#24864=AXIS2_PLACEMENT_3D('',#37612,#28687,#28688);
#24865=AXIS2_PLACEMENT_3D('',#37613,#28689,#28690);
#24866=AXIS2_PLACEMENT_3D('',#37614,#28691,#28692);
#24867=AXIS2_PLACEMENT_3D('',#37615,#28693,#28694);
#24868=AXIS2_PLACEMENT_3D('',#37616,#28695,#28696);
#24869=AXIS2_PLACEMENT_3D('',#37617,#28697,#28698);
#24870=AXIS2_PLACEMENT_3D('',#37618,#28699,#28700);
#24871=AXIS2_PLACEMENT_3D('',#37619,#28701,#28702);
#24872=AXIS2_PLACEMENT_3D('',#37644,#28704,#28705);
#24873=AXIS2_PLACEMENT_3D('',#37649,#28706,#28707);
#24874=AXIS2_PLACEMENT_3D('',#37736,#28709,#28710);
#24875=AXIS2_PLACEMENT_3D('',#37826,#28712,#28713);
#24876=AXIS2_PLACEMENT_3D('',#37913,#28715,#28716);
#24877=AXIS2_PLACEMENT_3D('',#38000,#28718,#28719);
#24878=AXIS2_PLACEMENT_3D('',#38087,#28721,#28722);
#24879=AXIS2_PLACEMENT_3D('',#38174,#28724,#28725);
#24880=AXIS2_PLACEMENT_3D('',#38261,#28727,#28728);
#24881=AXIS2_PLACEMENT_3D('',#38333,#28730,#28731);
#24882=AXIS2_PLACEMENT_3D('',#38384,#28733,#28734);
#24883=AXIS2_PLACEMENT_3D('',#38432,#28736,#28737);
#24884=AXIS2_PLACEMENT_3D('',#38480,#28739,#28740);
#24885=AXIS2_PLACEMENT_3D('',#38531,#28742,#28743);
#24886=AXIS2_PLACEMENT_3D('',#38582,#28745,#28746);
#24887=AXIS2_PLACEMENT_3D('',#38630,#28748,#28749);
#24888=AXIS2_PLACEMENT_3D('',#38681,#28751,#28752);
#24889=AXIS2_PLACEMENT_3D('',#38732,#28754,#28755);
#24890=AXIS2_PLACEMENT_3D('',#38780,#28757,#28758);
#24891=AXIS2_PLACEMENT_3D('',#38828,#28760,#28761);
#24892=AXIS2_PLACEMENT_3D('',#38879,#28763,#28764);
#24893=AXIS2_PLACEMENT_3D('',#38930,#28766,#28767);
#24894=AXIS2_PLACEMENT_3D('',#38978,#28769,#28770);
#24895=AXIS2_PLACEMENT_3D('',#39029,#28772,#28773);
#24896=AXIS2_PLACEMENT_3D('',#39080,#28775,#28776);
#24897=AXIS2_PLACEMENT_3D('',#39128,#28778,#28779);
#24898=AXIS2_PLACEMENT_3D('',#39176,#28781,#28782);
#24899=AXIS2_PLACEMENT_3D('',#39227,#28784,#28785);
#24900=AXIS2_PLACEMENT_3D('',#39278,#28787,#28788);
#24901=AXIS2_PLACEMENT_3D('',#39326,#28790,#28791);
#24902=AXIS2_PLACEMENT_3D('',#39377,#28793,#28794);
#24903=AXIS2_PLACEMENT_3D('',#39428,#28796,#28797);
#24904=AXIS2_PLACEMENT_3D('',#39476,#28799,#28800);
#24905=AXIS2_PLACEMENT_3D('',#39524,#28802,#28803);
#24906=AXIS2_PLACEMENT_3D('',#39575,#28805,#28806);
#24907=AXIS2_PLACEMENT_3D('',#39626,#28808,#28809);
#24908=AXIS2_PLACEMENT_3D('',#39674,#28811,#28812);
#24909=AXIS2_PLACEMENT_3D('',#39725,#28814,#28815);
#24910=AXIS2_PLACEMENT_3D('',#39776,#28817,#28818);
#24911=AXIS2_PLACEMENT_3D('',#39824,#28820,#28821);
#24912=AXIS2_PLACEMENT_3D('',#39872,#28823,#28824);
#24913=AXIS2_PLACEMENT_3D('',#39923,#28826,#28827);
#24914=AXIS2_PLACEMENT_3D('',#39974,#28829,#28830);
#24915=AXIS2_PLACEMENT_3D('',#40022,#28832,#28833);
#24916=AXIS2_PLACEMENT_3D('',#40073,#28835,#28836);
#24917=AXIS2_PLACEMENT_3D('',#40124,#28838,#28839);
#24918=AXIS2_PLACEMENT_3D('',#40172,#28841,#28842);
#24919=AXIS2_PLACEMENT_3D('',#40220,#28844,#28845);
#24920=AXIS2_PLACEMENT_3D('',#40271,#28847,#28848);
#24921=AXIS2_PLACEMENT_3D('',#40322,#28850,#28851);
#24922=AXIS2_PLACEMENT_3D('',#40370,#28853,#28854);
#24923=AXIS2_PLACEMENT_3D('',#40421,#28856,#28857);
#24924=AXIS2_PLACEMENT_3D('',#40472,#28859,#28860);
#24925=AXIS2_PLACEMENT_3D('',#40520,#28862,#28863);
#24926=AXIS2_PLACEMENT_3D('',#40568,#28865,#28866);
#24927=AXIS2_PLACEMENT_3D('',#40619,#28868,#28869);
#24928=AXIS2_PLACEMENT_3D('',#40685,#28871,#28872);
#24929=AXIS2_PLACEMENT_3D('',#40775,#28874,#28875);
#24930=AXIS2_PLACEMENT_3D('',#40862,#28877,#28878);
#24931=AXIS2_PLACEMENT_3D('',#40949,#28880,#28881);
#24932=AXIS2_PLACEMENT_3D('',#41036,#28883,#28884);
#24933=AXIS2_PLACEMENT_3D('',#41123,#28886,#28887);
#24934=AXIS2_PLACEMENT_3D('',#41210,#28889,#28890);
#24935=AXIS2_PLACEMENT_3D('',#41300,#28892,#28893);
#24936=AXIS2_PLACEMENT_3D('',#41309,#28895,#28896);
#24937=AXIS2_PLACEMENT_3D('',#41310,#28897,#28898);
#24938=AXIS2_PLACEMENT_3D('',#41332,#28900,#28901);
#24939=AXIS2_PLACEMENT_3D('',#41346,#28902,#28903);
#24940=AXIS2_PLACEMENT_3D('',#41384,#28905,#28906);
#24941=AXIS2_PLACEMENT_3D('',#41420,#28908,#28909);
#24942=AXIS2_PLACEMENT_3D('',#41458,#28911,#28912);
#24943=AXIS2_PLACEMENT_3D('',#41494,#28914,#28915);
#24944=AXIS2_PLACEMENT_3D('',#41532,#28917,#28918);
#24945=AXIS2_PLACEMENT_3D('',#41569,#28920,#28921);
#24946=AXIS2_PLACEMENT_3D('',#41604,#28923,#28924);
#24947=AXIS2_PLACEMENT_3D('',#41631,#28926,#28927);
#24948=AXIS2_PLACEMENT_3D('',#41655,#28929,#28930);
#24949=AXIS2_PLACEMENT_3D('',#41679,#28932,#28933);
#24950=AXIS2_PLACEMENT_3D('',#41703,#28935,#28936);
#24951=AXIS2_PLACEMENT_3D('',#41729,#28938,#28939);
#24952=AXIS2_PLACEMENT_3D('',#41753,#28941,#28942);
#24953=AXIS2_PLACEMENT_3D('',#41777,#28944,#28945);
#24954=AXIS2_PLACEMENT_3D('',#41803,#28947,#28948);
#24955=AXIS2_PLACEMENT_3D('',#41827,#28950,#28951);
#24956=AXIS2_PLACEMENT_3D('',#41851,#28953,#28954);
#24957=AXIS2_PLACEMENT_3D('',#41875,#28956,#28957);
#24958=AXIS2_PLACEMENT_3D('',#41901,#28959,#28960);
#24959=AXIS2_PLACEMENT_3D('',#41925,#28962,#28963);
#24960=AXIS2_PLACEMENT_3D('',#41949,#28965,#28966);
#24961=AXIS2_PLACEMENT_3D('',#41975,#28968,#28969);
#24962=AXIS2_PLACEMENT_3D('',#41999,#28971,#28972);
#24963=AXIS2_PLACEMENT_3D('',#42023,#28974,#28975);
#24964=AXIS2_PLACEMENT_3D('',#42047,#28977,#28978);
#24965=AXIS2_PLACEMENT_3D('',#42073,#28980,#28981);
#24966=AXIS2_PLACEMENT_3D('',#42097,#28983,#28984);
#24967=AXIS2_PLACEMENT_3D('',#42121,#28986,#28987);
#24968=AXIS2_PLACEMENT_3D('',#42147,#28989,#28990);
#24969=AXIS2_PLACEMENT_3D('',#42171,#28992,#28993);
#24970=AXIS2_PLACEMENT_3D('',#42195,#28995,#28996);
#24971=AXIS2_PLACEMENT_3D('',#42219,#28998,#28999);
#24972=AXIS2_PLACEMENT_3D('',#42245,#29001,#29002);
#24973=AXIS2_PLACEMENT_3D('',#42269,#29004,#29005);
#24974=AXIS2_PLACEMENT_3D('',#42293,#29007,#29008);
#24975=AXIS2_PLACEMENT_3D('',#42319,#29010,#29011);
#24976=AXIS2_PLACEMENT_3D('',#42343,#29013,#29014);
#24977=AXIS2_PLACEMENT_3D('',#42367,#29016,#29017);
#24978=AXIS2_PLACEMENT_3D('',#42391,#29019,#29020);
#24979=AXIS2_PLACEMENT_3D('',#42417,#29022,#29023);
#24980=AXIS2_PLACEMENT_3D('',#42441,#29025,#29026);
#24981=AXIS2_PLACEMENT_3D('',#42465,#29028,#29029);
#24982=AXIS2_PLACEMENT_3D('',#42491,#29031,#29032);
#24983=AXIS2_PLACEMENT_3D('',#42515,#29034,#29035);
#24984=AXIS2_PLACEMENT_3D('',#42539,#29037,#29038);
#24985=AXIS2_PLACEMENT_3D('',#42563,#29040,#29041);
#24986=AXIS2_PLACEMENT_3D('',#42589,#29043,#29044);
#24987=AXIS2_PLACEMENT_3D('',#42613,#29046,#29047);
#24988=AXIS2_PLACEMENT_3D('',#42637,#29049,#29050);
#24989=AXIS2_PLACEMENT_3D('',#42663,#29052,#29053);
#24990=AXIS2_PLACEMENT_3D('',#42687,#29055,#29056);
#24991=AXIS2_PLACEMENT_3D('',#42711,#29058,#29059);
#24992=AXIS2_PLACEMENT_3D('',#42736,#29061,#29062);
#24993=AXIS2_PLACEMENT_3D('',#42763,#29064,#29065);
#24994=AXIS2_PLACEMENT_3D('',#42800,#29067,#29068);
#24995=AXIS2_PLACEMENT_3D('',#42836,#29070,#29071);
#24996=AXIS2_PLACEMENT_3D('',#42874,#29073,#29074);
#24997=AXIS2_PLACEMENT_3D('',#42910,#29076,#29077);
#24998=AXIS2_PLACEMENT_3D('',#42948,#29079,#29080);
#24999=AXIS2_PLACEMENT_3D('',#42985,#29082,#29083);
#25000=AXIS2_PLACEMENT_3D('',#43022,#29085,#29086);
#25001=AXIS2_PLACEMENT_3D('',#43024,#29087,#29088);
#25002=AXIS2_PLACEMENT_3D('',#43101,#29089,#29090);
#25003=AXIS2_PLACEMENT_3D('',#43102,#29091,#29092);
#25004=AXIS2_PLACEMENT_3D('',#43105,#29094,#29095);
#25005=AXIS2_PLACEMENT_3D('',#43106,#29096,#29097);
#25006=AXIS2_PLACEMENT_3D('',#45180,#29098,#29099);
#25007=AXIS2_PLACEMENT_3D('',#47235,#29100,#29101);
#25008=AXIS2_PLACEMENT_3D('',#47244,#29106,#29107);
#25009=AXIS2_PLACEMENT_3D('',#47246,#29108,#29109);
#25010=AXIS2_PLACEMENT_3D('',#47250,#29112,#29113);
#25011=AXIS2_PLACEMENT_3D('',#47254,#29116,#29117);
#25012=AXIS2_PLACEMENT_3D('',#47258,#29120,#29121);
#25013=AXIS2_PLACEMENT_3D('',#47259,#29122,#29123);
#25014=AXIS2_PLACEMENT_3D('',#47260,#29124,#29125);
#25015=AXIS2_PLACEMENT_3D('',#47262,#29126,#29127);
#25016=AXIS2_PLACEMENT_3D('',#47265,#29129,#29130);
#25017=AXIS2_PLACEMENT_3D('',#47266,#29131,#29132);
#25018=AXIS2_PLACEMENT_3D('',#47267,#29133,#29134);
#25019=AXIS2_PLACEMENT_3D('',#47269,#29135,#29136);
#25020=AXIS2_PLACEMENT_3D('',#47270,#29137,#29138);
#25021=AXIS2_PLACEMENT_3D('',#47271,#29139,#29140);
#25022=AXIS2_PLACEMENT_3D('',#47273,#29141,#29142);
#25023=AXIS2_PLACEMENT_3D('',#47275,#29144,#29145);
#25024=AXIS2_PLACEMENT_3D('',#47276,#29146,#29147);
#25025=AXIS2_PLACEMENT_3D('',#47277,#29148,#29149);
#25026=AXIS2_PLACEMENT_3D('',#47278,#29150,#29151);
#25027=AXIS2_PLACEMENT_3D('',#47280,#29152,#29153);
#25028=AXIS2_PLACEMENT_3D('',#47283,#29155,#29156);
#25029=AXIS2_PLACEMENT_3D('',#47284,#29157,#29158);
#25030=AXIS2_PLACEMENT_3D('',#47286,#29159,#29160);
#25031=AXIS2_PLACEMENT_3D('',#47289,#29162,#29163);
#25032=AXIS2_PLACEMENT_3D('',#47290,#29164,#29165);
#25033=AXIS2_PLACEMENT_3D('',#47291,#29166,#29167);
#25034=AXIS2_PLACEMENT_3D('',#47292,#29168,#29169);
#25035=AXIS2_PLACEMENT_3D('',#47293,#29170,#29171);
#25036=AXIS2_PLACEMENT_3D('',#47297,#29173,#29174);
#25037=AXIS2_PLACEMENT_3D('',#47298,#29175,#29176);
#25038=AXIS2_PLACEMENT_3D('',#47310,#29177,#29178);
#25039=AXIS2_PLACEMENT_3D('',#47372,#29180,#29181);
#25040=AXIS2_PLACEMENT_3D('',#47374,#29183,#29184);
#25041=AXIS2_PLACEMENT_3D('',#47376,#29185,#29186);
#25042=AXIS2_PLACEMENT_3D('',#47379,#29188,#29189);
#25043=AXIS2_PLACEMENT_3D('',#47380,#29190,#29191);
#25044=AXIS2_PLACEMENT_3D('',#47382,#29192,#29193);
#25045=AXIS2_PLACEMENT_3D('',#47385,#29195,#29196);
#25046=AXIS2_PLACEMENT_3D('',#47386,#29197,#29198);
#25047=AXIS2_PLACEMENT_3D('',#47387,#29199,#29200);
#25048=AXIS2_PLACEMENT_3D('',#47388,#29201,#29202);
#25049=AXIS2_PLACEMENT_3D('',#47389,#29203,#29204);
#25050=AXIS2_PLACEMENT_3D('',#47391,#29205,#29206);
#25051=AXIS2_PLACEMENT_3D('',#47394,#29208,#29209);
#25052=AXIS2_PLACEMENT_3D('',#47395,#29210,#29211);
#25053=AXIS2_PLACEMENT_3D('',#47399,#29213,#29214);
#25054=AXIS2_PLACEMENT_3D('',#47400,#29215,#29216);
#25055=AXIS2_PLACEMENT_3D('',#47410,#29217,#29218);
#25056=AXIS2_PLACEMENT_3D('',#47466,#29220,#29221);
#25057=AXIS2_PLACEMENT_3D('',#47468,#29223,#29224);
#25058=AXIS2_PLACEMENT_3D('',#47481,#29231,#29232);
#25059=AXIS2_PLACEMENT_3D('',#47487,#29236,#29237);
#25060=AXIS2_PLACEMENT_3D('',#47497,#29243,#29244);
#25061=AXIS2_PLACEMENT_3D('',#47499,#29245,#29246);
#25062=AXIS2_PLACEMENT_3D('',#47500,#29247,#29248);
#25063=AXIS2_PLACEMENT_3D('',#47501,#29249,#29250);
#25064=AXIS2_PLACEMENT_3D('',#47503,#29251,#29252);
#25065=AXIS2_PLACEMENT_3D('',#47504,#29253,#29254);
#25066=AXIS2_PLACEMENT_3D('',#47505,#29255,#29256);
#25067=AXIS2_PLACEMENT_3D('',#47507,#29258,#29259);
#25068=AXIS2_PLACEMENT_3D('',#47508,#29260,#29261);
#25069=AXIS2_PLACEMENT_3D('',#47509,#29262,#29263);
#25070=AXIS2_PLACEMENT_3D('',#47510,#29264,#29265);
#25071=AXIS2_PLACEMENT_3D('',#47511,#29266,#29267);
#25072=AXIS2_PLACEMENT_3D('',#47512,#29268,#29269);
#25073=AXIS2_PLACEMENT_3D('',#47513,#29270,#29271);
#25074=AXIS2_PLACEMENT_3D('',#47515,#29272,#29273);
#25075=AXIS2_PLACEMENT_3D('',#47518,#29275,#29276);
#25076=AXIS2_PLACEMENT_3D('',#47519,#29277,#29278);
#25077=AXIS2_PLACEMENT_3D('',#47521,#29279,#29280);
#25078=AXIS2_PLACEMENT_3D('',#47524,#29282,#29283);
#25079=AXIS2_PLACEMENT_3D('',#47525,#29284,#29285);
#25080=AXIS2_PLACEMENT_3D('',#47526,#29286,#29287);
#25081=AXIS2_PLACEMENT_3D('',#47527,#29288,#29289);
#25082=AXIS2_PLACEMENT_3D('',#47528,#29290,#29291);
#25083=AXIS2_PLACEMENT_3D('',#47530,#29292,#29293);
#25084=AXIS2_PLACEMENT_3D('',#47533,#29295,#29296);
#25085=AXIS2_PLACEMENT_3D('',#47534,#29297,#29298);
#25086=AXIS2_PLACEMENT_3D('',#47536,#29299,#29300);
#25087=AXIS2_PLACEMENT_3D('',#47539,#29302,#29303);
#25088=AXIS2_PLACEMENT_3D('',#47540,#29304,#29305);
#25089=AXIS2_PLACEMENT_3D('',#47541,#29306,#29307);
#25090=AXIS2_PLACEMENT_3D('',#47542,#29308,#29309);
#25091=AXIS2_PLACEMENT_3D('',#47543,#29310,#29311);
#25092=AXIS2_PLACEMENT_3D('',#47560,#29320,#29321);
#25093=AXIS2_PLACEMENT_3D('',#47566,#29325,#29326);
#25094=AXIS2_PLACEMENT_3D('',#47570,#29329,#29330);
#25095=AXIS2_PLACEMENT_3D('',#47574,#29333,#29334);
#25096=AXIS2_PLACEMENT_3D('',#47578,#29337,#29338);
#25097=AXIS2_PLACEMENT_3D('',#47586,#29343,#29344);
#25098=AXIS2_PLACEMENT_3D('',#47588,#29346,#29347);
#25099=AXIS2_PLACEMENT_3D('',#47590,#29349,#29350);
#25100=AXIS2_PLACEMENT_3D('',#47592,#29352,#29353);
#25101=AXIS2_PLACEMENT_3D('',#47593,#29354,#29355);
#25102=AXIS2_PLACEMENT_3D('',#47594,#29356,#29357);
#25103=AXIS2_PLACEMENT_3D('',#47603,#29362,#29363);
#25104=AXIS2_PLACEMENT_3D('',#47609,#29367,#29368);
#25105=AXIS2_PLACEMENT_3D('',#47615,#29372,#29373);
#25106=AXIS2_PLACEMENT_3D('',#47621,#29377,#29378);
#25107=AXIS2_PLACEMENT_3D('',#47627,#29382,#29383);
#25108=AXIS2_PLACEMENT_3D('',#47630,#29386,#29387);
#25109=AXIS2_PLACEMENT_3D('',#47631,#29388,#29389);
#25110=AXIS2_PLACEMENT_3D('',#47633,#29390,#29391);
#25111=AXIS2_PLACEMENT_3D('',#47634,#29392,#29393);
#25112=AXIS2_PLACEMENT_3D('',#47636,#29394,#29395);
#25113=AXIS2_PLACEMENT_3D('',#47638,#29397,#29398);
#25114=AXIS2_PLACEMENT_3D('',#47640,#29399,#29400);
#25115=AXIS2_PLACEMENT_3D('',#47642,#29402,#29403);
#25116=AXIS2_PLACEMENT_3D('',#47644,#29404,#29405);
#25117=AXIS2_PLACEMENT_3D('',#47646,#29407,#29408);
#25118=AXIS2_PLACEMENT_3D('',#47647,#29409,#29410);
#25119=AXIS2_PLACEMENT_3D('',#47648,#29411,#29412);
#25120=AXIS2_PLACEMENT_3D('',#47650,#29413,#29414);
#25121=AXIS2_PLACEMENT_3D('',#47653,#29416,#29417);
#25122=AXIS2_PLACEMENT_3D('',#47654,#29418,#29419);
#25123=AXIS2_PLACEMENT_3D('',#47656,#29420,#29421);
#25124=AXIS2_PLACEMENT_3D('',#47659,#29423,#29424);
#25125=AXIS2_PLACEMENT_3D('',#47660,#29425,#29426);
#25126=AXIS2_PLACEMENT_3D('',#47661,#29427,#29428);
#25127=AXIS2_PLACEMENT_3D('',#47662,#29429,#29430);
#25128=AXIS2_PLACEMENT_3D('',#47663,#29431,#29432);
#25129=AXIS2_PLACEMENT_3D('',#47665,#29433,#29434);
#25130=AXIS2_PLACEMENT_3D('',#47666,#29435,#29436);
#25131=AXIS2_PLACEMENT_3D('',#47668,#29437,#29438);
#25132=AXIS2_PLACEMENT_3D('',#47670,#29440,#29441);
#25133=AXIS2_PLACEMENT_3D('',#47672,#29442,#29443);
#25134=AXIS2_PLACEMENT_3D('',#47674,#29445,#29446);
#25135=AXIS2_PLACEMENT_3D('',#47676,#29447,#29448);
#25136=AXIS2_PLACEMENT_3D('',#47678,#29450,#29451);
#25137=AXIS2_PLACEMENT_3D('',#47680,#29452,#29453);
#25138=AXIS2_PLACEMENT_3D('',#47681,#29454,#29455);
#25139=AXIS2_PLACEMENT_3D('',#47683,#29456,#29457);
#25140=AXIS2_PLACEMENT_3D('',#47685,#29459,#29460);
#25141=AXIS2_PLACEMENT_3D('',#47687,#29461,#29462);
#25142=AXIS2_PLACEMENT_3D('',#47689,#29464,#29465);
#25143=AXIS2_PLACEMENT_3D('',#47691,#29466,#29467);
#25144=AXIS2_PLACEMENT_3D('',#47693,#29469,#29470);
#25145=AXIS2_PLACEMENT_3D('',#47694,#29471,#29472);
#25146=AXIS2_PLACEMENT_3D('',#47703,#29477,#29478);
#25147=AXIS2_PLACEMENT_3D('',#47709,#29482,#29483);
#25148=AXIS2_PLACEMENT_3D('',#47715,#29487,#29488);
#25149=AXIS2_PLACEMENT_3D('',#47721,#29492,#29493);
#25150=AXIS2_PLACEMENT_3D('',#47727,#29497,#29498);
#25151=AXIS2_PLACEMENT_3D('',#47730,#29501,#29502);
#25152=AXIS2_PLACEMENT_3D('',#47731,#29503,#29504);
#25153=AXIS2_PLACEMENT_3D('',#47732,#29505,#29506);
#25154=AXIS2_PLACEMENT_3D('',#47733,#29507,#29508);
#25155=AXIS2_PLACEMENT_3D('',#47734,#29509,#29510);
#25156=AXIS2_PLACEMENT_3D('',#47735,#29511,#29512);
#25157=AXIS2_PLACEMENT_3D('',#47736,#29513,#29514);
#25158=AXIS2_PLACEMENT_3D('',#47737,#29515,#29516);
#25159=AXIS2_PLACEMENT_3D('',#47738,#29517,#29518);
#25160=AXIS2_PLACEMENT_3D('',#47739,#29519,#29520);
#25161=AXIS2_PLACEMENT_3D('',#47740,#29521,#29522);
#25162=AXIS2_PLACEMENT_3D('',#47741,#29523,#29524);
#25163=AXIS2_PLACEMENT_3D('',#47742,#29525,#29526);
#25164=AXIS2_PLACEMENT_3D('',#47743,#29527,#29528);
#25165=AXIS2_PLACEMENT_3D('',#47744,#29529,#29530);
#25166=AXIS2_PLACEMENT_3D('',#47745,#29531,#29532);
#25167=AXIS2_PLACEMENT_3D('',#47746,#29533,#29534);
#25168=AXIS2_PLACEMENT_3D('',#47747,#29535,#29536);
#25169=AXIS2_PLACEMENT_3D('',#47748,#29537,#29538);
#25170=AXIS2_PLACEMENT_3D('',#47749,#29539,#29540);
#25171=AXIS2_PLACEMENT_3D('',#47750,#29541,#29542);
#25172=AXIS2_PLACEMENT_3D('',#47751,#29543,#29544);
#25173=AXIS2_PLACEMENT_3D('',#47752,#29545,#29546);
#25174=AXIS2_PLACEMENT_3D('',#47753,#29547,#29548);
#25175=AXIS2_PLACEMENT_3D('',#47754,#29549,#29550);
#25176=AXIS2_PLACEMENT_3D('',#47755,#29551,#29552);
#25177=AXIS2_PLACEMENT_3D('',#47756,#29553,#29554);
#25178=AXIS2_PLACEMENT_3D('',#47757,#29555,#29556);
#25179=AXIS2_PLACEMENT_3D('',#47758,#29557,#29558);
#25180=AXIS2_PLACEMENT_3D('',#47759,#29559,#29560);
#25181=AXIS2_PLACEMENT_3D('',#47760,#29561,#29562);
#25182=AXIS2_PLACEMENT_3D('',#47761,#29563,#29564);
#25183=AXIS2_PLACEMENT_3D('',#47762,#29565,#29566);
#25184=AXIS2_PLACEMENT_3D('',#47763,#29567,#29568);
#25185=AXIS2_PLACEMENT_3D('',#47764,#29569,#29570);
#25186=AXIS2_PLACEMENT_3D('',#47765,#29571,#29572);
#25187=AXIS2_PLACEMENT_3D('',#47766,#29573,#29574);
#25188=AXIS2_PLACEMENT_3D('',#47767,#29575,#29576);
#25189=AXIS2_PLACEMENT_3D('',#47768,#29577,#29578);
#25190=AXIS2_PLACEMENT_3D('',#47769,#29579,#29580);
#25191=AXIS2_PLACEMENT_3D('',#47770,#29581,#29582);
#25192=AXIS2_PLACEMENT_3D('',#47771,#29583,#29584);
#25193=AXIS2_PLACEMENT_3D('',#47772,#29585,#29586);
#25194=AXIS2_PLACEMENT_3D('',#47773,#29587,#29588);
#25195=AXIS2_PLACEMENT_3D('',#47774,#29589,#29590);
#25196=AXIS2_PLACEMENT_3D('',#47775,#29591,#29592);
#25197=AXIS2_PLACEMENT_3D('',#47776,#29593,#29594);
#25198=AXIS2_PLACEMENT_3D('',#47777,#29595,#29596);
#25199=AXIS2_PLACEMENT_3D('',#47778,#29597,#29598);
#25200=AXIS2_PLACEMENT_3D('',#47779,#29599,#29600);
#25201=AXIS2_PLACEMENT_3D('',#47780,#29601,#29602);
#25202=AXIS2_PLACEMENT_3D('',#47781,#29603,#29604);
#25203=AXIS2_PLACEMENT_3D('',#47782,#29605,#29606);
#25204=AXIS2_PLACEMENT_3D('',#47784,#29607,#29608);
#25205=AXIS2_PLACEMENT_3D('',#47787,#29610,#29611);
#25206=AXIS2_PLACEMENT_3D('',#47788,#29612,#29613);
#25207=AXIS2_PLACEMENT_3D('',#47789,#29614,#29615);
#25208=AXIS2_PLACEMENT_3D('',#47791,#29616,#29617);
#25209=AXIS2_PLACEMENT_3D('',#47794,#29619,#29620);
#25210=AXIS2_PLACEMENT_3D('',#47795,#29621,#29622);
#25211=AXIS2_PLACEMENT_3D('',#47796,#29623,#29624);
#25212=AXIS2_PLACEMENT_3D('',#47798,#29625,#29626);
#25213=AXIS2_PLACEMENT_3D('',#47801,#29628,#29629);
#25214=AXIS2_PLACEMENT_3D('',#47802,#29630,#29631);
#25215=AXIS2_PLACEMENT_3D('',#47803,#29632,#29633);
#25216=AXIS2_PLACEMENT_3D('',#47805,#29634,#29635);
#25217=AXIS2_PLACEMENT_3D('',#47808,#29637,#29638);
#25218=AXIS2_PLACEMENT_3D('',#47809,#29639,#29640);
#25219=AXIS2_PLACEMENT_3D('',#47810,#29641,#29642);
#25220=AXIS2_PLACEMENT_3D('',#47812,#29643,#29644);
#25221=AXIS2_PLACEMENT_3D('',#47815,#29646,#29647);
#25222=AXIS2_PLACEMENT_3D('',#47816,#29648,#29649);
#25223=AXIS2_PLACEMENT_3D('',#47817,#29650,#29651);
#25224=AXIS2_PLACEMENT_3D('',#47819,#29652,#29653);
#25225=AXIS2_PLACEMENT_3D('',#47822,#29655,#29656);
#25226=AXIS2_PLACEMENT_3D('',#47823,#29657,#29658);
#25227=AXIS2_PLACEMENT_3D('',#47824,#29659,#29660);
#25228=AXIS2_PLACEMENT_3D('',#47826,#29661,#29662);
#25229=AXIS2_PLACEMENT_3D('',#47829,#29664,#29665);
#25230=AXIS2_PLACEMENT_3D('',#47830,#29666,#29667);
#25231=AXIS2_PLACEMENT_3D('',#47831,#29668,#29669);
#25232=AXIS2_PLACEMENT_3D('',#47833,#29670,#29671);
#25233=AXIS2_PLACEMENT_3D('',#47836,#29673,#29674);
#25234=AXIS2_PLACEMENT_3D('',#47837,#29675,#29676);
#25235=AXIS2_PLACEMENT_3D('',#47838,#29677,#29678);
#25236=AXIS2_PLACEMENT_3D('',#47840,#29679,#29680);
#25237=AXIS2_PLACEMENT_3D('',#47843,#29682,#29683);
#25238=AXIS2_PLACEMENT_3D('',#47844,#29684,#29685);
#25239=AXIS2_PLACEMENT_3D('',#47846,#29686,#29687);
#25240=AXIS2_PLACEMENT_3D('',#47847,#29688,#29689);
#25241=AXIS2_PLACEMENT_3D('',#47849,#29690,#29691);
#25242=AXIS2_PLACEMENT_3D('',#47852,#29693,#29694);
#25243=AXIS2_PLACEMENT_3D('',#47853,#29695,#29696);
#25244=AXIS2_PLACEMENT_3D('',#47855,#29697,#29698);
#25245=AXIS2_PLACEMENT_3D('',#47856,#29699,#29700);
#25246=AXIS2_PLACEMENT_3D('',#47858,#29701,#29702);
#25247=AXIS2_PLACEMENT_3D('',#47861,#29704,#29705);
#25248=AXIS2_PLACEMENT_3D('',#47862,#29706,#29707);
#25249=AXIS2_PLACEMENT_3D('',#47864,#29708,#29709);
#25250=AXIS2_PLACEMENT_3D('',#47865,#29710,#29711);
#25251=AXIS2_PLACEMENT_3D('',#47867,#29712,#29713);
#25252=AXIS2_PLACEMENT_3D('',#47870,#29715,#29716);
#25253=AXIS2_PLACEMENT_3D('',#47871,#29717,#29718);
#25254=AXIS2_PLACEMENT_3D('',#47873,#29719,#29720);
#25255=AXIS2_PLACEMENT_3D('',#47874,#29721,#29722);
#25256=AXIS2_PLACEMENT_3D('',#47876,#29723,#29724);
#25257=AXIS2_PLACEMENT_3D('',#47878,#29726,#29727);
#25258=AXIS2_PLACEMENT_3D('',#47880,#29728,#29729);
#25259=AXIS2_PLACEMENT_3D('',#47882,#29731,#29732);
#25260=AXIS2_PLACEMENT_3D('',#47884,#29733,#29734);
#25261=AXIS2_PLACEMENT_3D('',#47886,#29736,#29737);
#25262=AXIS2_PLACEMENT_3D('',#47888,#29738,#29739);
#25263=AXIS2_PLACEMENT_3D('',#47890,#29741,#29742);
#25264=AXIS2_PLACEMENT_3D('',#47892,#29743,#29744);
#25265=AXIS2_PLACEMENT_3D('',#47895,#29746,#29747);
#25266=AXIS2_PLACEMENT_3D('',#47896,#29748,#29749);
#25267=AXIS2_PLACEMENT_3D('',#47898,#29750,#29751);
#25268=AXIS2_PLACEMENT_3D('',#47901,#29753,#29754);
#25269=AXIS2_PLACEMENT_3D('',#47902,#29755,#29756);
#25270=AXIS2_PLACEMENT_3D('',#47904,#29757,#29758);
#25271=AXIS2_PLACEMENT_3D('',#47907,#29760,#29761);
#25272=AXIS2_PLACEMENT_3D('',#47908,#29762,#29763);
#25273=AXIS2_PLACEMENT_3D('',#47910,#29764,#29765);
#25274=AXIS2_PLACEMENT_3D('',#47913,#29767,#29768);
#25275=AXIS2_PLACEMENT_3D('',#47914,#29769,#29770);
#25276=AXIS2_PLACEMENT_3D('',#47916,#29771,#29772);
#25277=AXIS2_PLACEMENT_3D('',#47919,#29774,#29775);
#25278=AXIS2_PLACEMENT_3D('',#47920,#29776,#29777);
#25279=AXIS2_PLACEMENT_3D('',#47922,#29778,#29779);
#25280=AXIS2_PLACEMENT_3D('',#47925,#29781,#29782);
#25281=AXIS2_PLACEMENT_3D('',#47926,#29783,#29784);
#25282=AXIS2_PLACEMENT_3D('',#47928,#29785,#29786);
#25283=AXIS2_PLACEMENT_3D('',#47931,#29788,#29789);
#25284=AXIS2_PLACEMENT_3D('',#47932,#29790,#29791);
#25285=AXIS2_PLACEMENT_3D('',#47934,#29792,#29793);
#25286=AXIS2_PLACEMENT_3D('',#47937,#29795,#29796);
#25287=AXIS2_PLACEMENT_3D('',#47938,#29797,#29798);
#25288=AXIS2_PLACEMENT_3D('',#47940,#29799,#29800);
#25289=AXIS2_PLACEMENT_3D('',#47943,#29802,#29803);
#25290=AXIS2_PLACEMENT_3D('',#47944,#29804,#29805);
#25291=AXIS2_PLACEMENT_3D('',#47946,#29806,#29807);
#25292=AXIS2_PLACEMENT_3D('',#47949,#29809,#29810);
#25293=AXIS2_PLACEMENT_3D('',#47950,#29811,#29812);
#25294=AXIS2_PLACEMENT_3D('',#47959,#29817,#29818);
#25295=AXIS2_PLACEMENT_3D('',#47965,#29822,#29823);
#25296=AXIS2_PLACEMENT_3D('',#47971,#29827,#29828);
#25297=AXIS2_PLACEMENT_3D('',#47974,#29831,#29832);
#25298=AXIS2_PLACEMENT_3D('',#47975,#29833,#29834);
#25299=AXIS2_PLACEMENT_3D('',#47976,#29835,#29836);
#25300=AXIS2_PLACEMENT_3D('',#47977,#29837,#29838);
#25301=AXIS2_PLACEMENT_3D('',#47982,#29840,#29841);
#25302=AXIS2_PLACEMENT_3D('',#47985,#29843,#29844);
#25303=AXIS2_PLACEMENT_3D('',#47986,#29845,#29846);
#25304=AXIS2_PLACEMENT_3D('',#47991,#29848,#29849);
#25305=AXIS2_PLACEMENT_3D('',#47994,#29851,#29852);
#25306=AXIS2_PLACEMENT_3D('',#47995,#29853,#29854);
#25307=AXIS2_PLACEMENT_3D('',#47997,#29855,#29856);
#25308=AXIS2_PLACEMENT_3D('',#48000,#29858,#29859);
#25309=AXIS2_PLACEMENT_3D('',#48001,#29860,#29861);
#25310=AXIS2_PLACEMENT_3D('',#48003,#29862,#29863);
#25311=AXIS2_PLACEMENT_3D('',#48006,#29865,#29866);
#25312=AXIS2_PLACEMENT_3D('',#48007,#29867,#29868);
#25313=AXIS2_PLACEMENT_3D('',#48009,#29869,#29870);
#25314=AXIS2_PLACEMENT_3D('',#48012,#29872,#29873);
#25315=AXIS2_PLACEMENT_3D('',#48013,#29874,#29875);
#25316=AXIS2_PLACEMENT_3D('',#48015,#29876,#29877);
#25317=AXIS2_PLACEMENT_3D('',#48018,#29879,#29880);
#25318=AXIS2_PLACEMENT_3D('',#48019,#29881,#29882);
#25319=AXIS2_PLACEMENT_3D('',#48021,#29883,#29884);
#25320=AXIS2_PLACEMENT_3D('',#48024,#29886,#29887);
#25321=AXIS2_PLACEMENT_3D('',#48025,#29888,#29889);
#25322=AXIS2_PLACEMENT_3D('',#48027,#29890,#29891);
#25323=AXIS2_PLACEMENT_3D('',#48028,#29892,#29893);
#25324=AXIS2_PLACEMENT_3D('',#48029,#29894,#29895);
#25325=AXIS2_PLACEMENT_3D('',#48031,#29897,#29898);
#25326=AXIS2_PLACEMENT_3D('',#48032,#29899,#29900);
#25327=AXIS2_PLACEMENT_3D('',#48034,#29901,#29902);
#25328=AXIS2_PLACEMENT_3D('',#48035,#29903,#29904);
#25329=AXIS2_PLACEMENT_3D('',#48037,#29905,#29906);
#25330=AXIS2_PLACEMENT_3D('',#48040,#29908,#29909);
#25331=AXIS2_PLACEMENT_3D('',#48041,#29910,#29911);
#25332=AXIS2_PLACEMENT_3D('',#48043,#29912,#29913);
#25333=AXIS2_PLACEMENT_3D('',#48044,#29914,#29915);
#25334=AXIS2_PLACEMENT_3D('',#48045,#29916,#29917);
#25335=AXIS2_PLACEMENT_3D('',#48047,#29919,#29920);
#25336=AXIS2_PLACEMENT_3D('',#48048,#29921,#29922);
#25337=AXIS2_PLACEMENT_3D('',#48050,#29923,#29924);
#25338=AXIS2_PLACEMENT_3D('',#48051,#29925,#29926);
#25339=AXIS2_PLACEMENT_3D('',#48062,#29933,#29934);
#25340=AXIS2_PLACEMENT_3D('',#48064,#29935,#29936);
#25341=AXIS2_PLACEMENT_3D('',#48066,#29938,#29939);
#25342=AXIS2_PLACEMENT_3D('',#48068,#29940,#29941);
#25343=AXIS2_PLACEMENT_3D('',#48070,#29943,#29944);
#25344=AXIS2_PLACEMENT_3D('',#48072,#29945,#29946);
#25345=AXIS2_PLACEMENT_3D('',#48074,#29948,#29949);
#25346=AXIS2_PLACEMENT_3D('',#48076,#29950,#29951);
#25347=AXIS2_PLACEMENT_3D('',#48078,#29953,#29954);
#25348=AXIS2_PLACEMENT_3D('',#48084,#29958,#29959);
#25349=AXIS2_PLACEMENT_3D('',#48088,#29962,#29963);
#25350=AXIS2_PLACEMENT_3D('',#48092,#29966,#29967);
#25351=AXIS2_PLACEMENT_3D('',#48094,#29969,#29970);
#25352=AXIS2_PLACEMENT_3D('',#48095,#29971,#29972);
#25353=AXIS2_PLACEMENT_3D('',#48096,#29973,#29974);
#25354=AXIS2_PLACEMENT_3D('',#48098,#29975,#29976);
#25355=AXIS2_PLACEMENT_3D('',#48101,#29978,#29979);
#25356=AXIS2_PLACEMENT_3D('',#48102,#29980,#29981);
#25357=AXIS2_PLACEMENT_3D('',#48104,#29982,#29983);
#25358=AXIS2_PLACEMENT_3D('',#48107,#29985,#29986);
#25359=AXIS2_PLACEMENT_3D('',#48108,#29987,#29988);
#25360=AXIS2_PLACEMENT_3D('',#48110,#29989,#29990);
#25361=AXIS2_PLACEMENT_3D('',#48113,#29992,#29993);
#25362=AXIS2_PLACEMENT_3D('',#48114,#29994,#29995);
#25363=AXIS2_PLACEMENT_3D('',#48116,#29996,#29997);
#25364=AXIS2_PLACEMENT_3D('',#48119,#29999,#30000);
#25365=AXIS2_PLACEMENT_3D('',#48120,#30001,#30002);
#25366=AXIS2_PLACEMENT_3D('',#48122,#30003,#30004);
#25367=AXIS2_PLACEMENT_3D('',#48123,#30005,#30006);
#25368=AXIS2_PLACEMENT_3D('',#48126,#30008,#30009);
#25369=AXIS2_PLACEMENT_3D('',#48127,#30010,#30011);
#25370=AXIS2_PLACEMENT_3D('',#48129,#30012,#30013);
#25371=AXIS2_PLACEMENT_3D('',#48132,#30015,#30016);
#25372=AXIS2_PLACEMENT_3D('',#48133,#30017,#30018);
#25373=AXIS2_PLACEMENT_3D('',#48134,#30019,#30020);
#25374=AXIS2_PLACEMENT_3D('',#48136,#30021,#30022);
#25375=AXIS2_PLACEMENT_3D('',#48139,#30024,#30025);
#25376=AXIS2_PLACEMENT_3D('',#48140,#30026,#30027);
#25377=AXIS2_PLACEMENT_3D('',#48141,#30028,#30029);
#25378=AXIS2_PLACEMENT_3D('',#48150,#30034,#30035);
#25379=AXIS2_PLACEMENT_3D('',#48156,#30039,#30040);
#25380=AXIS2_PLACEMENT_3D('',#48162,#30044,#30045);
#25381=AXIS2_PLACEMENT_3D('',#48165,#30048,#30049);
#25382=AXIS2_PLACEMENT_3D('',#48166,#30050,#30051);
#25383=AXIS2_PLACEMENT_3D('',#48167,#30052,#30053);
#25384=AXIS2_PLACEMENT_3D('',#48168,#30054,#30055);
#25385=AXIS2_PLACEMENT_3D('',#48170,#30056,#30057);
#25386=AXIS2_PLACEMENT_3D('',#48173,#30059,#30060);
#25387=AXIS2_PLACEMENT_3D('',#48174,#30061,#30062);
#25388=AXIS2_PLACEMENT_3D('',#48176,#30063,#30064);
#25389=AXIS2_PLACEMENT_3D('',#48179,#30066,#30067);
#25390=AXIS2_PLACEMENT_3D('',#48180,#30068,#30069);
#25391=AXIS2_PLACEMENT_3D('',#48182,#30070,#30071);
#25392=AXIS2_PLACEMENT_3D('',#48185,#30073,#30074);
#25393=AXIS2_PLACEMENT_3D('',#48186,#30075,#30076);
#25394=AXIS2_PLACEMENT_3D('',#48188,#30077,#30078);
#25395=AXIS2_PLACEMENT_3D('',#48191,#30080,#30081);
#25396=AXIS2_PLACEMENT_3D('',#48192,#30082,#30083);
#25397=AXIS2_PLACEMENT_3D('',#48194,#30084,#30085);
#25398=AXIS2_PLACEMENT_3D('',#48195,#30086,#30087);
#25399=AXIS2_PLACEMENT_3D('',#48198,#30089,#30090);
#25400=AXIS2_PLACEMENT_3D('',#48199,#30091,#30092);
#25401=AXIS2_PLACEMENT_3D('',#48201,#30093,#30094);
#25402=AXIS2_PLACEMENT_3D('',#48204,#30096,#30097);
#25403=AXIS2_PLACEMENT_3D('',#48205,#30098,#30099);
#25404=AXIS2_PLACEMENT_3D('',#48206,#30100,#30101);
#25405=AXIS2_PLACEMENT_3D('',#48207,#30102,#30103);
#25406=AXIS2_PLACEMENT_3D('',#48208,#30104,#30105);
#25407=AXIS2_PLACEMENT_3D('',#48210,#30106,#30107);
#25408=AXIS2_PLACEMENT_3D('',#48213,#30109,#30110);
#25409=AXIS2_PLACEMENT_3D('',#48214,#30111,#30112);
#25410=AXIS2_PLACEMENT_3D('',#48216,#30113,#30114);
#25411=AXIS2_PLACEMENT_3D('',#48219,#30116,#30117);
#25412=AXIS2_PLACEMENT_3D('',#48220,#30118,#30119);
#25413=AXIS2_PLACEMENT_3D('',#48222,#30120,#30121);
#25414=AXIS2_PLACEMENT_3D('',#48225,#30123,#30124);
#25415=AXIS2_PLACEMENT_3D('',#48226,#30125,#30126);
#25416=AXIS2_PLACEMENT_3D('',#48228,#30127,#30128);
#25417=AXIS2_PLACEMENT_3D('',#48231,#30130,#30131);
#25418=AXIS2_PLACEMENT_3D('',#48232,#30132,#30133);
#25419=AXIS2_PLACEMENT_3D('',#48234,#30134,#30135);
#25420=AXIS2_PLACEMENT_3D('',#48235,#30136,#30137);
#25421=AXIS2_PLACEMENT_3D('',#48237,#30138,#30139);
#25422=AXIS2_PLACEMENT_3D('',#48239,#30141,#30142);
#25423=AXIS2_PLACEMENT_3D('',#48241,#30143,#30144);
#25424=AXIS2_PLACEMENT_3D('',#48244,#30146,#30147);
#25425=AXIS2_PLACEMENT_3D('',#48245,#30148,#30149);
#25426=AXIS2_PLACEMENT_3D('',#48246,#30150,#30151);
#25427=AXIS2_PLACEMENT_3D('',#48248,#30152,#30153);
#25428=AXIS2_PLACEMENT_3D('',#48251,#30155,#30156);
#25429=AXIS2_PLACEMENT_3D('',#48252,#30157,#30158);
#25430=AXIS2_PLACEMENT_3D('',#48253,#30159,#30160);
#25431=AXIS2_PLACEMENT_3D('',#48262,#30165,#30166);
#25432=AXIS2_PLACEMENT_3D('',#48268,#30170,#30171);
#25433=AXIS2_PLACEMENT_3D('',#48274,#30175,#30176);
#25434=AXIS2_PLACEMENT_3D('',#48277,#30179,#30180);
#25435=AXIS2_PLACEMENT_3D('',#48278,#30181,#30182);
#25436=AXIS2_PLACEMENT_3D('',#48279,#30183,#30184);
#25437=AXIS2_PLACEMENT_3D('',#48280,#30185,#30186);
#25438=AXIS2_PLACEMENT_3D('',#48282,#30187,#30188);
#25439=AXIS2_PLACEMENT_3D('',#48285,#30190,#30191);
#25440=AXIS2_PLACEMENT_3D('',#48286,#30192,#30193);
#25441=AXIS2_PLACEMENT_3D('',#48288,#30194,#30195);
#25442=AXIS2_PLACEMENT_3D('',#48291,#30197,#30198);
#25443=AXIS2_PLACEMENT_3D('',#48292,#30199,#30200);
#25444=AXIS2_PLACEMENT_3D('',#48294,#30201,#30202);
#25445=AXIS2_PLACEMENT_3D('',#48297,#30204,#30205);
#25446=AXIS2_PLACEMENT_3D('',#48298,#30206,#30207);
#25447=AXIS2_PLACEMENT_3D('',#48307,#30212,#30213);
#25448=AXIS2_PLACEMENT_3D('',#48308,#30214,#30215);
#25449=AXIS2_PLACEMENT_3D('',#48310,#30216,#30217);
#25450=AXIS2_PLACEMENT_3D('',#48311,#30218,#30219);
#25451=AXIS2_PLACEMENT_3D('',#48312,#30220,#30221);
#25452=AXIS2_PLACEMENT_3D('',#48313,#30222,#30223);
#25453=AXIS2_PLACEMENT_3D('',#48316,#30225,#30226);
#25454=AXIS2_PLACEMENT_3D('',#48317,#30227,#30228);
#25455=AXIS2_PLACEMENT_3D('',#48319,#30229,#30230);
#25456=AXIS2_PLACEMENT_3D('',#48320,#30231,#30232);
#25457=AXIS2_PLACEMENT_3D('',#48322,#30233,#30234);
#25458=AXIS2_PLACEMENT_3D('',#48324,#30236,#30237);
#25459=AXIS2_PLACEMENT_3D('',#48325,#30238,#30239);
#25460=AXIS2_PLACEMENT_3D('',#48326,#30240,#30241);
#25461=AXIS2_PLACEMENT_3D('',#48328,#30242,#30243);
#25462=AXIS2_PLACEMENT_3D('',#48331,#30245,#30246);
#25463=AXIS2_PLACEMENT_3D('',#48332,#30247,#30248);
#25464=AXIS2_PLACEMENT_3D('',#48334,#30249,#30250);
#25465=AXIS2_PLACEMENT_3D('',#48335,#30251,#30252);
#25466=AXIS2_PLACEMENT_3D('',#48337,#30253,#30254);
#25467=AXIS2_PLACEMENT_3D('',#48339,#30256,#30257);
#25468=AXIS2_PLACEMENT_3D('',#48348,#30262,#30263);
#25469=AXIS2_PLACEMENT_3D('',#48354,#30267,#30268);
#25470=AXIS2_PLACEMENT_3D('',#48360,#30272,#30273);
#25471=AXIS2_PLACEMENT_3D('',#48363,#30276,#30277);
#25472=AXIS2_PLACEMENT_3D('',#48364,#30278,#30279);
#25473=AXIS2_PLACEMENT_3D('',#48365,#30280,#30281);
#25474=AXIS2_PLACEMENT_3D('',#48366,#30282,#30283);
#25475=AXIS2_PLACEMENT_3D('',#48368,#30284,#30285);
#25476=AXIS2_PLACEMENT_3D('',#48371,#30287,#30288);
#25477=AXIS2_PLACEMENT_3D('',#48372,#30289,#30290);
#25478=AXIS2_PLACEMENT_3D('',#48374,#30291,#30292);
#25479=AXIS2_PLACEMENT_3D('',#48375,#30293,#30294);
#25480=AXIS2_PLACEMENT_3D('',#48377,#30295,#30296);
#25481=AXIS2_PLACEMENT_3D('',#48379,#30298,#30299);
#25482=AXIS2_PLACEMENT_3D('',#48388,#30304,#30305);
#25483=AXIS2_PLACEMENT_3D('',#48394,#30309,#30310);
#25484=AXIS2_PLACEMENT_3D('',#48400,#30314,#30315);
#25485=AXIS2_PLACEMENT_3D('',#48403,#30318,#30319);
#25486=AXIS2_PLACEMENT_3D('',#48404,#30320,#30321);
#25487=AXIS2_PLACEMENT_3D('',#48405,#30322,#30323);
#25488=AXIS2_PLACEMENT_3D('',#48406,#30324,#30325);
#25489=AXIS2_PLACEMENT_3D('',#48408,#30326,#30327);
#25490=AXIS2_PLACEMENT_3D('',#48411,#30329,#30330);
#25491=AXIS2_PLACEMENT_3D('',#48412,#30331,#30332);
#25492=AXIS2_PLACEMENT_3D('',#48414,#30333,#30334);
#25493=AXIS2_PLACEMENT_3D('',#48415,#30335,#30336);
#25494=AXIS2_PLACEMENT_3D('',#48417,#30337,#30338);
#25495=AXIS2_PLACEMENT_3D('',#48420,#30340,#30341);
#25496=AXIS2_PLACEMENT_3D('',#48421,#30342,#30343);
#25497=AXIS2_PLACEMENT_3D('',#48423,#30344,#30345);
#25498=AXIS2_PLACEMENT_3D('',#48424,#30346,#30347);
#25499=AXIS2_PLACEMENT_3D('',#48426,#30348,#30349);
#25500=AXIS2_PLACEMENT_3D('',#48429,#30351,#30352);
#25501=AXIS2_PLACEMENT_3D('',#48430,#30353,#30354);
#25502=AXIS2_PLACEMENT_3D('',#48432,#30355,#30356);
#25503=AXIS2_PLACEMENT_3D('',#48433,#30357,#30358);
#25504=AXIS2_PLACEMENT_3D('',#48435,#30359,#30360);
#25505=AXIS2_PLACEMENT_3D('',#48438,#30362,#30363);
#25506=AXIS2_PLACEMENT_3D('',#48439,#30364,#30365);
#25507=AXIS2_PLACEMENT_3D('',#48441,#30366,#30367);
#25508=AXIS2_PLACEMENT_3D('',#48442,#30368,#30369);
#25509=AXIS2_PLACEMENT_3D('',#48444,#30370,#30371);
#25510=AXIS2_PLACEMENT_3D('',#48446,#30373,#30374);
#25511=AXIS2_PLACEMENT_3D('',#48448,#30375,#30376);
#25512=AXIS2_PLACEMENT_3D('',#48450,#30378,#30379);
#25513=AXIS2_PLACEMENT_3D('',#48452,#30380,#30381);
#25514=AXIS2_PLACEMENT_3D('',#48454,#30383,#30384);
#25515=AXIS2_PLACEMENT_3D('',#48456,#30385,#30386);
#25516=AXIS2_PLACEMENT_3D('',#48458,#30388,#30389);
#25517=AXIS2_PLACEMENT_3D('',#48467,#30394,#30395);
#25518=AXIS2_PLACEMENT_3D('',#48473,#30399,#30400);
#25519=AXIS2_PLACEMENT_3D('',#48479,#30404,#30405);
#25520=AXIS2_PLACEMENT_3D('',#48485,#30409,#30410);
#25521=AXIS2_PLACEMENT_3D('',#48491,#30414,#30415);
#25522=AXIS2_PLACEMENT_3D('',#48497,#30419,#30420);
#25523=AXIS2_PLACEMENT_3D('',#48503,#30424,#30425);
#25524=AXIS2_PLACEMENT_3D('',#48509,#30429,#30430);
#25525=AXIS2_PLACEMENT_3D('',#48515,#30434,#30435);
#25526=AXIS2_PLACEMENT_3D('',#48521,#30439,#30440);
#25527=AXIS2_PLACEMENT_3D('',#48527,#30444,#30445);
#25528=AXIS2_PLACEMENT_3D('',#48530,#30448,#30449);
#25529=AXIS2_PLACEMENT_3D('',#48531,#30450,#30451);
#25530=AXIS2_PLACEMENT_3D('',#48532,#30452,#30453);
#25531=AXIS2_PLACEMENT_3D('',#48533,#30454,#30455);
#25532=AXIS2_PLACEMENT_3D('',#48534,#30456,#30457);
#25533=AXIS2_PLACEMENT_3D('',#48537,#30458,#30459);
#25534=AXIS2_PLACEMENT_3D('',#48538,#30460,#30461);
#25535=AXIS2_PLACEMENT_3D('',#48540,#30462,#30463);
#25536=AXIS2_PLACEMENT_3D('',#48542,#30464,#30465);
#25537=AXIS2_PLACEMENT_3D('',#48543,#30466,#30467);
#25538=AXIS2_PLACEMENT_3D('',#48544,#30468,#30469);
#25539=AXIS2_PLACEMENT_3D('',#48547,#30471,#30472);
#25540=AXIS2_PLACEMENT_3D('',#48548,#30473,#30474);
#25541=AXIS2_PLACEMENT_3D('',#48550,#30475,#30476);
#25542=AXIS2_PLACEMENT_3D('',#48553,#30478,#30479);
#25543=AXIS2_PLACEMENT_3D('',#48554,#30480,#30481);
#25544=AXIS2_PLACEMENT_3D('',#48557,#30483,#30484);
#25545=AXIS2_PLACEMENT_3D('',#48558,#30485,#30486);
#25546=AXIS2_PLACEMENT_3D('',#48559,#30487,#30488);
#25547=AXIS2_PLACEMENT_3D('',#48561,#30489,#30490);
#25548=AXIS2_PLACEMENT_3D('',#48563,#30492,#30493);
#25549=AXIS2_PLACEMENT_3D('',#48565,#30494,#30495);
#25550=AXIS2_PLACEMENT_3D('',#48566,#30496,#30497);
#25551=AXIS2_PLACEMENT_3D('',#48568,#30499,#30500);
#25552=AXIS2_PLACEMENT_3D('',#48569,#30501,#30502);
#25553=AXIS2_PLACEMENT_3D('',#48572,#30503,#30504);
#25554=AXIS2_PLACEMENT_3D('',#48573,#30505,#30506);
#25555=AXIS2_PLACEMENT_3D('',#48575,#30507,#30508);
#25556=AXIS2_PLACEMENT_3D('',#48577,#30509,#30510);
#25557=AXIS2_PLACEMENT_3D('',#48578,#30511,#30512);
#25558=AXIS2_PLACEMENT_3D('',#48579,#30513,#30514);
#25559=AXIS2_PLACEMENT_3D('',#48581,#30515,#30516);
#25560=AXIS2_PLACEMENT_3D('',#48583,#30518,#30519);
#25561=AXIS2_PLACEMENT_3D('',#48585,#30520,#30521);
#25562=AXIS2_PLACEMENT_3D('',#48587,#30522,#30523);
#25563=AXIS2_PLACEMENT_3D('',#48588,#30524,#30525);
#25564=AXIS2_PLACEMENT_3D('',#48590,#30526,#30527);
#25565=AXIS2_PLACEMENT_3D('',#48592,#30529,#30530);
#25566=AXIS2_PLACEMENT_3D('',#48594,#30531,#30532);
#25567=AXIS2_PLACEMENT_3D('',#48596,#30534,#30535);
#25568=AXIS2_PLACEMENT_3D('',#48598,#30536,#30537);
#25569=AXIS2_PLACEMENT_3D('',#48600,#30539,#30540);
#25570=AXIS2_PLACEMENT_3D('',#48601,#30541,#30542);
#25571=AXIS2_PLACEMENT_3D('',#48603,#30544,#30545);
#25572=AXIS2_PLACEMENT_3D('',#48604,#30546,#30547);
#25573=AXIS2_PLACEMENT_3D('',#48607,#30548,#30549);
#25574=AXIS2_PLACEMENT_3D('',#48608,#30550,#30551);
#25575=AXIS2_PLACEMENT_3D('',#48611,#30552,#30553);
#25576=AXIS2_PLACEMENT_3D('',#48612,#30554,#30555);
#25577=AXIS2_PLACEMENT_3D('',#48615,#30556,#30557);
#25578=AXIS2_PLACEMENT_3D('',#48616,#30558,#30559);
#25579=AXIS2_PLACEMENT_3D('',#48619,#30560,#30561);
#25580=AXIS2_PLACEMENT_3D('',#48620,#30562,#30563);
#25581=AXIS2_PLACEMENT_3D('',#48623,#30564,#30565);
#25582=AXIS2_PLACEMENT_3D('',#48624,#30566,#30567);
#25583=AXIS2_PLACEMENT_3D('',#48627,#30568,#30569);
#25584=AXIS2_PLACEMENT_3D('',#48628,#30570,#30571);
#25585=AXIS2_PLACEMENT_3D('',#48631,#30572,#30573);
#25586=AXIS2_PLACEMENT_3D('',#48632,#30574,#30575);
#25587=AXIS2_PLACEMENT_3D('',#48633,#30576,#30577);
#25588=AXIS2_PLACEMENT_3D('',#48659,#30578,#30579);
#25589=AXIS2_PLACEMENT_3D('',#48683,#30580,#30581);
#25590=AXIS2_PLACEMENT_3D('',#48684,#30582,#30583);
#25591=AXIS2_PLACEMENT_3D('',#48686,#30584,#30585);
#25592=AXIS2_PLACEMENT_3D('',#48711,#30586,#30587);
#25593=AXIS2_PLACEMENT_3D('',#48736,#30588,#30589);
#25594=AXIS2_PLACEMENT_3D('',#48739,#30591,#30592);
#25595=AXIS2_PLACEMENT_3D('',#48741,#30593,#30594);
#25596=AXIS2_PLACEMENT_3D('',#48766,#30595,#30596);
#25597=AXIS2_PLACEMENT_3D('',#48791,#30597,#30598);
#25598=AXIS2_PLACEMENT_3D('',#48816,#30599,#30600);
#25599=AXIS2_PLACEMENT_3D('',#48840,#30601,#30602);
#25600=AXIS2_PLACEMENT_3D('',#48841,#30603,#30604);
#25601=AXIS2_PLACEMENT_3D('',#48843,#30605,#30606);
#25602=AXIS2_PLACEMENT_3D('',#48844,#30607,#30608);
#25603=AXIS2_PLACEMENT_3D('',#48845,#30609,#30610);
#25604=AXIS2_PLACEMENT_3D('',#48869,#30611,#30612);
#25605=AXIS2_PLACEMENT_3D('',#48870,#30613,#30614);
#25606=AXIS2_PLACEMENT_3D('',#48872,#30615,#30616);
#25607=AXIS2_PLACEMENT_3D('',#48873,#30617,#30618);
#25608=AXIS2_PLACEMENT_3D('',#48874,#30619,#30620);
#25609=AXIS2_PLACEMENT_3D('',#48898,#30621,#30622);
#25610=AXIS2_PLACEMENT_3D('',#48899,#30623,#30624);
#25611=AXIS2_PLACEMENT_3D('',#48901,#30625,#30626);
#25612=AXIS2_PLACEMENT_3D('',#48903,#30627,#30628);
#25613=AXIS2_PLACEMENT_3D('',#48904,#30629,#30630);
#25614=AXIS2_PLACEMENT_3D('',#48905,#30631,#30632);
#25615=AXIS2_PLACEMENT_3D('',#48929,#30633,#30634);
#25616=AXIS2_PLACEMENT_3D('',#48930,#30635,#30636);
#25617=AXIS2_PLACEMENT_3D('',#48932,#30637,#30638);
#25618=AXIS2_PLACEMENT_3D('',#48933,#30639,#30640);
#25619=AXIS2_PLACEMENT_3D('',#48934,#30641,#30642);
#25620=AXIS2_PLACEMENT_3D('',#48958,#30643,#30644);
#25621=AXIS2_PLACEMENT_3D('',#48959,#30645,#30646);
#25622=AXIS2_PLACEMENT_3D('',#48961,#30647,#30648);
#25623=AXIS2_PLACEMENT_3D('',#48962,#30649,#30650);
#25624=AXIS2_PLACEMENT_3D('',#48963,#30651,#30652);
#25625=AXIS2_PLACEMENT_3D('',#48987,#30653,#30654);
#25626=AXIS2_PLACEMENT_3D('',#48988,#30655,#30656);
#25627=AXIS2_PLACEMENT_3D('',#48990,#30657,#30658);
#25628=AXIS2_PLACEMENT_3D('',#48993,#30660,#30661);
#25629=AXIS2_PLACEMENT_3D('',#49017,#30662,#30663);
#25630=AXIS2_PLACEMENT_3D('',#49018,#30664,#30665);
#25631=AXIS2_PLACEMENT_3D('',#49019,#30666,#30667);
#25632=AXIS2_PLACEMENT_3D('',#49020,#30668,#30669);
#25633=AXIS2_PLACEMENT_3D('',#49021,#30670,#30671);
#25634=AXIS2_PLACEMENT_3D('',#49022,#30672,#30673);
#25635=AXIS2_PLACEMENT_3D('',#49023,#30674,#30675);
#25636=AXIS2_PLACEMENT_3D('',#49024,#30676,#30677);
#25637=AXIS2_PLACEMENT_3D('',#49025,#30678,#30679);
#25638=AXIS2_PLACEMENT_3D('',#49027,#30680,#30681);
#25639=AXIS2_PLACEMENT_3D('',#49029,#30682,#30683);
#25640=AXIS2_PLACEMENT_3D('',#49030,#30684,#30685);
#25641=AXIS2_PLACEMENT_3D('',#49032,#30686,#30687);
#25642=AXIS2_PLACEMENT_3D('',#49034,#30689,#30690);
#25643=AXIS2_PLACEMENT_3D('',#49036,#30691,#30692);
#25644=AXIS2_PLACEMENT_3D('',#49037,#30693,#30694);
#25645=AXIS2_PLACEMENT_3D('',#49039,#30696,#30697);
#25646=AXIS2_PLACEMENT_3D('',#49041,#30698,#30699);
#25647=AXIS2_PLACEMENT_3D('',#49043,#30700,#30701);
#25648=AXIS2_PLACEMENT_3D('',#49044,#30702,#30703);
#25649=AXIS2_PLACEMENT_3D('',#49046,#30704,#30705);
#25650=AXIS2_PLACEMENT_3D('',#49048,#30707,#30708);
#25651=AXIS2_PLACEMENT_3D('',#49050,#30709,#30710);
#25652=AXIS2_PLACEMENT_3D('',#49051,#30711,#30712);
#25653=AXIS2_PLACEMENT_3D('',#49053,#30714,#30715);
#25654=AXIS2_PLACEMENT_3D('',#49054,#30716,#30717);
#25655=AXIS2_PLACEMENT_3D('',#49055,#30718,#30719);
#25656=AXIS2_PLACEMENT_3D('',#49056,#30720,#30721);
#25657=AXIS2_PLACEMENT_3D('',#49057,#30722,#30723);
#25658=AXIS2_PLACEMENT_3D('',#49058,#30724,#30725);
#25659=AXIS2_PLACEMENT_3D('',#49059,#30726,#30727);
#25660=AXIS2_PLACEMENT_3D('',#49060,#30728,#30729);
#25661=AXIS2_PLACEMENT_3D('',#49063,#30730,#30731);
#25662=AXIS2_PLACEMENT_3D('',#49064,#30732,#30733);
#25663=AXIS2_PLACEMENT_3D('',#49066,#30734,#30735);
#25664=AXIS2_PLACEMENT_3D('',#49068,#30736,#30737);
#25665=AXIS2_PLACEMENT_3D('',#49069,#30738,#30739);
#25666=AXIS2_PLACEMENT_3D('',#49070,#30740,#30741);
#25667=AXIS2_PLACEMENT_3D('',#49073,#30743,#30744);
#25668=AXIS2_PLACEMENT_3D('',#49074,#30745,#30746);
#25669=AXIS2_PLACEMENT_3D('',#49076,#30747,#30748);
#25670=AXIS2_PLACEMENT_3D('',#49079,#30750,#30751);
#25671=AXIS2_PLACEMENT_3D('',#49080,#30752,#30753);
#25672=AXIS2_PLACEMENT_3D('',#49083,#30755,#30756);
#25673=AXIS2_PLACEMENT_3D('',#49084,#30757,#30758);
#25674=AXIS2_PLACEMENT_3D('',#49085,#30759,#30760);
#25675=AXIS2_PLACEMENT_3D('',#49087,#30761,#30762);
#25676=AXIS2_PLACEMENT_3D('',#49089,#30764,#30765);
#25677=AXIS2_PLACEMENT_3D('',#49091,#30766,#30767);
#25678=AXIS2_PLACEMENT_3D('',#49092,#30768,#30769);
#25679=AXIS2_PLACEMENT_3D('',#49094,#30771,#30772);
#25680=AXIS2_PLACEMENT_3D('',#49095,#30773,#30774);
#25681=AXIS2_PLACEMENT_3D('',#49098,#30775,#30776);
#25682=AXIS2_PLACEMENT_3D('',#49099,#30777,#30778);
#25683=AXIS2_PLACEMENT_3D('',#49101,#30779,#30780);
#25684=AXIS2_PLACEMENT_3D('',#49103,#30781,#30782);
#25685=AXIS2_PLACEMENT_3D('',#49104,#30783,#30784);
#25686=AXIS2_PLACEMENT_3D('',#49105,#30785,#30786);
#25687=AXIS2_PLACEMENT_3D('',#49107,#30787,#30788);
#25688=AXIS2_PLACEMENT_3D('',#49109,#30790,#30791);
#25689=AXIS2_PLACEMENT_3D('',#49111,#30792,#30793);
#25690=AXIS2_PLACEMENT_3D('',#49113,#30794,#30795);
#25691=AXIS2_PLACEMENT_3D('',#49114,#30796,#30797);
#25692=AXIS2_PLACEMENT_3D('',#49116,#30798,#30799);
#25693=AXIS2_PLACEMENT_3D('',#49118,#30801,#30802);
#25694=AXIS2_PLACEMENT_3D('',#49120,#30803,#30804);
#25695=AXIS2_PLACEMENT_3D('',#49122,#30806,#30807);
#25696=AXIS2_PLACEMENT_3D('',#49124,#30808,#30809);
#25697=AXIS2_PLACEMENT_3D('',#49126,#30811,#30812);
#25698=AXIS2_PLACEMENT_3D('',#49127,#30813,#30814);
#25699=AXIS2_PLACEMENT_3D('',#49129,#30816,#30817);
#25700=AXIS2_PLACEMENT_3D('',#49130,#30818,#30819);
#25701=AXIS2_PLACEMENT_3D('',#49133,#30820,#30821);
#25702=AXIS2_PLACEMENT_3D('',#49134,#30822,#30823);
#25703=AXIS2_PLACEMENT_3D('',#49137,#30824,#30825);
#25704=AXIS2_PLACEMENT_3D('',#49138,#30826,#30827);
#25705=AXIS2_PLACEMENT_3D('',#49141,#30828,#30829);
#25706=AXIS2_PLACEMENT_3D('',#49142,#30830,#30831);
#25707=AXIS2_PLACEMENT_3D('',#49145,#30832,#30833);
#25708=AXIS2_PLACEMENT_3D('',#49146,#30834,#30835);
#25709=AXIS2_PLACEMENT_3D('',#49149,#30836,#30837);
#25710=AXIS2_PLACEMENT_3D('',#49150,#30838,#30839);
#25711=AXIS2_PLACEMENT_3D('',#49153,#30840,#30841);
#25712=AXIS2_PLACEMENT_3D('',#49154,#30842,#30843);
#25713=AXIS2_PLACEMENT_3D('',#49157,#30844,#30845);
#25714=AXIS2_PLACEMENT_3D('',#49158,#30846,#30847);
#25715=AXIS2_PLACEMENT_3D('',#49161,#30848,#30849);
#25716=AXIS2_PLACEMENT_3D('',#49162,#30850,#30851);
#25717=AXIS2_PLACEMENT_3D('',#49163,#30852,#30853);
#25718=AXIS2_PLACEMENT_3D('',#49189,#30854,#30855);
#25719=AXIS2_PLACEMENT_3D('',#49213,#30856,#30857);
#25720=AXIS2_PLACEMENT_3D('',#49214,#30858,#30859);
#25721=AXIS2_PLACEMENT_3D('',#49216,#30860,#30861);
#25722=AXIS2_PLACEMENT_3D('',#49241,#30862,#30863);
#25723=AXIS2_PLACEMENT_3D('',#49266,#30864,#30865);
#25724=AXIS2_PLACEMENT_3D('',#49282,#30867,#30868);
#25725=AXIS2_PLACEMENT_3D('',#49297,#30869,#30870);
#25726=AXIS2_PLACEMENT_3D('',#49322,#30871,#30872);
#25727=AXIS2_PLACEMENT_3D('',#49347,#30873,#30874);
#25728=AXIS2_PLACEMENT_3D('',#49372,#30875,#30876);
#25729=AXIS2_PLACEMENT_3D('',#49396,#30877,#30878);
#25730=AXIS2_PLACEMENT_3D('',#49397,#30879,#30880);
#25731=AXIS2_PLACEMENT_3D('',#49399,#30881,#30882);
#25732=AXIS2_PLACEMENT_3D('',#49400,#30883,#30884);
#25733=AXIS2_PLACEMENT_3D('',#49401,#30885,#30886);
#25734=AXIS2_PLACEMENT_3D('',#49425,#30887,#30888);
#25735=AXIS2_PLACEMENT_3D('',#49426,#30889,#30890);
#25736=AXIS2_PLACEMENT_3D('',#49428,#30891,#30892);
#25737=AXIS2_PLACEMENT_3D('',#49429,#30893,#30894);
#25738=AXIS2_PLACEMENT_3D('',#49430,#30895,#30896);
#25739=AXIS2_PLACEMENT_3D('',#49454,#30897,#30898);
#25740=AXIS2_PLACEMENT_3D('',#49455,#30899,#30900);
#25741=AXIS2_PLACEMENT_3D('',#49457,#30901,#30902);
#25742=AXIS2_PLACEMENT_3D('',#49458,#30903,#30904);
#25743=AXIS2_PLACEMENT_3D('',#49459,#30905,#30906);
#25744=AXIS2_PLACEMENT_3D('',#49474,#30907,#30908);
#25745=AXIS2_PLACEMENT_3D('',#49487,#30909,#30910);
#25746=AXIS2_PLACEMENT_3D('',#49489,#30911,#30912);
#25747=AXIS2_PLACEMENT_3D('',#49490,#30913,#30914);
#25748=AXIS2_PLACEMENT_3D('',#49491,#30915,#30916);
#25749=AXIS2_PLACEMENT_3D('',#49515,#30917,#30918);
#25750=AXIS2_PLACEMENT_3D('',#49516,#30919,#30920);
#25751=AXIS2_PLACEMENT_3D('',#49518,#30921,#30922);
#25752=AXIS2_PLACEMENT_3D('',#49519,#30923,#30924);
#25753=AXIS2_PLACEMENT_3D('',#49520,#30925,#30926);
#25754=AXIS2_PLACEMENT_3D('',#49544,#30927,#30928);
#25755=AXIS2_PLACEMENT_3D('',#49545,#30929,#30930);
#25756=AXIS2_PLACEMENT_3D('',#49547,#30931,#30932);
#25757=AXIS2_PLACEMENT_3D('',#49548,#30933,#30934);
#25758=AXIS2_PLACEMENT_3D('',#49549,#30935,#30936);
#25759=AXIS2_PLACEMENT_3D('',#49573,#30937,#30938);
#25760=AXIS2_PLACEMENT_3D('',#49574,#30939,#30940);
#25761=AXIS2_PLACEMENT_3D('',#49576,#30941,#30942);
#25762=AXIS2_PLACEMENT_3D('',#49579,#30944,#30945);
#25763=AXIS2_PLACEMENT_3D('',#49603,#30946,#30947);
#25764=AXIS2_PLACEMENT_3D('',#49604,#30948,#30949);
#25765=AXIS2_PLACEMENT_3D('',#49605,#30950,#30951);
#25766=AXIS2_PLACEMENT_3D('',#49606,#30952,#30953);
#25767=AXIS2_PLACEMENT_3D('',#49607,#30954,#30955);
#25768=AXIS2_PLACEMENT_3D('',#49608,#30956,#30957);
#25769=AXIS2_PLACEMENT_3D('',#49609,#30958,#30959);
#25770=AXIS2_PLACEMENT_3D('',#49610,#30960,#30961);
#25771=AXIS2_PLACEMENT_3D('',#49611,#30962,#30963);
#25772=AXIS2_PLACEMENT_3D('',#49613,#30964,#30965);
#25773=AXIS2_PLACEMENT_3D('',#49615,#30966,#30967);
#25774=AXIS2_PLACEMENT_3D('',#49616,#30968,#30969);
#25775=AXIS2_PLACEMENT_3D('',#49618,#30970,#30971);
#25776=AXIS2_PLACEMENT_3D('',#49620,#30973,#30974);
#25777=AXIS2_PLACEMENT_3D('',#49622,#30975,#30976);
#25778=AXIS2_PLACEMENT_3D('',#49623,#30977,#30978);
#25779=AXIS2_PLACEMENT_3D('',#49625,#30980,#30981);
#25780=AXIS2_PLACEMENT_3D('',#49627,#30982,#30983);
#25781=AXIS2_PLACEMENT_3D('',#49629,#30984,#30985);
#25782=AXIS2_PLACEMENT_3D('',#49630,#30986,#30987);
#25783=AXIS2_PLACEMENT_3D('',#49632,#30988,#30989);
#25784=AXIS2_PLACEMENT_3D('',#49634,#30991,#30992);
#25785=AXIS2_PLACEMENT_3D('',#49636,#30993,#30994);
#25786=AXIS2_PLACEMENT_3D('',#49637,#30995,#30996);
#25787=AXIS2_PLACEMENT_3D('',#49639,#30998,#30999);
#25788=AXIS2_PLACEMENT_3D('',#49640,#31000,#31001);
#25789=AXIS2_PLACEMENT_3D('',#49641,#31002,#31003);
#25790=AXIS2_PLACEMENT_3D('',#49642,#31004,#31005);
#25791=AXIS2_PLACEMENT_3D('',#49643,#31006,#31007);
#25792=AXIS2_PLACEMENT_3D('',#49644,#31008,#31009);
#25793=AXIS2_PLACEMENT_3D('',#49645,#31010,#31011);
#25794=AXIS2_PLACEMENT_3D('',#49654,#31016,#31017);
#25795=AXIS2_PLACEMENT_3D('',#49660,#31021,#31022);
#25796=AXIS2_PLACEMENT_3D('',#49666,#31026,#31027);
#25797=AXIS2_PLACEMENT_3D('',#49672,#31031,#31032);
#25798=AXIS2_PLACEMENT_3D('',#49678,#31036,#31037);
#25799=AXIS2_PLACEMENT_3D('',#49681,#31040,#31041);
#25800=AXIS2_PLACEMENT_3D('',#49682,#31042,#31043);
#25801=AXIS2_PLACEMENT_3D('',#49683,#31044,#31045);
#25802=AXIS2_PLACEMENT_3D('',#49685,#31046,#31047);
#25803=AXIS2_PLACEMENT_3D('',#49686,#31048,#31049);
#25804=AXIS2_PLACEMENT_3D('',#49688,#31050,#31051);
#25805=AXIS2_PLACEMENT_3D('',#49689,#31052,#31053);
#25806=AXIS2_PLACEMENT_3D('',#49691,#31054,#31055);
#25807=AXIS2_PLACEMENT_3D('',#49693,#31057,#31058);
#25808=AXIS2_PLACEMENT_3D('',#49695,#31059,#31060);
#25809=AXIS2_PLACEMENT_3D('',#49697,#31062,#31063);
#25810=AXIS2_PLACEMENT_3D('',#49699,#31064,#31065);
#25811=AXIS2_PLACEMENT_3D('',#49701,#31067,#31068);
#25812=AXIS2_PLACEMENT_3D('',#49703,#31069,#31070);
#25813=AXIS2_PLACEMENT_3D('',#49704,#31071,#31072);
#25814=AXIS2_PLACEMENT_3D('',#49706,#31073,#31074);
#25815=AXIS2_PLACEMENT_3D('',#49708,#31076,#31077);
#25816=AXIS2_PLACEMENT_3D('',#49710,#31079,#31080);
#25817=AXIS2_PLACEMENT_3D('',#49711,#31081,#31082);
#25818=AXIS2_PLACEMENT_3D('',#49712,#31083,#31084);
#25819=AXIS2_PLACEMENT_3D('',#49714,#31085,#31086);
#25820=AXIS2_PLACEMENT_3D('',#49717,#31088,#31089);
#25821=AXIS2_PLACEMENT_3D('',#49718,#31090,#31091);
#25822=AXIS2_PLACEMENT_3D('',#49720,#31092,#31093);
#25823=AXIS2_PLACEMENT_3D('',#49723,#31095,#31096);
#25824=AXIS2_PLACEMENT_3D('',#49724,#31097,#31098);
#25825=AXIS2_PLACEMENT_3D('',#49726,#31099,#31100);
#25826=AXIS2_PLACEMENT_3D('',#49729,#31102,#31103);
#25827=AXIS2_PLACEMENT_3D('',#49730,#31104,#31105);
#25828=AXIS2_PLACEMENT_3D('',#49732,#31106,#31107);
#25829=AXIS2_PLACEMENT_3D('',#49735,#31109,#31110);
#25830=AXIS2_PLACEMENT_3D('',#49736,#31111,#31112);
#25831=AXIS2_PLACEMENT_3D('',#49745,#31117,#31118);
#25832=AXIS2_PLACEMENT_3D('',#49751,#31122,#31123);
#25833=AXIS2_PLACEMENT_3D('',#49757,#31127,#31128);
#25834=AXIS2_PLACEMENT_3D('',#49760,#31131,#31132);
#25835=AXIS2_PLACEMENT_3D('',#49761,#31133,#31134);
#25836=AXIS2_PLACEMENT_3D('',#49762,#31135,#31136);
#25837=AXIS2_PLACEMENT_3D('',#49763,#31137,#31138);
#25838=AXIS2_PLACEMENT_3D('',#49765,#31139,#31140);
#25839=AXIS2_PLACEMENT_3D('',#49768,#31142,#31143);
#25840=AXIS2_PLACEMENT_3D('',#49769,#31144,#31145);
#25841=AXIS2_PLACEMENT_3D('',#49771,#31146,#31147);
#25842=AXIS2_PLACEMENT_3D('',#49774,#31149,#31150);
#25843=AXIS2_PLACEMENT_3D('',#49775,#31151,#31152);
#25844=AXIS2_PLACEMENT_3D('',#49777,#31153,#31154);
#25845=AXIS2_PLACEMENT_3D('',#49780,#31156,#31157);
#25846=AXIS2_PLACEMENT_3D('',#49781,#31158,#31159);
#25847=AXIS2_PLACEMENT_3D('',#49783,#31160,#31161);
#25848=AXIS2_PLACEMENT_3D('',#49786,#31163,#31164);
#25849=AXIS2_PLACEMENT_3D('',#49787,#31165,#31166);
#25850=AXIS2_PLACEMENT_3D('',#49789,#31167,#31168);
#25851=AXIS2_PLACEMENT_3D('',#49792,#31170,#31171);
#25852=AXIS2_PLACEMENT_3D('',#49793,#31172,#31173);
#25853=AXIS2_PLACEMENT_3D('',#49795,#31174,#31175);
#25854=AXIS2_PLACEMENT_3D('',#49798,#31177,#31178);
#25855=AXIS2_PLACEMENT_3D('',#49799,#31179,#31180);
#25856=AXIS2_PLACEMENT_3D('',#49801,#31181,#31182);
#25857=AXIS2_PLACEMENT_3D('',#49804,#31184,#31185);
#25858=AXIS2_PLACEMENT_3D('',#49805,#31186,#31187);
#25859=AXIS2_PLACEMENT_3D('',#49807,#31188,#31189);
#25860=AXIS2_PLACEMENT_3D('',#49810,#31191,#31192);
#25861=AXIS2_PLACEMENT_3D('',#49811,#31193,#31194);
#25862=AXIS2_PLACEMENT_3D('',#49820,#31199,#31200);
#25863=AXIS2_PLACEMENT_3D('',#49826,#31204,#31205);
#25864=AXIS2_PLACEMENT_3D('',#49832,#31209,#31210);
#25865=AXIS2_PLACEMENT_3D('',#49835,#31213,#31214);
#25866=AXIS2_PLACEMENT_3D('',#49836,#31215,#31216);
#25867=AXIS2_PLACEMENT_3D('',#49837,#31217,#31218);
#25868=AXIS2_PLACEMENT_3D('',#49838,#31219,#31220);
#25869=AXIS2_PLACEMENT_3D('',#49840,#31221,#31222);
#25870=AXIS2_PLACEMENT_3D('',#49843,#31224,#31225);
#25871=AXIS2_PLACEMENT_3D('',#49844,#31226,#31227);
#25872=AXIS2_PLACEMENT_3D('',#49845,#31228,#31229);
#25873=AXIS2_PLACEMENT_3D('',#49847,#31230,#31231);
#25874=AXIS2_PLACEMENT_3D('',#49850,#31233,#31234);
#25875=AXIS2_PLACEMENT_3D('',#49851,#31235,#31236);
#25876=AXIS2_PLACEMENT_3D('',#49852,#31237,#31238);
#25877=AXIS2_PLACEMENT_3D('',#49854,#31239,#31240);
#25878=AXIS2_PLACEMENT_3D('',#49857,#31242,#31243);
#25879=AXIS2_PLACEMENT_3D('',#49858,#31244,#31245);
#25880=AXIS2_PLACEMENT_3D('',#49859,#31246,#31247);
#25881=AXIS2_PLACEMENT_3D('',#49861,#31248,#31249);
#25882=AXIS2_PLACEMENT_3D('',#49864,#31251,#31252);
#25883=AXIS2_PLACEMENT_3D('',#49865,#31253,#31254);
#25884=AXIS2_PLACEMENT_3D('',#49866,#31255,#31256);
#25885=AXIS2_PLACEMENT_3D('',#49868,#31257,#31258);
#25886=AXIS2_PLACEMENT_3D('',#49871,#31260,#31261);
#25887=AXIS2_PLACEMENT_3D('',#49872,#31262,#31263);
#25888=AXIS2_PLACEMENT_3D('',#49873,#31264,#31265);
#25889=AXIS2_PLACEMENT_3D('',#49875,#31266,#31267);
#25890=AXIS2_PLACEMENT_3D('',#49878,#31269,#31270);
#25891=AXIS2_PLACEMENT_3D('',#49879,#31271,#31272);
#25892=AXIS2_PLACEMENT_3D('',#49880,#31273,#31274);
#25893=AXIS2_PLACEMENT_3D('',#49882,#31275,#31276);
#25894=AXIS2_PLACEMENT_3D('',#49885,#31278,#31279);
#25895=AXIS2_PLACEMENT_3D('',#49886,#31280,#31281);
#25896=AXIS2_PLACEMENT_3D('',#49887,#31282,#31283);
#25897=AXIS2_PLACEMENT_3D('',#49889,#31284,#31285);
#25898=AXIS2_PLACEMENT_3D('',#49892,#31287,#31288);
#25899=AXIS2_PLACEMENT_3D('',#49893,#31289,#31290);
#25900=AXIS2_PLACEMENT_3D('',#49902,#31295,#31296);
#25901=AXIS2_PLACEMENT_3D('',#49908,#31300,#31301);
#25902=AXIS2_PLACEMENT_3D('',#49914,#31305,#31306);
#25903=AXIS2_PLACEMENT_3D('',#49917,#31309,#31310);
#25904=AXIS2_PLACEMENT_3D('',#49918,#31311,#31312);
#25905=AXIS2_PLACEMENT_3D('',#49919,#31313,#31314);
#25906=AXIS2_PLACEMENT_3D('',#49920,#31315,#31316);
#25907=AXIS2_PLACEMENT_3D('',#49921,#31317,#31318);
#25908=AXIS2_PLACEMENT_3D('',#49925,#31320,#31321);
#25909=AXIS2_PLACEMENT_3D('',#49926,#31322,#31323);
#25910=AXIS2_PLACEMENT_3D('',#49930,#31325,#31326);
#25911=AXIS2_PLACEMENT_3D('',#49933,#31328,#31329);
#25912=AXIS2_PLACEMENT_3D('',#49935,#31330,#31331);
#25913=AXIS2_PLACEMENT_3D('',#49937,#31333,#31334);
#25914=AXIS2_PLACEMENT_3D('',#49941,#31336,#31337);
#25915=AXIS2_PLACEMENT_3D('',#49942,#31338,#31339);
#25916=AXIS2_PLACEMENT_3D('',#49946,#31341,#31342);
#25917=AXIS2_PLACEMENT_3D('',#49949,#31344,#31345);
#25918=AXIS2_PLACEMENT_3D('',#49951,#31346,#31347);
#25919=AXIS2_PLACEMENT_3D('',#49953,#31349,#31350);
#25920=AXIS2_PLACEMENT_3D('',#49957,#31352,#31353);
#25921=AXIS2_PLACEMENT_3D('',#49958,#31354,#31355);
#25922=AXIS2_PLACEMENT_3D('',#49962,#31357,#31358);
#25923=AXIS2_PLACEMENT_3D('',#49965,#31360,#31361);
#25924=AXIS2_PLACEMENT_3D('',#49967,#31362,#31363);
#25925=AXIS2_PLACEMENT_3D('',#49969,#31365,#31366);
#25926=AXIS2_PLACEMENT_3D('',#49973,#31368,#31369);
#25927=AXIS2_PLACEMENT_3D('',#49974,#31370,#31371);
#25928=AXIS2_PLACEMENT_3D('',#49978,#31373,#31374);
#25929=AXIS2_PLACEMENT_3D('',#49981,#31376,#31377);
#25930=AXIS2_PLACEMENT_3D('',#49983,#31378,#31379);
#25931=AXIS2_PLACEMENT_3D('',#49985,#31381,#31382);
#25932=AXIS2_PLACEMENT_3D('',#49996,#31389,#31390);
#25933=AXIS2_PLACEMENT_3D('',#50007,#31397,#31398);
#25934=AXIS2_PLACEMENT_3D('',#50026,#31409,#31410);
#25935=AXIS2_PLACEMENT_3D('',#50030,#31413,#31414);
#25936=AXIS2_PLACEMENT_3D('',#50034,#31417,#31418);
#25937=AXIS2_PLACEMENT_3D('',#50038,#31421,#31422);
#25938=AXIS2_PLACEMENT_3D('',#50042,#31425,#31426);
#25939=AXIS2_PLACEMENT_3D('',#50044,#31428,#31429);
#25940=AXIS2_PLACEMENT_3D('',#50048,#31432,#31433);
#25941=AXIS2_PLACEMENT_3D('',#50052,#31436,#31437);
#25942=AXIS2_PLACEMENT_3D('',#50056,#31440,#31441);
#25943=AXIS2_PLACEMENT_3D('',#50060,#31444,#31445);
#25944=AXIS2_PLACEMENT_3D('',#50062,#31447,#31448);
#25945=AXIS2_PLACEMENT_3D('',#50063,#31449,#31450);
#25946=AXIS2_PLACEMENT_3D('',#50064,#31451,#31452);
#25947=AXIS2_PLACEMENT_3D('',#50073,#31457,#31458);
#25948=AXIS2_PLACEMENT_3D('',#50079,#31462,#31463);
#25949=AXIS2_PLACEMENT_3D('',#50085,#31467,#31468);
#25950=AXIS2_PLACEMENT_3D('',#50091,#31472,#31473);
#25951=AXIS2_PLACEMENT_3D('',#50097,#31477,#31478);
#25952=AXIS2_PLACEMENT_3D('',#50103,#31482,#31483);
#25953=AXIS2_PLACEMENT_3D('',#50109,#31487,#31488);
#25954=AXIS2_PLACEMENT_3D('',#50112,#31491,#31492);
#25955=AXIS2_PLACEMENT_3D('',#50113,#31493,#31494);
#25956=AXIS2_PLACEMENT_3D('',#50114,#31495,#31496);
#25957=AXIS2_PLACEMENT_3D('',#50115,#31497,#31498);
#25958=AXIS2_PLACEMENT_3D('',#50124,#31503,#31504);
#25959=AXIS2_PLACEMENT_3D('',#50130,#31508,#31509);
#25960=AXIS2_PLACEMENT_3D('',#50136,#31513,#31514);
#25961=AXIS2_PLACEMENT_3D('',#50142,#31518,#31519);
#25962=AXIS2_PLACEMENT_3D('',#50148,#31523,#31524);
#25963=AXIS2_PLACEMENT_3D('',#50154,#31528,#31529);
#25964=AXIS2_PLACEMENT_3D('',#50160,#31533,#31534);
#25965=AXIS2_PLACEMENT_3D('',#50163,#31537,#31538);
#25966=AXIS2_PLACEMENT_3D('',#50164,#31539,#31540);
#25967=AXIS2_PLACEMENT_3D('',#50165,#31541,#31542);
#25968=AXIS2_PLACEMENT_3D('',#50166,#31543,#31544);
#25969=AXIS2_PLACEMENT_3D('',#50167,#31545,#31546);
#25970=AXIS2_PLACEMENT_3D('',#50168,#31547,#31548);
#25971=AXIS2_PLACEMENT_3D('',#50169,#31549,#31550);
#25972=AXIS2_PLACEMENT_3D('',#50171,#31551,#31552);
#25973=AXIS2_PLACEMENT_3D('',#50174,#31554,#31555);
#25974=AXIS2_PLACEMENT_3D('',#50175,#31556,#31557);
#25975=AXIS2_PLACEMENT_3D('',#50178,#31559,#31560);
#25976=AXIS2_PLACEMENT_3D('',#50179,#31561,#31562);
#25977=AXIS2_PLACEMENT_3D('',#50181,#31563,#31564);
#25978=AXIS2_PLACEMENT_3D('',#50182,#31565,#31566);
#25979=AXIS2_PLACEMENT_3D('',#50185,#31568,#31569);
#25980=AXIS2_PLACEMENT_3D('',#50186,#31570,#31571);
#25981=AXIS2_PLACEMENT_3D('',#50187,#31572,#31573);
#25982=AXIS2_PLACEMENT_3D('',#50188,#31574,#31575);
#25983=AXIS2_PLACEMENT_3D('',#50197,#31580,#31581);
#25984=AXIS2_PLACEMENT_3D('',#50203,#31585,#31586);
#25985=AXIS2_PLACEMENT_3D('',#50209,#31590,#31591);
#25986=AXIS2_PLACEMENT_3D('',#50215,#31595,#31596);
#25987=AXIS2_PLACEMENT_3D('',#50221,#31600,#31601);
#25988=AXIS2_PLACEMENT_3D('',#50224,#31604,#31605);
#25989=AXIS2_PLACEMENT_3D('',#50225,#31606,#31607);
#25990=AXIS2_PLACEMENT_3D('',#50226,#31608,#31609);
#25991=AXIS2_PLACEMENT_3D('',#50228,#31610,#31611);
#25992=AXIS2_PLACEMENT_3D('',#50230,#31612,#31613);
#25993=AXIS2_PLACEMENT_3D('',#50231,#31614,#31615);
#25994=AXIS2_PLACEMENT_3D('',#50234,#31617,#31618);
#25995=AXIS2_PLACEMENT_3D('',#50235,#31619,#31620);
#25996=AXIS2_PLACEMENT_3D('',#50236,#31621,#31622);
#25997=AXIS2_PLACEMENT_3D('',#50238,#31623,#31624);
#25998=AXIS2_PLACEMENT_3D('',#50239,#31625,#31626);
#25999=AXIS2_PLACEMENT_3D('',#50241,#31627,#31628);
#26000=AXIS2_PLACEMENT_3D('',#50243,#31630,#31631);
#26001=AXIS2_PLACEMENT_3D('',#50245,#31632,#31633);
#26002=AXIS2_PLACEMENT_3D('',#50247,#31635,#31636);
#26003=AXIS2_PLACEMENT_3D('',#50249,#31637,#31638);
#26004=AXIS2_PLACEMENT_3D('',#50251,#31640,#31641);
#26005=AXIS2_PLACEMENT_3D('',#50253,#31642,#31643);
#26006=AXIS2_PLACEMENT_3D('',#50254,#31644,#31645);
#26007=AXIS2_PLACEMENT_3D('',#50256,#31646,#31647);
#26008=AXIS2_PLACEMENT_3D('',#50258,#31649,#31650);
#26009=AXIS2_PLACEMENT_3D('',#50260,#31652,#31653);
#26010=AXIS2_PLACEMENT_3D('',#50261,#31654,#31655);
#26011=AXIS2_PLACEMENT_3D('',#50292,#31657,#31658);
#26012=AXIS2_PLACEMENT_3D('',#50333,#31659,#31660);
#26013=AXIS2_PLACEMENT_3D('',#50420,#31662,#31663);
#26014=AXIS2_PLACEMENT_3D('',#50510,#31665,#31666);
#26015=AXIS2_PLACEMENT_3D('',#50597,#31668,#31669);
#26016=AXIS2_PLACEMENT_3D('',#50687,#31671,#31672);
#26017=AXIS2_PLACEMENT_3D('',#50774,#31674,#31675);
#26018=AXIS2_PLACEMENT_3D('',#50861,#31677,#31678);
#26019=AXIS2_PLACEMENT_3D('',#50951,#31680,#31681);
#26020=AXIS2_PLACEMENT_3D('',#50956,#31683,#31684);
#26021=AXIS2_PLACEMENT_3D('',#50967,#31685,#31686);
#26022=AXIS2_PLACEMENT_3D('',#50980,#31688,#31689);
#26023=AXIS2_PLACEMENT_3D('',#50993,#31690,#31691);
#26024=AXIS2_PLACEMENT_3D('',#51030,#31693,#31694);
#26025=AXIS2_PLACEMENT_3D('',#51067,#31696,#31697);
#26026=AXIS2_PLACEMENT_3D('',#51105,#31699,#31700);
#26027=AXIS2_PLACEMENT_3D('',#51142,#31702,#31703);
#26028=AXIS2_PLACEMENT_3D('',#51179,#31705,#31706);
#26029=AXIS2_PLACEMENT_3D('',#51217,#31708,#31709);
#26030=AXIS2_PLACEMENT_3D('',#51255,#31711,#31712);
#26031=AXIS2_PLACEMENT_3D('',#51266,#31714,#31715);
#26032=AXIS2_PLACEMENT_3D('',#51277,#31716,#31717);
#26033=AXIS2_PLACEMENT_3D('',#52420,#31718,#31719);
#26034=AXIS2_PLACEMENT_3D('',#52424,#31721,#31722);
#26035=AXIS2_PLACEMENT_3D('',#52425,#31723,#31724);
#26036=AXIS2_PLACEMENT_3D('',#52427,#31725,#31726);
#26037=AXIS2_PLACEMENT_3D('',#52429,#31727,#31728);
#26038=AXIS2_PLACEMENT_3D('',#52431,#31729,#31730);
#26039=AXIS2_PLACEMENT_3D('',#52432,#31731,#31732);
#26040=AXIS2_PLACEMENT_3D('',#52434,#31733,#31734);
#26041=AXIS2_PLACEMENT_3D('',#52436,#31736,#31737);
#26042=AXIS2_PLACEMENT_3D('',#52438,#31738,#31739);
#26043=AXIS2_PLACEMENT_3D('',#52440,#31741,#31742);
#26044=AXIS2_PLACEMENT_3D('',#52442,#31743,#31744);
#26045=AXIS2_PLACEMENT_3D('',#52444,#31746,#31747);
#26046=AXIS2_PLACEMENT_3D('',#52450,#31751,#31752);
#26047=AXIS2_PLACEMENT_3D('',#52451,#31753,#31754);
#26048=AXIS2_PLACEMENT_3D('',#52453,#31755,#31756);
#26049=AXIS2_PLACEMENT_3D('',#52454,#31757,#31758);
#26050=AXIS2_PLACEMENT_3D('',#52455,#31759,#31760);
#26051=AXIS2_PLACEMENT_3D('',#52456,#31761,#31762);
#26052=AXIS2_PLACEMENT_3D('',#52459,#31764,#31765);
#26053=AXIS2_PLACEMENT_3D('',#52460,#31766,#31767);
#26054=AXIS2_PLACEMENT_3D('',#52461,#31768,#31769);
#26055=AXIS2_PLACEMENT_3D('',#52462,#31770,#31771);
#26056=AXIS2_PLACEMENT_3D('',#52464,#31772,#31773);
#26057=AXIS2_PLACEMENT_3D('',#52465,#31774,#31775);
#26058=AXIS2_PLACEMENT_3D('',#52467,#31776,#31777);
#26059=AXIS2_PLACEMENT_3D('',#52469,#31779,#31780);
#26060=AXIS2_PLACEMENT_3D('',#52471,#31781,#31782);
#26061=AXIS2_PLACEMENT_3D('',#52473,#31784,#31785);
#26062=AXIS2_PLACEMENT_3D('',#52475,#31786,#31787);
#26063=AXIS2_PLACEMENT_3D('',#52477,#31789,#31790);
#26064=AXIS2_PLACEMENT_3D('',#52479,#31791,#31792);
#26065=AXIS2_PLACEMENT_3D('',#52480,#31793,#31794);
#26066=AXIS2_PLACEMENT_3D('',#52482,#31795,#31796);
#26067=AXIS2_PLACEMENT_3D('',#52484,#31798,#31799);
#26068=AXIS2_PLACEMENT_3D('',#52486,#31800,#31801);
#26069=AXIS2_PLACEMENT_3D('',#52488,#31803,#31804);
#26070=AXIS2_PLACEMENT_3D('',#52490,#31805,#31806);
#26071=AXIS2_PLACEMENT_3D('',#52492,#31808,#31809);
#26072=AXIS2_PLACEMENT_3D('',#52493,#31810,#31811);
#26073=AXIS2_PLACEMENT_3D('',#52502,#31816,#31817);
#26074=AXIS2_PLACEMENT_3D('',#52508,#31821,#31822);
#26075=AXIS2_PLACEMENT_3D('',#52514,#31826,#31827);
#26076=AXIS2_PLACEMENT_3D('',#52520,#31831,#31832);
#26077=AXIS2_PLACEMENT_3D('',#52526,#31836,#31837);
#26078=AXIS2_PLACEMENT_3D('',#52529,#31840,#31841);
#26079=AXIS2_PLACEMENT_3D('',#52530,#31842,#31843);
#26080=AXIS2_PLACEMENT_3D('',#52531,#31844,#31845);
#26081=AXIS2_PLACEMENT_3D('',#52532,#31846,#31847);
#26082=AXIS2_PLACEMENT_3D('',#52534,#31848,#31849);
#26083=AXIS2_PLACEMENT_3D('',#52535,#31850,#31851);
#26084=AXIS2_PLACEMENT_3D('',#52537,#31852,#31853);
#26085=AXIS2_PLACEMENT_3D('',#52539,#31855,#31856);
#26086=AXIS2_PLACEMENT_3D('',#52541,#31857,#31858);
#26087=AXIS2_PLACEMENT_3D('',#52543,#31860,#31861);
#26088=AXIS2_PLACEMENT_3D('',#52545,#31862,#31863);
#26089=AXIS2_PLACEMENT_3D('',#52547,#31865,#31866);
#26090=AXIS2_PLACEMENT_3D('',#52549,#31867,#31868);
#26091=AXIS2_PLACEMENT_3D('',#52550,#31869,#31870);
#26092=AXIS2_PLACEMENT_3D('',#52552,#31871,#31872);
#26093=AXIS2_PLACEMENT_3D('',#52554,#31874,#31875);
#26094=AXIS2_PLACEMENT_3D('',#52556,#31876,#31877);
#26095=AXIS2_PLACEMENT_3D('',#52558,#31879,#31880);
#26096=AXIS2_PLACEMENT_3D('',#52560,#31881,#31882);
#26097=AXIS2_PLACEMENT_3D('',#52562,#31884,#31885);
#26098=AXIS2_PLACEMENT_3D('',#52563,#31886,#31887);
#26099=AXIS2_PLACEMENT_3D('',#52572,#31892,#31893);
#26100=AXIS2_PLACEMENT_3D('',#52578,#31897,#31898);
#26101=AXIS2_PLACEMENT_3D('',#52584,#31902,#31903);
#26102=AXIS2_PLACEMENT_3D('',#52590,#31907,#31908);
#26103=AXIS2_PLACEMENT_3D('',#52596,#31912,#31913);
#26104=AXIS2_PLACEMENT_3D('',#52599,#31916,#31917);
#26105=AXIS2_PLACEMENT_3D('',#52600,#31918,#31919);
#26106=AXIS2_PLACEMENT_3D('',#52601,#31920,#31921);
#26107=AXIS2_PLACEMENT_3D('',#52602,#31922,#31923);
#26108=AXIS2_PLACEMENT_3D('',#52603,#31924,#31925);
#26109=AXIS2_PLACEMENT_3D('',#52604,#31926,#31927);
#26110=AXIS2_PLACEMENT_3D('',#52605,#31928,#31929);
#26111=AXIS2_PLACEMENT_3D('',#52606,#31930,#31931);
#26112=AXIS2_PLACEMENT_3D('',#52607,#31932,#31933);
#26113=AXIS2_PLACEMENT_3D('',#52608,#31934,#31935);
#26114=AXIS2_PLACEMENT_3D('',#52609,#31936,#31937);
#26115=AXIS2_PLACEMENT_3D('',#52610,#31938,#31939);
#26116=AXIS2_PLACEMENT_3D('',#52611,#31940,#31941);
#26117=AXIS2_PLACEMENT_3D('',#52612,#31942,#31943);
#26118=AXIS2_PLACEMENT_3D('',#52613,#31944,#31945);
#26119=AXIS2_PLACEMENT_3D('',#52614,#31946,#31947);
#26120=AXIS2_PLACEMENT_3D('',#52615,#31948,#31949);
#26121=AXIS2_PLACEMENT_3D('',#52616,#31950,#31951);
#26122=AXIS2_PLACEMENT_3D('',#52617,#31952,#31953);
#26123=AXIS2_PLACEMENT_3D('',#52618,#31954,#31955);
#26124=AXIS2_PLACEMENT_3D('',#52619,#31956,#31957);
#26125=AXIS2_PLACEMENT_3D('',#52620,#31958,#31959);
#26126=AXIS2_PLACEMENT_3D('',#52621,#31960,#31961);
#26127=AXIS2_PLACEMENT_3D('',#52622,#31962,#31963);
#26128=AXIS2_PLACEMENT_3D('',#52623,#31964,#31965);
#26129=AXIS2_PLACEMENT_3D('',#52648,#31967,#31968);
#26130=AXIS2_PLACEMENT_3D('',#52653,#31969,#31970);
#26131=AXIS2_PLACEMENT_3D('',#52740,#31972,#31973);
#26132=AXIS2_PLACEMENT_3D('',#52830,#31975,#31976);
#26133=AXIS2_PLACEMENT_3D('',#52917,#31978,#31979);
#26134=AXIS2_PLACEMENT_3D('',#53004,#31981,#31982);
#26135=AXIS2_PLACEMENT_3D('',#53091,#31984,#31985);
#26136=AXIS2_PLACEMENT_3D('',#53178,#31987,#31988);
#26137=AXIS2_PLACEMENT_3D('',#53265,#31990,#31991);
#26138=AXIS2_PLACEMENT_3D('',#53337,#31993,#31994);
#26139=AXIS2_PLACEMENT_3D('',#53388,#31996,#31997);
#26140=AXIS2_PLACEMENT_3D('',#53436,#31999,#32000);
#26141=AXIS2_PLACEMENT_3D('',#53484,#32002,#32003);
#26142=AXIS2_PLACEMENT_3D('',#53535,#32005,#32006);
#26143=AXIS2_PLACEMENT_3D('',#53586,#32008,#32009);
#26144=AXIS2_PLACEMENT_3D('',#53634,#32011,#32012);
#26145=AXIS2_PLACEMENT_3D('',#53685,#32014,#32015);
#26146=AXIS2_PLACEMENT_3D('',#53736,#32017,#32018);
#26147=AXIS2_PLACEMENT_3D('',#53784,#32020,#32021);
#26148=AXIS2_PLACEMENT_3D('',#53832,#32023,#32024);
#26149=AXIS2_PLACEMENT_3D('',#53883,#32026,#32027);
#26150=AXIS2_PLACEMENT_3D('',#53934,#32029,#32030);
#26151=AXIS2_PLACEMENT_3D('',#53982,#32032,#32033);
#26152=AXIS2_PLACEMENT_3D('',#54033,#32035,#32036);
#26153=AXIS2_PLACEMENT_3D('',#54084,#32038,#32039);
#26154=AXIS2_PLACEMENT_3D('',#54132,#32041,#32042);
#26155=AXIS2_PLACEMENT_3D('',#54180,#32044,#32045);
#26156=AXIS2_PLACEMENT_3D('',#54231,#32047,#32048);
#26157=AXIS2_PLACEMENT_3D('',#54282,#32050,#32051);
#26158=AXIS2_PLACEMENT_3D('',#54330,#32053,#32054);
#26159=AXIS2_PLACEMENT_3D('',#54381,#32056,#32057);
#26160=AXIS2_PLACEMENT_3D('',#54432,#32059,#32060);
#26161=AXIS2_PLACEMENT_3D('',#54480,#32062,#32063);
#26162=AXIS2_PLACEMENT_3D('',#54528,#32065,#32066);
#26163=AXIS2_PLACEMENT_3D('',#54579,#32068,#32069);
#26164=AXIS2_PLACEMENT_3D('',#54630,#32071,#32072);
#26165=AXIS2_PLACEMENT_3D('',#54678,#32074,#32075);
#26166=AXIS2_PLACEMENT_3D('',#54729,#32077,#32078);
#26167=AXIS2_PLACEMENT_3D('',#54780,#32080,#32081);
#26168=AXIS2_PLACEMENT_3D('',#54828,#32083,#32084);
#26169=AXIS2_PLACEMENT_3D('',#54876,#32086,#32087);
#26170=AXIS2_PLACEMENT_3D('',#54927,#32089,#32090);
#26171=AXIS2_PLACEMENT_3D('',#54978,#32092,#32093);
#26172=AXIS2_PLACEMENT_3D('',#55026,#32095,#32096);
#26173=AXIS2_PLACEMENT_3D('',#55077,#32098,#32099);
#26174=AXIS2_PLACEMENT_3D('',#55128,#32101,#32102);
#26175=AXIS2_PLACEMENT_3D('',#55176,#32104,#32105);
#26176=AXIS2_PLACEMENT_3D('',#55224,#32107,#32108);
#26177=AXIS2_PLACEMENT_3D('',#55275,#32110,#32111);
#26178=AXIS2_PLACEMENT_3D('',#55326,#32113,#32114);
#26179=AXIS2_PLACEMENT_3D('',#55374,#32116,#32117);
#26180=AXIS2_PLACEMENT_3D('',#55425,#32119,#32120);
#26181=AXIS2_PLACEMENT_3D('',#55476,#32122,#32123);
#26182=AXIS2_PLACEMENT_3D('',#55524,#32125,#32126);
#26183=AXIS2_PLACEMENT_3D('',#55572,#32128,#32129);
#26184=AXIS2_PLACEMENT_3D('',#55623,#32131,#32132);
#26185=AXIS2_PLACEMENT_3D('',#55689,#32134,#32135);
#26186=AXIS2_PLACEMENT_3D('',#55779,#32137,#32138);
#26187=AXIS2_PLACEMENT_3D('',#55866,#32140,#32141);
#26188=AXIS2_PLACEMENT_3D('',#55953,#32143,#32144);
#26189=AXIS2_PLACEMENT_3D('',#56040,#32146,#32147);
#26190=AXIS2_PLACEMENT_3D('',#56127,#32149,#32150);
#26191=AXIS2_PLACEMENT_3D('',#56214,#32152,#32153);
#26192=AXIS2_PLACEMENT_3D('',#56304,#32155,#32156);
#26193=AXIS2_PLACEMENT_3D('',#56313,#32158,#32159);
#26194=AXIS2_PLACEMENT_3D('',#56314,#32160,#32161);
#26195=AXIS2_PLACEMENT_3D('',#56336,#32163,#32164);
#26196=AXIS2_PLACEMENT_3D('',#56350,#32165,#32166);
#26197=AXIS2_PLACEMENT_3D('',#56388,#32168,#32169);
#26198=AXIS2_PLACEMENT_3D('',#56424,#32171,#32172);
#26199=AXIS2_PLACEMENT_3D('',#56462,#32174,#32175);
#26200=AXIS2_PLACEMENT_3D('',#56498,#32177,#32178);
#26201=AXIS2_PLACEMENT_3D('',#56536,#32180,#32181);
#26202=AXIS2_PLACEMENT_3D('',#56573,#32183,#32184);
#26203=AXIS2_PLACEMENT_3D('',#56608,#32186,#32187);
#26204=AXIS2_PLACEMENT_3D('',#56635,#32189,#32190);
#26205=AXIS2_PLACEMENT_3D('',#56659,#32192,#32193);
#26206=AXIS2_PLACEMENT_3D('',#56683,#32195,#32196);
#26207=AXIS2_PLACEMENT_3D('',#56707,#32198,#32199);
#26208=AXIS2_PLACEMENT_3D('',#56733,#32201,#32202);
#26209=AXIS2_PLACEMENT_3D('',#56757,#32204,#32205);
#26210=AXIS2_PLACEMENT_3D('',#56781,#32207,#32208);
#26211=AXIS2_PLACEMENT_3D('',#56807,#32210,#32211);
#26212=AXIS2_PLACEMENT_3D('',#56831,#32213,#32214);
#26213=AXIS2_PLACEMENT_3D('',#56855,#32216,#32217);
#26214=AXIS2_PLACEMENT_3D('',#56879,#32219,#32220);
#26215=AXIS2_PLACEMENT_3D('',#56905,#32222,#32223);
#26216=AXIS2_PLACEMENT_3D('',#56929,#32225,#32226);
#26217=AXIS2_PLACEMENT_3D('',#56953,#32228,#32229);
#26218=AXIS2_PLACEMENT_3D('',#56979,#32231,#32232);
#26219=AXIS2_PLACEMENT_3D('',#57003,#32234,#32235);
#26220=AXIS2_PLACEMENT_3D('',#57027,#32237,#32238);
#26221=AXIS2_PLACEMENT_3D('',#57051,#32240,#32241);
#26222=AXIS2_PLACEMENT_3D('',#57077,#32243,#32244);
#26223=AXIS2_PLACEMENT_3D('',#57101,#32246,#32247);
#26224=AXIS2_PLACEMENT_3D('',#57125,#32249,#32250);
#26225=AXIS2_PLACEMENT_3D('',#57151,#32252,#32253);
#26226=AXIS2_PLACEMENT_3D('',#57175,#32255,#32256);
#26227=AXIS2_PLACEMENT_3D('',#57199,#32258,#32259);
#26228=AXIS2_PLACEMENT_3D('',#57223,#32261,#32262);
#26229=AXIS2_PLACEMENT_3D('',#57249,#32264,#32265);
#26230=AXIS2_PLACEMENT_3D('',#57273,#32267,#32268);
#26231=AXIS2_PLACEMENT_3D('',#57297,#32270,#32271);
#26232=AXIS2_PLACEMENT_3D('',#57323,#32273,#32274);
#26233=AXIS2_PLACEMENT_3D('',#57347,#32276,#32277);
#26234=AXIS2_PLACEMENT_3D('',#57371,#32279,#32280);
#26235=AXIS2_PLACEMENT_3D('',#57395,#32282,#32283);
#26236=AXIS2_PLACEMENT_3D('',#57421,#32285,#32286);
#26237=AXIS2_PLACEMENT_3D('',#57445,#32288,#32289);
#26238=AXIS2_PLACEMENT_3D('',#57469,#32291,#32292);
#26239=AXIS2_PLACEMENT_3D('',#57495,#32294,#32295);
#26240=AXIS2_PLACEMENT_3D('',#57519,#32297,#32298);
#26241=AXIS2_PLACEMENT_3D('',#57543,#32300,#32301);
#26242=AXIS2_PLACEMENT_3D('',#57567,#32303,#32304);
#26243=AXIS2_PLACEMENT_3D('',#57593,#32306,#32307);
#26244=AXIS2_PLACEMENT_3D('',#57617,#32309,#32310);
#26245=AXIS2_PLACEMENT_3D('',#57641,#32312,#32313);
#26246=AXIS2_PLACEMENT_3D('',#57667,#32315,#32316);
#26247=AXIS2_PLACEMENT_3D('',#57691,#32318,#32319);
#26248=AXIS2_PLACEMENT_3D('',#57715,#32321,#32322);
#26249=AXIS2_PLACEMENT_3D('',#57740,#32324,#32325);
#26250=AXIS2_PLACEMENT_3D('',#57767,#32327,#32328);
#26251=AXIS2_PLACEMENT_3D('',#57804,#32330,#32331);
#26252=AXIS2_PLACEMENT_3D('',#57840,#32333,#32334);
#26253=AXIS2_PLACEMENT_3D('',#57878,#32336,#32337);
#26254=AXIS2_PLACEMENT_3D('',#57914,#32339,#32340);
#26255=AXIS2_PLACEMENT_3D('',#57952,#32342,#32343);
#26256=AXIS2_PLACEMENT_3D('',#57989,#32345,#32346);
#26257=AXIS2_PLACEMENT_3D('',#58026,#32348,#32349);
#26258=AXIS2_PLACEMENT_3D('',#58028,#32350,#32351);
#26259=AXIS2_PLACEMENT_3D('',#58105,#32352,#32353);
#26260=AXIS2_PLACEMENT_3D('',#58106,#32354,#32355);
#26261=AXIS2_PLACEMENT_3D('',#58109,#32357,#32358);
#26262=AXIS2_PLACEMENT_3D('',#58110,#32359,#32360);
#26263=AXIS2_PLACEMENT_3D('',#60184,#32361,#32362);
#26264=AXIS2_PLACEMENT_3D('',#62239,#32363,#32364);
#26265=AXIS2_PLACEMENT_3D('',#62248,#32369,#32370);
#26266=AXIS2_PLACEMENT_3D('',#62250,#32371,#32372);
#26267=AXIS2_PLACEMENT_3D('',#62254,#32375,#32376);
#26268=AXIS2_PLACEMENT_3D('',#62258,#32379,#32380);
#26269=AXIS2_PLACEMENT_3D('',#62262,#32383,#32384);
#26270=AXIS2_PLACEMENT_3D('',#62263,#32385,#32386);
#26271=AXIS2_PLACEMENT_3D('',#62264,#32387,#32388);
#26272=AXIS2_PLACEMENT_3D('',#62266,#32389,#32390);
#26273=AXIS2_PLACEMENT_3D('',#62269,#32392,#32393);
#26274=AXIS2_PLACEMENT_3D('',#62270,#32394,#32395);
#26275=AXIS2_PLACEMENT_3D('',#62271,#32396,#32397);
#26276=AXIS2_PLACEMENT_3D('',#62273,#32398,#32399);
#26277=AXIS2_PLACEMENT_3D('',#62274,#32400,#32401);
#26278=AXIS2_PLACEMENT_3D('',#62275,#32402,#32403);
#26279=AXIS2_PLACEMENT_3D('',#62277,#32404,#32405);
#26280=AXIS2_PLACEMENT_3D('',#62279,#32407,#32408);
#26281=AXIS2_PLACEMENT_3D('',#62280,#32409,#32410);
#26282=AXIS2_PLACEMENT_3D('',#62281,#32411,#32412);
#26283=AXIS2_PLACEMENT_3D('',#62282,#32413,#32414);
#26284=AXIS2_PLACEMENT_3D('',#62284,#32415,#32416);
#26285=AXIS2_PLACEMENT_3D('',#62287,#32418,#32419);
#26286=AXIS2_PLACEMENT_3D('',#62288,#32420,#32421);
#26287=AXIS2_PLACEMENT_3D('',#62290,#32422,#32423);
#26288=AXIS2_PLACEMENT_3D('',#62293,#32425,#32426);
#26289=AXIS2_PLACEMENT_3D('',#62294,#32427,#32428);
#26290=AXIS2_PLACEMENT_3D('',#62295,#32429,#32430);
#26291=AXIS2_PLACEMENT_3D('',#62296,#32431,#32432);
#26292=AXIS2_PLACEMENT_3D('',#62297,#32433,#32434);
#26293=AXIS2_PLACEMENT_3D('',#62301,#32436,#32437);
#26294=AXIS2_PLACEMENT_3D('',#62302,#32438,#32439);
#26295=AXIS2_PLACEMENT_3D('',#62314,#32440,#32441);
#26296=AXIS2_PLACEMENT_3D('',#62376,#32443,#32444);
#26297=AXIS2_PLACEMENT_3D('',#62378,#32446,#32447);
#26298=AXIS2_PLACEMENT_3D('',#62380,#32448,#32449);
#26299=AXIS2_PLACEMENT_3D('',#62383,#32451,#32452);
#26300=AXIS2_PLACEMENT_3D('',#62384,#32453,#32454);
#26301=AXIS2_PLACEMENT_3D('',#62386,#32455,#32456);
#26302=AXIS2_PLACEMENT_3D('',#62389,#32458,#32459);
#26303=AXIS2_PLACEMENT_3D('',#62390,#32460,#32461);
#26304=AXIS2_PLACEMENT_3D('',#62391,#32462,#32463);
#26305=AXIS2_PLACEMENT_3D('',#62392,#32464,#32465);
#26306=AXIS2_PLACEMENT_3D('',#62393,#32466,#32467);
#26307=AXIS2_PLACEMENT_3D('',#62395,#32468,#32469);
#26308=AXIS2_PLACEMENT_3D('',#62398,#32471,#32472);
#26309=AXIS2_PLACEMENT_3D('',#62399,#32473,#32474);
#26310=AXIS2_PLACEMENT_3D('',#62403,#32476,#32477);
#26311=AXIS2_PLACEMENT_3D('',#62404,#32478,#32479);
#26312=AXIS2_PLACEMENT_3D('',#62414,#32480,#32481);
#26313=AXIS2_PLACEMENT_3D('',#62470,#32483,#32484);
#26314=AXIS2_PLACEMENT_3D('',#62472,#32486,#32487);
#26315=AXIS2_PLACEMENT_3D('',#62485,#32494,#32495);
#26316=AXIS2_PLACEMENT_3D('',#62491,#32499,#32500);
#26317=AXIS2_PLACEMENT_3D('',#62501,#32506,#32507);
#26318=AXIS2_PLACEMENT_3D('',#62503,#32508,#32509);
#26319=AXIS2_PLACEMENT_3D('',#62504,#32510,#32511);
#26320=AXIS2_PLACEMENT_3D('',#62505,#32512,#32513);
#26321=AXIS2_PLACEMENT_3D('',#62507,#32514,#32515);
#26322=AXIS2_PLACEMENT_3D('',#62508,#32516,#32517);
#26323=AXIS2_PLACEMENT_3D('',#62509,#32518,#32519);
#26324=AXIS2_PLACEMENT_3D('',#62511,#32521,#32522);
#26325=AXIS2_PLACEMENT_3D('',#62512,#32523,#32524);
#26326=AXIS2_PLACEMENT_3D('',#62513,#32525,#32526);
#26327=AXIS2_PLACEMENT_3D('',#62514,#32527,#32528);
#26328=AXIS2_PLACEMENT_3D('',#62515,#32529,#32530);
#26329=AXIS2_PLACEMENT_3D('',#62516,#32531,#32532);
#26330=AXIS2_PLACEMENT_3D('',#62517,#32533,#32534);
#26331=AXIS2_PLACEMENT_3D('',#62519,#32535,#32536);
#26332=AXIS2_PLACEMENT_3D('',#62522,#32538,#32539);
#26333=AXIS2_PLACEMENT_3D('',#62523,#32540,#32541);
#26334=AXIS2_PLACEMENT_3D('',#62525,#32542,#32543);
#26335=AXIS2_PLACEMENT_3D('',#62528,#32545,#32546);
#26336=AXIS2_PLACEMENT_3D('',#62529,#32547,#32548);
#26337=AXIS2_PLACEMENT_3D('',#62530,#32549,#32550);
#26338=AXIS2_PLACEMENT_3D('',#62531,#32551,#32552);
#26339=AXIS2_PLACEMENT_3D('',#62532,#32553,#32554);
#26340=AXIS2_PLACEMENT_3D('',#62534,#32555,#32556);
#26341=AXIS2_PLACEMENT_3D('',#62537,#32558,#32559);
#26342=AXIS2_PLACEMENT_3D('',#62538,#32560,#32561);
#26343=AXIS2_PLACEMENT_3D('',#62540,#32562,#32563);
#26344=AXIS2_PLACEMENT_3D('',#62543,#32565,#32566);
#26345=AXIS2_PLACEMENT_3D('',#62544,#32567,#32568);
#26346=AXIS2_PLACEMENT_3D('',#62545,#32569,#32570);
#26347=AXIS2_PLACEMENT_3D('',#62546,#32571,#32572);
#26348=AXIS2_PLACEMENT_3D('',#62547,#32573,#32574);
#26349=AXIS2_PLACEMENT_3D('',#62564,#32583,#32584);
#26350=AXIS2_PLACEMENT_3D('',#62570,#32588,#32589);
#26351=AXIS2_PLACEMENT_3D('',#62574,#32592,#32593);
#26352=AXIS2_PLACEMENT_3D('',#62578,#32596,#32597);
#26353=AXIS2_PLACEMENT_3D('',#62582,#32600,#32601);
#26354=AXIS2_PLACEMENT_3D('',#62590,#32606,#32607);
#26355=AXIS2_PLACEMENT_3D('',#62592,#32609,#32610);
#26356=AXIS2_PLACEMENT_3D('',#62594,#32612,#32613);
#26357=AXIS2_PLACEMENT_3D('',#62596,#32615,#32616);
#26358=AXIS2_PLACEMENT_3D('',#62597,#32617,#32618);
#26359=AXIS2_PLACEMENT_3D('',#62598,#32619,#32620);
#26360=AXIS2_PLACEMENT_3D('',#62607,#32625,#32626);
#26361=AXIS2_PLACEMENT_3D('',#62613,#32630,#32631);
#26362=AXIS2_PLACEMENT_3D('',#62619,#32635,#32636);
#26363=AXIS2_PLACEMENT_3D('',#62625,#32640,#32641);
#26364=AXIS2_PLACEMENT_3D('',#62631,#32645,#32646);
#26365=AXIS2_PLACEMENT_3D('',#62634,#32649,#32650);
#26366=AXIS2_PLACEMENT_3D('',#62635,#32651,#32652);
#26367=AXIS2_PLACEMENT_3D('',#62637,#32653,#32654);
#26368=AXIS2_PLACEMENT_3D('',#62638,#32655,#32656);
#26369=AXIS2_PLACEMENT_3D('',#62640,#32657,#32658);
#26370=AXIS2_PLACEMENT_3D('',#62642,#32660,#32661);
#26371=AXIS2_PLACEMENT_3D('',#62644,#32662,#32663);
#26372=AXIS2_PLACEMENT_3D('',#62646,#32665,#32666);
#26373=AXIS2_PLACEMENT_3D('',#62648,#32667,#32668);
#26374=AXIS2_PLACEMENT_3D('',#62650,#32670,#32671);
#26375=AXIS2_PLACEMENT_3D('',#62651,#32672,#32673);
#26376=AXIS2_PLACEMENT_3D('',#62652,#32674,#32675);
#26377=AXIS2_PLACEMENT_3D('',#62654,#32676,#32677);
#26378=AXIS2_PLACEMENT_3D('',#62657,#32679,#32680);
#26379=AXIS2_PLACEMENT_3D('',#62658,#32681,#32682);
#26380=AXIS2_PLACEMENT_3D('',#62660,#32683,#32684);
#26381=AXIS2_PLACEMENT_3D('',#62663,#32686,#32687);
#26382=AXIS2_PLACEMENT_3D('',#62664,#32688,#32689);
#26383=AXIS2_PLACEMENT_3D('',#62665,#32690,#32691);
#26384=AXIS2_PLACEMENT_3D('',#62666,#32692,#32693);
#26385=AXIS2_PLACEMENT_3D('',#62667,#32694,#32695);
#26386=AXIS2_PLACEMENT_3D('',#62669,#32696,#32697);
#26387=AXIS2_PLACEMENT_3D('',#62670,#32698,#32699);
#26388=AXIS2_PLACEMENT_3D('',#62672,#32700,#32701);
#26389=AXIS2_PLACEMENT_3D('',#62674,#32703,#32704);
#26390=AXIS2_PLACEMENT_3D('',#62676,#32705,#32706);
#26391=AXIS2_PLACEMENT_3D('',#62678,#32708,#32709);
#26392=AXIS2_PLACEMENT_3D('',#62680,#32710,#32711);
#26393=AXIS2_PLACEMENT_3D('',#62682,#32713,#32714);
#26394=AXIS2_PLACEMENT_3D('',#62684,#32715,#32716);
#26395=AXIS2_PLACEMENT_3D('',#62685,#32717,#32718);
#26396=AXIS2_PLACEMENT_3D('',#62687,#32719,#32720);
#26397=AXIS2_PLACEMENT_3D('',#62689,#32722,#32723);
#26398=AXIS2_PLACEMENT_3D('',#62691,#32724,#32725);
#26399=AXIS2_PLACEMENT_3D('',#62693,#32727,#32728);
#26400=AXIS2_PLACEMENT_3D('',#62695,#32729,#32730);
#26401=AXIS2_PLACEMENT_3D('',#62697,#32732,#32733);
#26402=AXIS2_PLACEMENT_3D('',#62698,#32734,#32735);
#26403=AXIS2_PLACEMENT_3D('',#62707,#32740,#32741);
#26404=AXIS2_PLACEMENT_3D('',#62713,#32745,#32746);
#26405=AXIS2_PLACEMENT_3D('',#62719,#32750,#32751);
#26406=AXIS2_PLACEMENT_3D('',#62725,#32755,#32756);
#26407=AXIS2_PLACEMENT_3D('',#62731,#32760,#32761);
#26408=AXIS2_PLACEMENT_3D('',#62734,#32764,#32765);
#26409=AXIS2_PLACEMENT_3D('',#62735,#32766,#32767);
#26410=AXIS2_PLACEMENT_3D('',#62736,#32768,#32769);
#26411=AXIS2_PLACEMENT_3D('',#62737,#32770,#32771);
#26412=AXIS2_PLACEMENT_3D('',#62738,#32772,#32773);
#26413=AXIS2_PLACEMENT_3D('',#62739,#32774,#32775);
#26414=AXIS2_PLACEMENT_3D('',#62740,#32776,#32777);
#26415=AXIS2_PLACEMENT_3D('',#62741,#32778,#32779);
#26416=AXIS2_PLACEMENT_3D('',#62742,#32780,#32781);
#26417=AXIS2_PLACEMENT_3D('',#62743,#32782,#32783);
#26418=AXIS2_PLACEMENT_3D('',#62744,#32784,#32785);
#26419=AXIS2_PLACEMENT_3D('',#62745,#32786,#32787);
#26420=AXIS2_PLACEMENT_3D('',#62746,#32788,#32789);
#26421=AXIS2_PLACEMENT_3D('',#62747,#32790,#32791);
#26422=AXIS2_PLACEMENT_3D('',#62748,#32792,#32793);
#26423=AXIS2_PLACEMENT_3D('',#62749,#32794,#32795);
#26424=AXIS2_PLACEMENT_3D('',#62750,#32796,#32797);
#26425=AXIS2_PLACEMENT_3D('',#62751,#32798,#32799);
#26426=AXIS2_PLACEMENT_3D('',#62752,#32800,#32801);
#26427=AXIS2_PLACEMENT_3D('',#62753,#32802,#32803);
#26428=AXIS2_PLACEMENT_3D('',#62754,#32804,#32805);
#26429=AXIS2_PLACEMENT_3D('',#62755,#32806,#32807);
#26430=AXIS2_PLACEMENT_3D('',#62756,#32808,#32809);
#26431=AXIS2_PLACEMENT_3D('',#62757,#32810,#32811);
#26432=AXIS2_PLACEMENT_3D('',#62758,#32812,#32813);
#26433=AXIS2_PLACEMENT_3D('',#62759,#32814,#32815);
#26434=AXIS2_PLACEMENT_3D('',#62760,#32816,#32817);
#26435=AXIS2_PLACEMENT_3D('',#62761,#32818,#32819);
#26436=AXIS2_PLACEMENT_3D('',#62762,#32820,#32821);
#26437=AXIS2_PLACEMENT_3D('',#62763,#32822,#32823);
#26438=AXIS2_PLACEMENT_3D('',#62764,#32824,#32825);
#26439=AXIS2_PLACEMENT_3D('',#62765,#32826,#32827);
#26440=AXIS2_PLACEMENT_3D('',#62766,#32828,#32829);
#26441=AXIS2_PLACEMENT_3D('',#62767,#32830,#32831);
#26442=AXIS2_PLACEMENT_3D('',#62768,#32832,#32833);
#26443=AXIS2_PLACEMENT_3D('',#62769,#32834,#32835);
#26444=AXIS2_PLACEMENT_3D('',#62770,#32836,#32837);
#26445=AXIS2_PLACEMENT_3D('',#62771,#32838,#32839);
#26446=AXIS2_PLACEMENT_3D('',#62772,#32840,#32841);
#26447=AXIS2_PLACEMENT_3D('',#62773,#32842,#32843);
#26448=AXIS2_PLACEMENT_3D('',#62774,#32844,#32845);
#26449=AXIS2_PLACEMENT_3D('',#62775,#32846,#32847);
#26450=AXIS2_PLACEMENT_3D('',#62776,#32848,#32849);
#26451=AXIS2_PLACEMENT_3D('',#62777,#32850,#32851);
#26452=AXIS2_PLACEMENT_3D('',#62778,#32852,#32853);
#26453=AXIS2_PLACEMENT_3D('',#62779,#32854,#32855);
#26454=AXIS2_PLACEMENT_3D('',#62780,#32856,#32857);
#26455=AXIS2_PLACEMENT_3D('',#62781,#32858,#32859);
#26456=AXIS2_PLACEMENT_3D('',#62782,#32860,#32861);
#26457=AXIS2_PLACEMENT_3D('',#62783,#32862,#32863);
#26458=AXIS2_PLACEMENT_3D('',#62784,#32864,#32865);
#26459=AXIS2_PLACEMENT_3D('',#62785,#32866,#32867);
#26460=AXIS2_PLACEMENT_3D('',#62786,#32868,#32869);
#26461=DIRECTION('axis',(0.,0.,1.));
#26462=DIRECTION('refdir',(1.,0.,0.));
#26463=DIRECTION('axis',(0.,0.,1.));
#26464=DIRECTION('refdir',(1.,0.,0.));
#26465=DIRECTION('axis',(0.,0.,1.));
#26466=DIRECTION('refdir',(1.,0.,0.));
#26467=DIRECTION('axis',(0.,0.,1.));
#26468=DIRECTION('refdir',(1.,0.,0.));
#26469=DIRECTION('center_axis',(0.,0.,1.));
#26470=DIRECTION('ref_axis',(1.,0.,0.));
#26471=DIRECTION('center_axis',(0.,0.,1.));
#26472=DIRECTION('ref_axis',(1.,0.,0.));
#26473=DIRECTION('',(0.,0.,1.));
#26474=DIRECTION('center_axis',(0.,0.,-1.));
#26475=DIRECTION('ref_axis',(1.,0.,0.));
#26476=DIRECTION('center_axis',(0.,0.,1.));
#26477=DIRECTION('ref_axis',(1.,0.,0.));
#26478=DIRECTION('center_axis',(0.,0.,1.));
#26479=DIRECTION('ref_axis',(1.,0.,0.));
#26480=DIRECTION('',(0.,0.,1.));
#26481=DIRECTION('center_axis',(0.,0.,-1.));
#26482=DIRECTION('ref_axis',(1.,0.,0.));
#26483=DIRECTION('center_axis',(0.,0.,1.));
#26484=DIRECTION('ref_axis',(1.,0.,0.));
#26485=DIRECTION('center_axis',(0.,0.,1.));
#26486=DIRECTION('ref_axis',(1.,0.,0.));
#26487=DIRECTION('',(0.,0.,1.));
#26488=DIRECTION('center_axis',(0.,0.,-1.));
#26489=DIRECTION('ref_axis',(1.,0.,0.));
#26490=DIRECTION('center_axis',(0.,0.,1.));
#26491=DIRECTION('ref_axis',(1.,0.,0.));
#26492=DIRECTION('center_axis',(0.,0.,1.));
#26493=DIRECTION('ref_axis',(1.,0.,0.));
#26494=DIRECTION('',(0.,0.,1.));
#26495=DIRECTION('center_axis',(0.,0.,-1.));
#26496=DIRECTION('ref_axis',(1.,0.,0.));
#26497=DIRECTION('center_axis',(0.,0.,1.));
#26498=DIRECTION('ref_axis',(1.,0.,0.));
#26499=DIRECTION('center_axis',(0.,0.,1.));
#26500=DIRECTION('ref_axis',(1.,0.,0.));
#26501=DIRECTION('',(0.,0.,1.));
#26502=DIRECTION('center_axis',(0.,0.,-1.));
#26503=DIRECTION('ref_axis',(1.,0.,0.));
#26504=DIRECTION('center_axis',(0.,0.,1.));
#26505=DIRECTION('ref_axis',(1.,0.,0.));
#26506=DIRECTION('center_axis',(0.,0.,1.));
#26507=DIRECTION('ref_axis',(1.,0.,0.));
#26508=DIRECTION('',(0.,0.,1.));
#26509=DIRECTION('center_axis',(0.,0.,-1.));
#26510=DIRECTION('ref_axis',(1.,0.,0.));
#26511=DIRECTION('center_axis',(0.,0.,1.));
#26512=DIRECTION('ref_axis',(1.,0.,0.));
#26513=DIRECTION('center_axis',(0.,0.,1.));
#26514=DIRECTION('ref_axis',(1.,0.,0.));
#26515=DIRECTION('',(0.,0.,1.));
#26516=DIRECTION('center_axis',(0.,0.,-1.));
#26517=DIRECTION('ref_axis',(1.,0.,0.));
#26518=DIRECTION('center_axis',(0.,0.,1.));
#26519=DIRECTION('ref_axis',(1.,0.,0.));
#26520=DIRECTION('center_axis',(0.,0.,1.));
#26521=DIRECTION('ref_axis',(1.,0.,0.));
#26522=DIRECTION('',(0.,0.,1.));
#26523=DIRECTION('center_axis',(0.,0.,-1.));
#26524=DIRECTION('ref_axis',(1.,0.,0.));
#26525=DIRECTION('center_axis',(0.,0.,1.));
#26526=DIRECTION('ref_axis',(1.,0.,0.));
#26527=DIRECTION('center_axis',(0.,0.,1.));
#26528=DIRECTION('ref_axis',(1.,0.,0.));
#26529=DIRECTION('',(0.,0.,1.));
#26530=DIRECTION('center_axis',(0.,0.,-1.));
#26531=DIRECTION('ref_axis',(1.,0.,0.));
#26532=DIRECTION('center_axis',(0.,0.,1.));
#26533=DIRECTION('ref_axis',(1.,0.,0.));
#26534=DIRECTION('center_axis',(0.,0.,1.));
#26535=DIRECTION('ref_axis',(1.,0.,0.));
#26536=DIRECTION('',(0.,0.,1.));
#26537=DIRECTION('center_axis',(0.,0.,-1.));
#26538=DIRECTION('ref_axis',(1.,0.,0.));
#26539=DIRECTION('center_axis',(0.,1.,0.));
#26540=DIRECTION('ref_axis',(-1.,0.,0.));
#26541=DIRECTION('',(-1.,0.,0.));
#26542=DIRECTION('',(0.,0.,1.));
#26543=DIRECTION('',(-1.,0.,0.));
#26544=DIRECTION('',(0.,0.,1.));
#26545=DIRECTION('center_axis',(1.,0.,0.));
#26546=DIRECTION('ref_axis',(0.,1.,0.));
#26547=DIRECTION('',(0.,1.,0.));
#26548=DIRECTION('',(0.,1.,0.));
#26549=DIRECTION('',(0.,0.,1.));
#26550=DIRECTION('center_axis',(0.,-1.,0.));
#26551=DIRECTION('ref_axis',(1.,0.,0.));
#26552=DIRECTION('',(1.,0.,0.));
#26553=DIRECTION('',(1.,0.,0.));
#26554=DIRECTION('',(0.,0.,1.));
#26555=DIRECTION('center_axis',(-1.,0.,0.));
#26556=DIRECTION('ref_axis',(0.,-1.,0.));
#26557=DIRECTION('',(0.,-1.,0.));
#26558=DIRECTION('',(0.,-1.,0.));
#26559=DIRECTION('center_axis',(0.,0.,1.));
#26560=DIRECTION('ref_axis',(1.,0.,0.));
#26561=DIRECTION('center_axis',(0.,0.,1.));
#26562=DIRECTION('ref_axis',(1.,0.,0.));
#26563=DIRECTION('axis',(0.,0.,1.));
#26564=DIRECTION('refdir',(1.,0.,0.));
#26565=DIRECTION('center_axis',(0.,1.,0.));
#26566=DIRECTION('ref_axis',(-1.,0.,0.));
#26567=DIRECTION('',(-1.,0.,0.));
#26568=DIRECTION('',(0.,0.,1.));
#26569=DIRECTION('',(-1.,0.,0.));
#26570=DIRECTION('',(0.,0.,1.));
#26571=DIRECTION('center_axis',(1.,0.,0.));
#26572=DIRECTION('ref_axis',(0.,1.,0.));
#26573=DIRECTION('',(0.,1.,0.));
#26574=DIRECTION('',(0.,1.,0.));
#26575=DIRECTION('',(0.,0.,1.));
#26576=DIRECTION('center_axis',(0.,-1.,0.));
#26577=DIRECTION('ref_axis',(1.,0.,0.));
#26578=DIRECTION('',(1.,0.,0.));
#26579=DIRECTION('',(1.,0.,0.));
#26580=DIRECTION('',(0.,0.,1.));
#26581=DIRECTION('center_axis',(-1.,0.,0.));
#26582=DIRECTION('ref_axis',(0.,-1.,0.));
#26583=DIRECTION('',(0.,-1.,0.));
#26584=DIRECTION('',(0.,-1.,0.));
#26585=DIRECTION('center_axis',(0.,0.,1.));
#26586=DIRECTION('ref_axis',(1.,0.,0.));
#26587=DIRECTION('center_axis',(0.,0.,1.));
#26588=DIRECTION('ref_axis',(1.,0.,0.));
#26589=DIRECTION('axis',(0.,0.,1.));
#26590=DIRECTION('refdir',(1.,0.,0.));
#26591=DIRECTION('center_axis',(0.,1.,0.));
#26592=DIRECTION('ref_axis',(-1.,0.,0.));
#26593=DIRECTION('',(-1.,0.,0.));
#26594=DIRECTION('',(0.,0.,1.));
#26595=DIRECTION('',(-1.,0.,0.));
#26596=DIRECTION('',(0.,0.,1.));
#26597=DIRECTION('center_axis',(1.,0.,0.));
#26598=DIRECTION('ref_axis',(0.,1.,0.));
#26599=DIRECTION('',(0.,1.,0.));
#26600=DIRECTION('',(0.,1.,0.));
#26601=DIRECTION('',(0.,0.,1.));
#26602=DIRECTION('center_axis',(0.,-1.,0.));
#26603=DIRECTION('ref_axis',(1.,0.,0.));
#26604=DIRECTION('',(1.,0.,0.));
#26605=DIRECTION('',(1.,0.,0.));
#26606=DIRECTION('',(0.,0.,1.));
#26607=DIRECTION('center_axis',(-1.,0.,0.));
#26608=DIRECTION('ref_axis',(0.,-1.,0.));
#26609=DIRECTION('',(0.,-1.,0.));
#26610=DIRECTION('',(0.,-1.,0.));
#26611=DIRECTION('center_axis',(0.,0.,1.));
#26612=DIRECTION('ref_axis',(1.,0.,0.));
#26613=DIRECTION('center_axis',(0.,0.,1.));
#26614=DIRECTION('ref_axis',(1.,0.,0.));
#26615=DIRECTION('axis',(0.,0.,1.));
#26616=DIRECTION('refdir',(1.,0.,0.));
#26617=DIRECTION('center_axis',(0.,0.,1.));
#26618=DIRECTION('ref_axis',(1.,0.,0.));
#26619=DIRECTION('',(0.,0.,1.));
#26620=DIRECTION('center_axis',(0.,0.,1.));
#26621=DIRECTION('ref_axis',(1.,0.,0.));
#26622=DIRECTION('',(0.,0.,1.));
#26623=DIRECTION('center_axis',(0.,0.,-1.));
#26624=DIRECTION('ref_axis',(1.,0.,0.));
#26625=DIRECTION('center_axis',(0.,0.,1.));
#26626=DIRECTION('ref_axis',(1.,0.,0.));
#26627=DIRECTION('',(0.,0.,1.));
#26628=DIRECTION('center_axis',(0.,0.,1.));
#26629=DIRECTION('ref_axis',(1.,0.,0.));
#26630=DIRECTION('',(0.,0.,1.));
#26631=DIRECTION('center_axis',(0.,0.,-1.));
#26632=DIRECTION('ref_axis',(1.,0.,0.));
#26633=DIRECTION('center_axis',(0.,0.,1.));
#26634=DIRECTION('ref_axis',(1.,0.,0.));
#26635=DIRECTION('center_axis',(0.,0.,1.));
#26636=DIRECTION('ref_axis',(1.,0.,0.));
#26637=DIRECTION('',(0.,0.,1.));
#26638=DIRECTION('center_axis',(0.,0.,-1.));
#26639=DIRECTION('ref_axis',(1.,0.,0.));
#26640=DIRECTION('center_axis',(0.,0.,1.));
#26641=DIRECTION('ref_axis',(1.,0.,0.));
#26642=DIRECTION('center_axis',(0.,0.,1.));
#26643=DIRECTION('ref_axis',(1.,0.,0.));
#26644=DIRECTION('',(0.,0.,1.));
#26645=DIRECTION('center_axis',(0.,0.,-1.));
#26646=DIRECTION('ref_axis',(1.,0.,0.));
#26647=DIRECTION('center_axis',(0.,0.,1.));
#26648=DIRECTION('ref_axis',(1.,0.,0.));
#26649=DIRECTION('center_axis',(0.,0.,1.));
#26650=DIRECTION('ref_axis',(1.,0.,0.));
#26651=DIRECTION('',(0.,0.,1.));
#26652=DIRECTION('center_axis',(0.,0.,-1.));
#26653=DIRECTION('ref_axis',(1.,0.,0.));
#26654=DIRECTION('center_axis',(0.,0.,1.));
#26655=DIRECTION('ref_axis',(1.,0.,0.));
#26656=DIRECTION('center_axis',(0.,0.,1.));
#26657=DIRECTION('ref_axis',(1.,0.,0.));
#26658=DIRECTION('',(0.,0.,1.));
#26659=DIRECTION('center_axis',(0.,0.,-1.));
#26660=DIRECTION('ref_axis',(1.,0.,0.));
#26661=DIRECTION('center_axis',(0.,0.,1.));
#26662=DIRECTION('ref_axis',(1.,0.,0.));
#26663=DIRECTION('center_axis',(0.,0.,1.));
#26664=DIRECTION('ref_axis',(1.,0.,0.));
#26665=DIRECTION('',(0.,0.,1.));
#26666=DIRECTION('center_axis',(0.,0.,-1.));
#26667=DIRECTION('ref_axis',(1.,0.,0.));
#26668=DIRECTION('center_axis',(0.,0.,1.));
#26669=DIRECTION('ref_axis',(1.,0.,0.));
#26670=DIRECTION('center_axis',(0.,0.,1.));
#26671=DIRECTION('ref_axis',(1.,0.,0.));
#26672=DIRECTION('center_axis',(0.,0.,1.));
#26673=DIRECTION('ref_axis',(1.,0.,0.));
#26674=DIRECTION('center_axis',(0.,0.,-1.));
#26675=DIRECTION('ref_axis',(1.,0.,0.));
#26676=DIRECTION('',(0.,0.,1.));
#26677=DIRECTION('center_axis',(0.,0.,1.));
#26678=DIRECTION('ref_axis',(1.,0.,0.));
#26679=DIRECTION('center_axis',(0.,0.,1.));
#26680=DIRECTION('ref_axis',(1.,0.,0.));
#26681=DIRECTION('center_axis',(0.,0.,1.));
#26682=DIRECTION('ref_axis',(1.,0.,0.));
#26683=DIRECTION('center_axis',(0.,0.,1.));
#26684=DIRECTION('ref_axis',(1.,0.,0.));
#26685=DIRECTION('center_axis',(0.,0.,1.));
#26686=DIRECTION('ref_axis',(1.,0.,0.));
#26687=DIRECTION('',(0.,0.,1.));
#26688=DIRECTION('center_axis',(0.,0.,-1.));
#26689=DIRECTION('ref_axis',(1.,0.,0.));
#26690=DIRECTION('center_axis',(0.,0.,1.));
#26691=DIRECTION('ref_axis',(1.,0.,0.));
#26692=DIRECTION('center_axis',(0.,0.,1.));
#26693=DIRECTION('ref_axis',(1.,0.,0.));
#26694=DIRECTION('center_axis',(0.,0.,1.));
#26695=DIRECTION('ref_axis',(1.,0.,0.));
#26696=DIRECTION('center_axis',(0.,0.,-1.));
#26697=DIRECTION('ref_axis',(1.,0.,0.));
#26698=DIRECTION('',(0.,0.,1.));
#26699=DIRECTION('center_axis',(0.,0.,1.));
#26700=DIRECTION('ref_axis',(1.,0.,0.));
#26701=DIRECTION('center_axis',(0.,0.,1.));
#26702=DIRECTION('ref_axis',(1.,0.,0.));
#26703=DIRECTION('center_axis',(0.,0.,1.));
#26704=DIRECTION('ref_axis',(1.,0.,0.));
#26705=DIRECTION('center_axis',(0.,0.,1.));
#26706=DIRECTION('ref_axis',(1.,0.,0.));
#26707=DIRECTION('',(0.,-1.,0.));
#26708=DIRECTION('',(1.,0.,0.));
#26709=DIRECTION('',(0.,1.,0.));
#26710=DIRECTION('',(-1.,0.,0.));
#26711=DIRECTION('',(-1.,0.,0.));
#26712=DIRECTION('',(-1.,0.,0.));
#26713=DIRECTION('center_axis',(0.,0.,1.));
#26714=DIRECTION('ref_axis',(1.,0.,0.));
#26715=DIRECTION('center_axis',(0.,0.,1.));
#26716=DIRECTION('ref_axis',(1.,0.,0.));
#26717=DIRECTION('',(0.,0.,1.));
#26718=DIRECTION('center_axis',(0.,0.,1.));
#26719=DIRECTION('ref_axis',(1.,0.,0.));
#26720=DIRECTION('center_axis',(0.,0.,1.));
#26721=DIRECTION('ref_axis',(1.,0.,0.));
#26722=DIRECTION('',(0.,0.,1.));
#26723=DIRECTION('center_axis',(0.,0.,1.));
#26724=DIRECTION('ref_axis',(1.,0.,0.));
#26725=DIRECTION('center_axis',(0.,0.,1.));
#26726=DIRECTION('ref_axis',(1.,0.,0.));
#26727=DIRECTION('',(0.,0.,1.));
#26728=DIRECTION('center_axis',(0.,0.,1.));
#26729=DIRECTION('ref_axis',(1.,0.,0.));
#26730=DIRECTION('center_axis',(0.,0.,1.));
#26731=DIRECTION('ref_axis',(1.,0.,0.));
#26732=DIRECTION('',(0.,0.,1.));
#26733=DIRECTION('center_axis',(0.,1.,0.));
#26734=DIRECTION('ref_axis',(-1.,0.,0.));
#26735=DIRECTION('',(-1.,0.,0.));
#26736=DIRECTION('',(0.,0.,1.));
#26737=DIRECTION('',(0.,0.,1.));
#26738=DIRECTION('center_axis',(1.,0.,0.));
#26739=DIRECTION('ref_axis',(0.,1.,0.));
#26740=DIRECTION('',(0.,1.,0.));
#26741=DIRECTION('',(0.,0.,1.));
#26742=DIRECTION('center_axis',(0.,-1.,0.));
#26743=DIRECTION('ref_axis',(1.,0.,0.));
#26744=DIRECTION('',(1.,0.,0.));
#26745=DIRECTION('',(0.,0.,1.));
#26746=DIRECTION('center_axis',(-1.,0.,0.));
#26747=DIRECTION('ref_axis',(0.,-1.,0.));
#26748=DIRECTION('',(0.,-1.,0.));
#26749=DIRECTION('center_axis',(0.,0.,1.));
#26750=DIRECTION('ref_axis',(1.,0.,0.));
#26751=DIRECTION('axis',(0.,0.,1.));
#26752=DIRECTION('refdir',(1.,0.,0.));
#26753=DIRECTION('center_axis',(1.,0.,0.));
#26754=DIRECTION('ref_axis',(0.,0.,-1.));
#26755=DIRECTION('center_axis',(1.,0.,0.));
#26756=DIRECTION('ref_axis',(0.,0.,-1.));
#26757=DIRECTION('',(1.,0.,0.));
#26758=DIRECTION('center_axis',(-1.,0.,0.));
#26759=DIRECTION('ref_axis',(0.,0.,-1.));
#26760=DIRECTION('center_axis',(1.,0.,0.));
#26761=DIRECTION('ref_axis',(0.,0.,-1.));
#26762=DIRECTION('center_axis',(1.,0.,0.));
#26763=DIRECTION('ref_axis',(0.,0.,-1.));
#26764=DIRECTION('',(1.,0.,0.));
#26765=DIRECTION('center_axis',(-1.,0.,0.));
#26766=DIRECTION('ref_axis',(0.,0.,-1.));
#26767=DIRECTION('center_axis',(1.,0.,0.));
#26768=DIRECTION('ref_axis',(0.,0.,-1.));
#26769=DIRECTION('center_axis',(1.,0.,0.));
#26770=DIRECTION('ref_axis',(0.,0.,-1.));
#26771=DIRECTION('',(1.,0.,0.));
#26772=DIRECTION('center_axis',(-1.,0.,0.));
#26773=DIRECTION('ref_axis',(0.,0.,-1.));
#26774=DIRECTION('center_axis',(1.,0.,0.));
#26775=DIRECTION('ref_axis',(0.,0.,-1.));
#26776=DIRECTION('center_axis',(1.,0.,0.));
#26777=DIRECTION('ref_axis',(0.,0.,-1.));
#26778=DIRECTION('',(1.,0.,0.));
#26779=DIRECTION('center_axis',(1.,0.,0.));
#26780=DIRECTION('ref_axis',(0.,0.,-1.));
#26781=DIRECTION('center_axis',(1.,0.,0.));
#26782=DIRECTION('ref_axis',(0.,0.,-1.));
#26783=DIRECTION('center_axis',(-1.,0.,0.));
#26784=DIRECTION('ref_axis',(0.,0.,-1.));
#26785=DIRECTION('center_axis',(1.,0.,0.));
#26786=DIRECTION('ref_axis',(0.,0.,-1.));
#26787=DIRECTION('',(1.,0.,0.));
#26788=DIRECTION('center_axis',(-1.,0.,0.));
#26789=DIRECTION('ref_axis',(0.,0.,-1.));
#26790=DIRECTION('center_axis',(0.,0.,1.));
#26791=DIRECTION('ref_axis',(1.,0.,0.));
#26792=DIRECTION('center_axis',(0.,0.,1.));
#26793=DIRECTION('ref_axis',(1.,0.,0.));
#26794=DIRECTION('',(0.,0.,1.));
#26795=DIRECTION('center_axis',(0.,0.,1.));
#26796=DIRECTION('ref_axis',(1.,0.,0.));
#26797=DIRECTION('center_axis',(0.,0.,1.));
#26798=DIRECTION('ref_axis',(1.,0.,0.));
#26799=DIRECTION('center_axis',(0.,0.,1.));
#26800=DIRECTION('ref_axis',(1.,0.,0.));
#26801=DIRECTION('center_axis',(0.,0.,1.));
#26802=DIRECTION('ref_axis',(1.,0.,0.));
#26803=DIRECTION('',(0.,0.,1.));
#26804=DIRECTION('center_axis',(0.,0.,1.));
#26805=DIRECTION('ref_axis',(1.,0.,0.));
#26806=DIRECTION('center_axis',(0.,0.,1.));
#26807=DIRECTION('ref_axis',(1.,0.,0.));
#26808=DIRECTION('center_axis',(0.,1.,0.));
#26809=DIRECTION('ref_axis',(-1.,0.,0.));
#26810=DIRECTION('',(-1.,0.,0.));
#26811=DIRECTION('',(0.,0.,1.));
#26812=DIRECTION('',(-1.,0.,0.));
#26813=DIRECTION('',(0.,0.,1.));
#26814=DIRECTION('center_axis',(1.,0.,0.));
#26815=DIRECTION('ref_axis',(0.,1.,0.));
#26816=DIRECTION('',(0.,1.,0.));
#26817=DIRECTION('',(0.,1.,0.));
#26818=DIRECTION('',(0.,0.,1.));
#26819=DIRECTION('center_axis',(0.,-1.,0.));
#26820=DIRECTION('ref_axis',(1.,0.,0.));
#26821=DIRECTION('',(1.,0.,0.));
#26822=DIRECTION('',(1.,0.,0.));
#26823=DIRECTION('',(0.,0.,1.));
#26824=DIRECTION('center_axis',(-1.,0.,0.));
#26825=DIRECTION('ref_axis',(0.,-1.,0.));
#26826=DIRECTION('',(0.,-1.,0.));
#26827=DIRECTION('',(0.,-1.,0.));
#26828=DIRECTION('center_axis',(0.,0.,1.));
#26829=DIRECTION('ref_axis',(1.,0.,0.));
#26830=DIRECTION('center_axis',(0.,0.,1.));
#26831=DIRECTION('ref_axis',(1.,0.,0.));
#26832=DIRECTION('axis',(0.,0.,1.));
#26833=DIRECTION('refdir',(1.,0.,0.));
#26834=DIRECTION('center_axis',(1.,0.,0.));
#26835=DIRECTION('ref_axis',(0.,0.,-1.));
#26836=DIRECTION('center_axis',(1.,0.,0.));
#26837=DIRECTION('ref_axis',(0.,0.,-1.));
#26838=DIRECTION('',(1.,0.,0.));
#26839=DIRECTION('center_axis',(-1.,0.,0.));
#26840=DIRECTION('ref_axis',(0.,0.,-1.));
#26841=DIRECTION('center_axis',(1.,0.,0.));
#26842=DIRECTION('ref_axis',(0.,0.,-1.));
#26843=DIRECTION('center_axis',(1.,0.,0.));
#26844=DIRECTION('ref_axis',(0.,0.,-1.));
#26845=DIRECTION('',(1.,0.,0.));
#26846=DIRECTION('center_axis',(-1.,0.,0.));
#26847=DIRECTION('ref_axis',(0.,0.,-1.));
#26848=DIRECTION('center_axis',(1.,0.,0.));
#26849=DIRECTION('ref_axis',(0.,0.,-1.));
#26850=DIRECTION('center_axis',(1.,0.,0.));
#26851=DIRECTION('ref_axis',(0.,0.,-1.));
#26852=DIRECTION('',(1.,0.,0.));
#26853=DIRECTION('center_axis',(-1.,0.,0.));
#26854=DIRECTION('ref_axis',(0.,0.,-1.));
#26855=DIRECTION('center_axis',(1.,0.,0.));
#26856=DIRECTION('ref_axis',(0.,0.,-1.));
#26857=DIRECTION('center_axis',(1.,0.,0.));
#26858=DIRECTION('ref_axis',(0.,0.,-1.));
#26859=DIRECTION('',(-1.,0.,0.));
#26860=DIRECTION('center_axis',(-1.,0.,0.));
#26861=DIRECTION('ref_axis',(0.,0.,-1.));
#26862=DIRECTION('center_axis',(1.,0.,0.));
#26863=DIRECTION('ref_axis',(0.,0.,-1.));
#26864=DIRECTION('center_axis',(-1.,0.,0.));
#26865=DIRECTION('ref_axis',(0.,0.,-1.));
#26866=DIRECTION('center_axis',(1.,0.,0.));
#26867=DIRECTION('ref_axis',(0.,0.,-1.));
#26868=DIRECTION('',(-1.,0.,0.));
#26869=DIRECTION('center_axis',(-1.,0.,0.));
#26870=DIRECTION('ref_axis',(0.,0.,-1.));
#26871=DIRECTION('center_axis',(1.,0.,0.));
#26872=DIRECTION('ref_axis',(0.,0.,-1.));
#26873=DIRECTION('center_axis',(1.,0.,0.));
#26874=DIRECTION('ref_axis',(0.,0.,-1.));
#26875=DIRECTION('',(-1.,0.,0.));
#26876=DIRECTION('center_axis',(1.,0.,0.));
#26877=DIRECTION('ref_axis',(0.,0.,-1.));
#26878=DIRECTION('center_axis',(1.,0.,0.));
#26879=DIRECTION('ref_axis',(0.,0.,-1.));
#26880=DIRECTION('center_axis',(1.,0.,0.));
#26881=DIRECTION('ref_axis',(0.,0.,-1.));
#26882=DIRECTION('axis',(0.,0.,1.));
#26883=DIRECTION('refdir',(1.,0.,0.));
#26884=DIRECTION('center_axis',(1.,0.,0.));
#26885=DIRECTION('ref_axis',(0.,0.,-1.));
#26886=DIRECTION('center_axis',(1.,0.,0.));
#26887=DIRECTION('ref_axis',(0.,0.,-1.));
#26888=DIRECTION('',(1.,0.,0.));
#26889=DIRECTION('center_axis',(-1.,0.,0.));
#26890=DIRECTION('ref_axis',(0.,0.,-1.));
#26891=DIRECTION('center_axis',(1.,0.,0.));
#26892=DIRECTION('ref_axis',(0.,0.,-1.));
#26893=DIRECTION('center_axis',(1.,0.,0.));
#26894=DIRECTION('ref_axis',(0.,0.,-1.));
#26895=DIRECTION('',(1.,0.,0.));
#26896=DIRECTION('center_axis',(-1.,0.,0.));
#26897=DIRECTION('ref_axis',(0.,0.,-1.));
#26898=DIRECTION('center_axis',(1.,0.,0.));
#26899=DIRECTION('ref_axis',(0.,0.,-1.));
#26900=DIRECTION('center_axis',(1.,0.,0.));
#26901=DIRECTION('ref_axis',(0.,0.,-1.));
#26902=DIRECTION('',(1.,0.,0.));
#26903=DIRECTION('center_axis',(-1.,0.,0.));
#26904=DIRECTION('ref_axis',(0.,0.,-1.));
#26905=DIRECTION('center_axis',(1.,0.,0.));
#26906=DIRECTION('ref_axis',(0.,0.,-1.));
#26907=DIRECTION('center_axis',(1.,0.,0.));
#26908=DIRECTION('ref_axis',(0.,0.,-1.));
#26909=DIRECTION('',(1.,0.,0.));
#26910=DIRECTION('center_axis',(-1.,0.,0.));
#26911=DIRECTION('ref_axis',(0.,0.,-1.));
#26912=DIRECTION('center_axis',(1.,0.,0.));
#26913=DIRECTION('ref_axis',(0.,0.,-1.));
#26914=DIRECTION('center_axis',(1.,0.,0.));
#26915=DIRECTION('ref_axis',(0.,0.,-1.));
#26916=DIRECTION('center_axis',(1.,0.,0.));
#26917=DIRECTION('ref_axis',(0.,0.,-1.));
#26918=DIRECTION('center_axis',(1.,0.,0.));
#26919=DIRECTION('ref_axis',(0.,0.,-1.));
#26920=DIRECTION('',(1.,0.,0.));
#26921=DIRECTION('center_axis',(0.,0.,1.));
#26922=DIRECTION('ref_axis',(1.,0.,0.));
#26923=DIRECTION('center_axis',(0.,0.,1.));
#26924=DIRECTION('ref_axis',(1.,0.,0.));
#26925=DIRECTION('',(0.,0.,1.));
#26926=DIRECTION('center_axis',(0.,0.,1.));
#26927=DIRECTION('ref_axis',(1.,0.,0.));
#26928=DIRECTION('center_axis',(0.,0.,1.));
#26929=DIRECTION('ref_axis',(1.,0.,0.));
#26930=DIRECTION('center_axis',(0.,0.,1.));
#26931=DIRECTION('ref_axis',(1.,0.,0.));
#26932=DIRECTION('center_axis',(0.,0.,1.));
#26933=DIRECTION('ref_axis',(1.,0.,0.));
#26934=DIRECTION('',(0.,0.,1.));
#26935=DIRECTION('center_axis',(0.,0.,1.));
#26936=DIRECTION('ref_axis',(1.,0.,0.));
#26937=DIRECTION('center_axis',(0.,0.,1.));
#26938=DIRECTION('ref_axis',(1.,0.,0.));
#26939=DIRECTION('center_axis',(0.,1.,0.));
#26940=DIRECTION('ref_axis',(-1.,0.,0.));
#26941=DIRECTION('',(-1.,0.,0.));
#26942=DIRECTION('',(0.,0.,1.));
#26943=DIRECTION('',(-1.,0.,0.));
#26944=DIRECTION('',(0.,0.,1.));
#26945=DIRECTION('center_axis',(1.,0.,0.));
#26946=DIRECTION('ref_axis',(0.,1.,0.));
#26947=DIRECTION('',(0.,1.,0.));
#26948=DIRECTION('',(0.,1.,0.));
#26949=DIRECTION('',(0.,0.,1.));
#26950=DIRECTION('center_axis',(0.,-1.,0.));
#26951=DIRECTION('ref_axis',(1.,0.,0.));
#26952=DIRECTION('',(1.,0.,0.));
#26953=DIRECTION('',(1.,0.,0.));
#26954=DIRECTION('',(0.,0.,1.));
#26955=DIRECTION('center_axis',(-1.,0.,0.));
#26956=DIRECTION('ref_axis',(0.,-1.,0.));
#26957=DIRECTION('',(0.,-1.,0.));
#26958=DIRECTION('',(0.,-1.,0.));
#26959=DIRECTION('center_axis',(0.,0.,1.));
#26960=DIRECTION('ref_axis',(1.,0.,0.));
#26961=DIRECTION('center_axis',(0.,0.,1.));
#26962=DIRECTION('ref_axis',(1.,0.,0.));
#26963=DIRECTION('axis',(0.,0.,1.));
#26964=DIRECTION('refdir',(1.,0.,0.));
#26965=DIRECTION('center_axis',(1.,0.,0.));
#26966=DIRECTION('ref_axis',(0.,0.,-1.));
#26967=DIRECTION('center_axis',(1.,0.,0.));
#26968=DIRECTION('ref_axis',(0.,0.,-1.));
#26969=DIRECTION('',(1.,0.,0.));
#26970=DIRECTION('center_axis',(-1.,0.,0.));
#26971=DIRECTION('ref_axis',(0.,0.,-1.));
#26972=DIRECTION('center_axis',(1.,0.,0.));
#26973=DIRECTION('ref_axis',(0.,0.,-1.));
#26974=DIRECTION('center_axis',(1.,0.,0.));
#26975=DIRECTION('ref_axis',(0.,0.,-1.));
#26976=DIRECTION('',(1.,0.,0.));
#26977=DIRECTION('center_axis',(-1.,0.,0.));
#26978=DIRECTION('ref_axis',(0.,0.,-1.));
#26979=DIRECTION('center_axis',(1.,0.,0.));
#26980=DIRECTION('ref_axis',(0.,0.,-1.));
#26981=DIRECTION('center_axis',(1.,0.,0.));
#26982=DIRECTION('ref_axis',(0.,0.,-1.));
#26983=DIRECTION('',(1.,0.,0.));
#26984=DIRECTION('center_axis',(-1.,0.,0.));
#26985=DIRECTION('ref_axis',(0.,0.,-1.));
#26986=DIRECTION('center_axis',(0.,0.,1.));
#26987=DIRECTION('ref_axis',(0.,-1.,0.));
#26988=DIRECTION('',(1.,0.,0.));
#26989=DIRECTION('',(0.,-1.,0.));
#26990=DIRECTION('',(-1.,0.,0.));
#26991=DIRECTION('',(0.,1.,0.));
#26992=DIRECTION('center_axis',(1.,0.,0.));
#26993=DIRECTION('ref_axis',(0.,0.,-1.));
#26994=DIRECTION('center_axis',(1.,0.,0.));
#26995=DIRECTION('ref_axis',(0.,0.,-1.));
#26996=DIRECTION('center_axis',(1.,0.,0.));
#26997=DIRECTION('ref_axis',(0.,0.,-1.));
#26998=DIRECTION('center_axis',(1.,0.,0.));
#26999=DIRECTION('ref_axis',(0.,1.22464679914735E-16,1.));
#27000=DIRECTION('center_axis',(1.,0.,0.));
#27001=DIRECTION('ref_axis',(0.,0.,-1.));
#27002=DIRECTION('center_axis',(1.,0.,0.));
#27003=DIRECTION('ref_axis',(0.,0.,-1.));
#27004=DIRECTION('',(-1.,0.,0.));
#27005=DIRECTION('center_axis',(1.,0.,0.));
#27006=DIRECTION('ref_axis',(0.,0.,-1.));
#27007=DIRECTION('center_axis',(1.,0.,0.));
#27008=DIRECTION('ref_axis',(0.,0.,-1.));
#27009=DIRECTION('center_axis',(-1.,0.,0.));
#27010=DIRECTION('ref_axis',(0.,0.,-1.));
#27011=DIRECTION('center_axis',(1.,0.,0.));
#27012=DIRECTION('ref_axis',(0.,0.,-1.));
#27013=DIRECTION('center_axis',(-1.,0.,0.));
#27014=DIRECTION('ref_axis',(0.,0.,-1.));
#27015=DIRECTION('',(-1.,0.,0.));
#27016=DIRECTION('center_axis',(1.,0.,0.));
#27017=DIRECTION('ref_axis',(0.,0.,-1.));
#27018=DIRECTION('axis',(0.,0.,1.));
#27019=DIRECTION('refdir',(1.,0.,0.));
#27020=DIRECTION('center_axis',(0.,0.,1.));
#27021=DIRECTION('ref_axis',(1.,0.,0.));
#27022=DIRECTION('center_axis',(0.,0.,1.));
#27023=DIRECTION('ref_axis',(1.,0.,0.));
#27024=DIRECTION('',(0.,0.,1.));
#27025=DIRECTION('center_axis',(0.,0.,-1.));
#27026=DIRECTION('ref_axis',(1.,0.,0.));
#27027=DIRECTION('center_axis',(0.,0.,1.));
#27028=DIRECTION('ref_axis',(1.,0.,0.));
#27029=DIRECTION('center_axis',(0.,0.,1.));
#27030=DIRECTION('ref_axis',(1.,0.,0.));
#27031=DIRECTION('center_axis',(0.,0.,1.));
#27032=DIRECTION('ref_axis',(1.,0.,0.));
#27033=DIRECTION('center_axis',(0.,0.,1.));
#27034=DIRECTION('ref_axis',(1.,0.,0.));
#27035=DIRECTION('',(0.,0.,1.));
#27036=DIRECTION('center_axis',(0.,1.,0.));
#27037=DIRECTION('ref_axis',(-1.,0.,0.));
#27038=DIRECTION('',(-1.,0.,0.));
#27039=DIRECTION('',(0.,0.,1.));
#27040=DIRECTION('',(-1.,0.,0.));
#27041=DIRECTION('',(0.,0.,1.));
#27042=DIRECTION('center_axis',(1.,0.,0.));
#27043=DIRECTION('ref_axis',(0.,1.,0.));
#27044=DIRECTION('',(0.,1.,0.));
#27045=DIRECTION('',(0.,1.,0.));
#27046=DIRECTION('',(0.,0.,1.));
#27047=DIRECTION('center_axis',(0.,-1.,0.));
#27048=DIRECTION('ref_axis',(1.,0.,0.));
#27049=DIRECTION('',(1.,0.,0.));
#27050=DIRECTION('',(1.,0.,0.));
#27051=DIRECTION('',(0.,0.,1.));
#27052=DIRECTION('center_axis',(-1.,0.,0.));
#27053=DIRECTION('ref_axis',(0.,-1.,0.));
#27054=DIRECTION('',(0.,-1.,0.));
#27055=DIRECTION('',(0.,-1.,0.));
#27056=DIRECTION('center_axis',(0.,0.,1.));
#27057=DIRECTION('ref_axis',(1.,0.,0.));
#27058=DIRECTION('center_axis',(0.,0.,1.));
#27059=DIRECTION('ref_axis',(1.,0.,0.));
#27060=DIRECTION('axis',(0.,0.,1.));
#27061=DIRECTION('refdir',(1.,0.,0.));
#27062=DIRECTION('center_axis',(0.,0.,1.));
#27063=DIRECTION('ref_axis',(1.,0.,0.));
#27064=DIRECTION('center_axis',(0.,0.,1.));
#27065=DIRECTION('ref_axis',(1.,0.,0.));
#27066=DIRECTION('',(0.,0.,1.));
#27067=DIRECTION('center_axis',(0.,0.,-1.));
#27068=DIRECTION('ref_axis',(1.,0.,0.));
#27069=DIRECTION('center_axis',(0.,0.,1.));
#27070=DIRECTION('ref_axis',(1.,0.,0.));
#27071=DIRECTION('center_axis',(0.,0.,1.));
#27072=DIRECTION('ref_axis',(1.,0.,0.));
#27073=DIRECTION('center_axis',(0.,0.,1.));
#27074=DIRECTION('ref_axis',(1.,0.,0.));
#27075=DIRECTION('center_axis',(0.,0.,1.));
#27076=DIRECTION('ref_axis',(1.,0.,0.));
#27077=DIRECTION('',(0.,0.,1.));
#27078=DIRECTION('center_axis',(0.,1.,0.));
#27079=DIRECTION('ref_axis',(-1.,0.,0.));
#27080=DIRECTION('',(-1.,0.,0.));
#27081=DIRECTION('',(0.,0.,1.));
#27082=DIRECTION('',(-1.,0.,0.));
#27083=DIRECTION('',(0.,0.,1.));
#27084=DIRECTION('center_axis',(1.,0.,0.));
#27085=DIRECTION('ref_axis',(0.,1.,0.));
#27086=DIRECTION('',(0.,1.,0.));
#27087=DIRECTION('',(0.,1.,0.));
#27088=DIRECTION('',(0.,0.,1.));
#27089=DIRECTION('center_axis',(0.,-1.,0.));
#27090=DIRECTION('ref_axis',(1.,0.,0.));
#27091=DIRECTION('',(1.,0.,0.));
#27092=DIRECTION('',(1.,0.,0.));
#27093=DIRECTION('',(0.,0.,1.));
#27094=DIRECTION('center_axis',(-1.,0.,0.));
#27095=DIRECTION('ref_axis',(0.,-1.,0.));
#27096=DIRECTION('',(0.,-1.,0.));
#27097=DIRECTION('',(0.,-1.,0.));
#27098=DIRECTION('center_axis',(0.,0.,1.));
#27099=DIRECTION('ref_axis',(1.,0.,0.));
#27100=DIRECTION('center_axis',(0.,0.,1.));
#27101=DIRECTION('ref_axis',(1.,0.,0.));
#27102=DIRECTION('axis',(0.,0.,1.));
#27103=DIRECTION('refdir',(1.,0.,0.));
#27104=DIRECTION('center_axis',(0.,0.,1.));
#27105=DIRECTION('ref_axis',(1.,0.,0.));
#27106=DIRECTION('center_axis',(0.,0.,1.));
#27107=DIRECTION('ref_axis',(1.,0.,0.));
#27108=DIRECTION('',(0.,0.,1.));
#27109=DIRECTION('center_axis',(0.,0.,-1.));
#27110=DIRECTION('ref_axis',(1.,0.,0.));
#27111=DIRECTION('center_axis',(0.,0.,1.));
#27112=DIRECTION('ref_axis',(1.,0.,0.));
#27113=DIRECTION('center_axis',(0.,0.,1.));
#27114=DIRECTION('ref_axis',(1.,0.,0.));
#27115=DIRECTION('center_axis',(0.,0.,1.));
#27116=DIRECTION('ref_axis',(1.,0.,0.));
#27117=DIRECTION('center_axis',(0.,0.,1.));
#27118=DIRECTION('ref_axis',(1.,0.,0.));
#27119=DIRECTION('',(0.,0.,1.));
#27120=DIRECTION('center_axis',(0.,0.,-1.));
#27121=DIRECTION('ref_axis',(1.,0.,0.));
#27122=DIRECTION('center_axis',(0.,0.,1.));
#27123=DIRECTION('ref_axis',(1.,0.,0.));
#27124=DIRECTION('center_axis',(0.,0.,1.));
#27125=DIRECTION('ref_axis',(1.,0.,0.));
#27126=DIRECTION('center_axis',(0.,0.,1.));
#27127=DIRECTION('ref_axis',(1.,0.,0.));
#27128=DIRECTION('center_axis',(0.,0.,1.));
#27129=DIRECTION('ref_axis',(1.,0.,0.));
#27130=DIRECTION('',(0.,0.,1.));
#27131=DIRECTION('center_axis',(0.,0.,-1.));
#27132=DIRECTION('ref_axis',(1.,0.,0.));
#27133=DIRECTION('center_axis',(0.,0.,1.));
#27134=DIRECTION('ref_axis',(1.,0.,0.));
#27135=DIRECTION('center_axis',(0.,0.,1.));
#27136=DIRECTION('ref_axis',(1.,0.,0.));
#27137=DIRECTION('center_axis',(0.,0.,1.));
#27138=DIRECTION('ref_axis',(1.,0.,0.));
#27139=DIRECTION('center_axis',(0.,0.,1.));
#27140=DIRECTION('ref_axis',(1.,0.,0.));
#27141=DIRECTION('',(0.,0.,1.));
#27142=DIRECTION('center_axis',(0.,0.,-1.));
#27143=DIRECTION('ref_axis',(1.,0.,0.));
#27144=DIRECTION('center_axis',(0.,0.,1.));
#27145=DIRECTION('ref_axis',(1.,0.,0.));
#27146=DIRECTION('center_axis',(0.,0.,1.));
#27147=DIRECTION('ref_axis',(1.,0.,0.));
#27148=DIRECTION('center_axis',(0.,0.,1.));
#27149=DIRECTION('ref_axis',(1.,0.,0.));
#27150=DIRECTION('center_axis',(0.,0.,1.));
#27151=DIRECTION('ref_axis',(1.,0.,0.));
#27152=DIRECTION('',(0.,0.,1.));
#27153=DIRECTION('center_axis',(0.,0.,1.));
#27154=DIRECTION('ref_axis',(1.,0.,0.));
#27155=DIRECTION('center_axis',(0.,0.,1.));
#27156=DIRECTION('ref_axis',(1.,0.,0.));
#27157=DIRECTION('',(0.,0.,1.));
#27158=DIRECTION('center_axis',(0.,0.,1.));
#27159=DIRECTION('ref_axis',(1.,0.,0.));
#27160=DIRECTION('center_axis',(0.,0.,1.));
#27161=DIRECTION('ref_axis',(1.,0.,0.));
#27162=DIRECTION('',(0.,0.,1.));
#27163=DIRECTION('center_axis',(0.,0.,1.));
#27164=DIRECTION('ref_axis',(1.,0.,0.));
#27165=DIRECTION('center_axis',(0.,0.,1.));
#27166=DIRECTION('ref_axis',(1.,0.,0.));
#27167=DIRECTION('',(0.,0.,1.));
#27168=DIRECTION('center_axis',(0.,-0.56333682464151,0.826227342807548));
#27169=DIRECTION('ref_axis',(0.,-0.826227342807548,-0.56333682464151));
#27170=DIRECTION('',(0.,-0.826227342807548,-0.56333682464151));
#27171=DIRECTION('',(1.,0.,0.));
#27172=DIRECTION('',(0.,-0.826227342807548,-0.56333682464151));
#27173=DIRECTION('',(1.,0.,0.));
#27174=DIRECTION('center_axis',(0.,-1.,0.));
#27175=DIRECTION('ref_axis',(0.,0.,-1.));
#27176=DIRECTION('',(0.,0.,-1.));
#27177=DIRECTION('',(0.,0.,-1.));
#27178=DIRECTION('',(1.,0.,0.));
#27179=DIRECTION('center_axis',(0.,-0.56333682464151,-0.826227342807548));
#27180=DIRECTION('ref_axis',(0.,0.826227342807548,-0.56333682464151));
#27181=DIRECTION('',(0.,0.826227342807548,-0.56333682464151));
#27182=DIRECTION('',(0.,0.826227342807548,-0.56333682464151));
#27183=DIRECTION('',(1.,0.,0.));
#27184=DIRECTION('center_axis',(0.,-1.,0.));
#27185=DIRECTION('ref_axis',(0.,0.,-1.));
#27186=DIRECTION('',(0.,0.,-1.));
#27187=DIRECTION('',(0.,0.,-1.));
#27188=DIRECTION('',(1.,0.,0.));
#27189=DIRECTION('center_axis',(0.,0.,1.));
#27190=DIRECTION('ref_axis',(0.,-1.,0.));
#27191=DIRECTION('',(0.,-1.,0.));
#27192=DIRECTION('',(0.,-1.,0.));
#27193=DIRECTION('',(1.,0.,0.));
#27194=DIRECTION('center_axis',(0.,1.,0.));
#27195=DIRECTION('ref_axis',(0.,0.,1.));
#27196=DIRECTION('',(0.,0.,1.));
#27197=DIRECTION('',(0.,0.,1.));
#27198=DIRECTION('',(1.,0.,0.));
#27199=DIRECTION('center_axis',(0.,0.56333682464151,-0.826227342807548));
#27200=DIRECTION('ref_axis',(0.,0.826227342807548,0.56333682464151));
#27201=DIRECTION('',(0.,0.826227342807548,0.56333682464151));
#27202=DIRECTION('',(0.,0.826227342807548,0.56333682464151));
#27203=DIRECTION('',(1.,0.,0.));
#27204=DIRECTION('center_axis',(0.,1.,0.));
#27205=DIRECTION('ref_axis',(0.,0.,1.));
#27206=DIRECTION('',(0.,0.,1.));
#27207=DIRECTION('',(0.,0.,1.));
#27208=DIRECTION('',(1.,0.,0.));
#27209=DIRECTION('center_axis',(0.,0.56333682464151,0.826227342807548));
#27210=DIRECTION('ref_axis',(0.,-0.826227342807548,0.56333682464151));
#27211=DIRECTION('',(0.,-0.826227342807548,0.56333682464151));
#27212=DIRECTION('',(0.,-0.826227342807548,0.56333682464151));
#27213=DIRECTION('',(1.,0.,0.));
#27214=DIRECTION('center_axis',(0.,1.,0.));
#27215=DIRECTION('ref_axis',(0.,0.,1.));
#27216=DIRECTION('',(0.,0.,1.));
#27217=DIRECTION('',(0.,0.,1.));
#27218=DIRECTION('',(1.,0.,0.));
#27219=DIRECTION('center_axis',(0.,0.,-1.));
#27220=DIRECTION('ref_axis',(0.,1.,0.));
#27221=DIRECTION('',(0.,1.,0.));
#27222=DIRECTION('',(0.,1.,0.));
#27223=DIRECTION('',(1.,0.,0.));
#27224=DIRECTION('center_axis',(0.,-1.,0.));
#27225=DIRECTION('ref_axis',(0.,0.,-1.));
#27226=DIRECTION('',(0.,0.,-1.));
#27227=DIRECTION('',(0.,0.,-1.));
#27228=DIRECTION('center_axis',(1.,0.,0.));
#27229=DIRECTION('ref_axis',(0.,0.,-1.));
#27230=DIRECTION('center_axis',(1.,0.,0.));
#27231=DIRECTION('ref_axis',(0.,0.,-1.));
#27232=DIRECTION('axis',(0.,0.,1.));
#27233=DIRECTION('refdir',(1.,0.,0.));
#27234=DIRECTION('axis',(0.,0.,1.));
#27235=DIRECTION('refdir',(1.,0.,0.));
#27236=DIRECTION('center_axis',(0.,-1.,0.));
#27237=DIRECTION('ref_axis',(0.,0.,-1.));
#27238=DIRECTION('center_axis',(0.,-1.,0.));
#27239=DIRECTION('ref_axis',(1.,0.,0.));
#27240=DIRECTION('center_axis',(0.,-1.,0.));
#27241=DIRECTION('ref_axis',(1.,0.,0.));
#27242=DIRECTION('center_axis',(1.,0.,1.22464679914735E-16));
#27243=DIRECTION('ref_axis',(-1.22464679914735E-16,0.,1.));
#27244=DIRECTION('center_axis',(0.,1.,0.));
#27245=DIRECTION('ref_axis',(1.,0.,0.));
#27246=DIRECTION('center_axis',(0.,1.,0.));
#27247=DIRECTION('ref_axis',(1.,0.,0.));
#27248=DIRECTION('center_axis',(0.,-1.,0.));
#27249=DIRECTION('ref_axis',(1.,0.,0.));
#27250=DIRECTION('',(0.,1.,0.));
#27251=DIRECTION('center_axis',(0.,-1.,0.));
#27252=DIRECTION('ref_axis',(1.,0.,0.));
#27253=DIRECTION('center_axis',(0.,-1.,0.));
#27254=DIRECTION('ref_axis',(1.,0.,0.));
#27255=DIRECTION('center_axis',(0.,-1.,0.));
#27256=DIRECTION('ref_axis',(1.,0.,0.));
#27257=DIRECTION('',(0.,1.,0.));
#27258=DIRECTION('center_axis',(0.,-1.,0.));
#27259=DIRECTION('ref_axis',(1.,0.,0.));
#27260=DIRECTION('center_axis',(0.,1.,0.));
#27261=DIRECTION('ref_axis',(1.,0.,0.));
#27262=DIRECTION('',(-0.707106781186548,0.707106781186547,-8.65956056235493E-17));
#27263=DIRECTION('center_axis',(0.,-1.,0.));
#27264=DIRECTION('ref_axis',(1.,0.,0.));
#27265=DIRECTION('center_axis',(0.,1.,0.));
#27266=DIRECTION('ref_axis',(0.,0.,1.));
#27267=DIRECTION('center_axis',(0.,-1.,0.));
#27268=DIRECTION('ref_axis',(1.,0.,0.));
#27269=DIRECTION('center_axis',(0.,-1.,0.));
#27270=DIRECTION('ref_axis',(1.,0.,0.));
#27271=DIRECTION('',(0.,1.,0.));
#27272=DIRECTION('center_axis',(0.,-1.,0.));
#27273=DIRECTION('ref_axis',(0.,0.,-1.));
#27274=DIRECTION('center_axis',(0.,-1.,0.));
#27275=DIRECTION('ref_axis',(1.,0.,0.));
#27276=DIRECTION('center_axis',(0.,-1.,0.));
#27277=DIRECTION('ref_axis',(1.,0.,0.));
#27278=DIRECTION('',(0.707106781186548,0.707106781186547,8.65956056235493E-17));
#27279=DIRECTION('axis',(0.,0.,1.));
#27280=DIRECTION('refdir',(1.,0.,0.));
#27281=DIRECTION('center_axis',(0.,-1.,0.));
#27282=DIRECTION('ref_axis',(0.,0.,-1.));
#27283=DIRECTION('center_axis',(0.,-1.,0.));
#27284=DIRECTION('ref_axis',(1.,0.,0.));
#27285=DIRECTION('center_axis',(0.,-1.,0.));
#27286=DIRECTION('ref_axis',(1.,0.,0.));
#27287=DIRECTION('center_axis',(1.,0.,1.22464679914735E-16));
#27288=DIRECTION('ref_axis',(-1.22464679914735E-16,0.,1.));
#27289=DIRECTION('center_axis',(0.,1.,0.));
#27290=DIRECTION('ref_axis',(1.,0.,0.));
#27291=DIRECTION('center_axis',(0.,1.,0.));
#27292=DIRECTION('ref_axis',(1.,0.,0.));
#27293=DIRECTION('center_axis',(0.,-1.,0.));
#27294=DIRECTION('ref_axis',(1.,0.,0.));
#27295=DIRECTION('center_axis',(0.,-1.,0.));
#27296=DIRECTION('ref_axis',(1.,0.,0.));
#27297=DIRECTION('',(0.,1.,0.));
#27298=DIRECTION('center_axis',(0.,1.,0.));
#27299=DIRECTION('ref_axis',(0.,0.,1.));
#27300=DIRECTION('center_axis',(0.,-1.,0.));
#27301=DIRECTION('ref_axis',(1.,0.,0.));
#27302=DIRECTION('center_axis',(0.,-1.,0.));
#27303=DIRECTION('ref_axis',(1.,0.,0.));
#27304=DIRECTION('center_axis',(0.,-1.,0.));
#27305=DIRECTION('ref_axis',(1.,0.,0.));
#27306=DIRECTION('center_axis',(0.,-1.,0.));
#27307=DIRECTION('ref_axis',(1.,0.,0.));
#27308=DIRECTION('',(0.707106781186548,0.707106781186547,8.65956056235494E-17));
#27309=DIRECTION('center_axis',(0.,-1.,0.));
#27310=DIRECTION('ref_axis',(1.,0.,0.));
#27311=DIRECTION('center_axis',(0.,-1.,0.));
#27312=DIRECTION('ref_axis',(1.,0.,0.));
#27313=DIRECTION('',(0.,1.,0.));
#27314=DIRECTION('center_axis',(0.,1.,0.));
#27315=DIRECTION('ref_axis',(1.,0.,0.));
#27316=DIRECTION('center_axis',(0.,-1.,0.));
#27317=DIRECTION('ref_axis',(1.,0.,0.));
#27318=DIRECTION('',(-0.707106781186548,0.707106781186547,-8.65956056235494E-17));
#27319=DIRECTION('center_axis',(0.,-1.,0.));
#27320=DIRECTION('ref_axis',(0.,0.,-1.));
#27321=DIRECTION('center_axis',(0.,-1.,0.));
#27322=DIRECTION('ref_axis',(1.,0.,0.));
#27323=DIRECTION('',(0.,1.,0.));
#27324=DIRECTION('axis',(0.,0.,1.));
#27325=DIRECTION('refdir',(1.,0.,0.));
#27326=DIRECTION('center_axis',(0.,0.,1.));
#27327=DIRECTION('ref_axis',(1.,0.,0.));
#27328=DIRECTION('center_axis',(1.22464679914735E-16,-1.,0.));
#27329=DIRECTION('ref_axis',(-1.,-1.22464679914735E-16,0.));
#27330=DIRECTION('center_axis',(0.78183148246803,0.,0.623489801858733));
#27331=DIRECTION('ref_axis',(0.623489801858734,0.,-0.78183148246803));
#27332=DIRECTION('center_axis',(7.63554790147315E-17,-1.,-9.57467422477103E-17));
#27333=DIRECTION('ref_axis',(-0.623489801858734,-1.22464679914735E-16,0.78183148246803));
#27334=DIRECTION('center_axis',(0.974927912181824,0.,-0.222520933956314));
#27335=DIRECTION('ref_axis',(-0.222520933956314,0.,-0.974927912181824));
#27336=DIRECTION('center_axis',(-2.7250954951288E-17,-1.,-1.19394234705288E-16));
#27337=DIRECTION('ref_axis',(0.222520933956314,-1.22464679914735E-16,0.974927912181824));
#27338=DIRECTION('center_axis',(0.433883739117558,0.,-0.900968867902419));
#27339=DIRECTION('ref_axis',(-0.900968867902419,0.,-0.433883739117558));
#27340=DIRECTION('center_axis',(-1.10336864020811E-16,-1.,-5.31354332312403E-17));
#27341=DIRECTION('ref_axis',(0.900968867902419,-1.22464679914735E-16,0.433883739117558));
#27342=DIRECTION('center_axis',(-0.433883739117558,0.,-0.900968867902419));
#27343=DIRECTION('ref_axis',(-0.900968867902419,0.,0.433883739117558));
#27344=DIRECTION('center_axis',(-1.10336864020811E-16,-1.,5.31354332312403E-17));
#27345=DIRECTION('ref_axis',(0.900968867902419,-1.22464679914735E-16,-0.433883739117558));
#27346=DIRECTION('center_axis',(-0.974927912181824,0.,-0.222520933956314));
#27347=DIRECTION('ref_axis',(-0.222520933956315,0.,0.974927912181824));
#27348=DIRECTION('center_axis',(-2.7250954951288E-17,-1.,1.19394234705288E-16));
#27349=DIRECTION('ref_axis',(0.222520933956315,-1.22464679914735E-16,-0.974927912181824));
#27350=DIRECTION('center_axis',(-0.78183148246803,0.,0.623489801858734));
#27351=DIRECTION('ref_axis',(0.623489801858733,0.,0.78183148246803));
#27352=DIRECTION('center_axis',(7.63554790147315E-17,-1.,9.57467422477103E-17));
#27353=DIRECTION('ref_axis',(-0.623489801858733,-1.22464679914735E-16,-0.78183148246803));
#27354=DIRECTION('axis',(0.,0.,1.));
#27355=DIRECTION('refdir',(1.,0.,0.));
#27356=DIRECTION('center_axis',(0.,0.,1.));
#27357=DIRECTION('ref_axis',(1.,0.,0.));
#27358=DIRECTION('center_axis',(0.,-1.,0.));
#27359=DIRECTION('ref_axis',(0.,0.,-1.));
#27360=DIRECTION('center_axis',(0.,-1.,0.));
#27361=DIRECTION('ref_axis',(0.,0.,-1.));
#27362=DIRECTION('center_axis',(0.,1.,0.));
#27363=DIRECTION('ref_axis',(1.,0.,0.));
#27364=DIRECTION('center_axis',(0.,1.,0.));
#27365=DIRECTION('ref_axis',(1.,0.,0.));
#27366=DIRECTION('center_axis',(0.,1.,0.));
#27367=DIRECTION('ref_axis',(1.,0.,0.));
#27368=DIRECTION('center_axis',(0.,1.,0.));
#27369=DIRECTION('ref_axis',(1.,0.,0.));
#27370=DIRECTION('',(0.,-1.,0.));
#27371=DIRECTION('center_axis',(0.,-1.,0.));
#27372=DIRECTION('ref_axis',(1.,0.,0.));
#27373=DIRECTION('center_axis',(0.,1.,0.));
#27374=DIRECTION('ref_axis',(1.,0.,0.));
#27375=DIRECTION('center_axis',(0.,1.,0.));
#27376=DIRECTION('ref_axis',(1.,0.,0.));
#27377=DIRECTION('center_axis',(0.,1.,0.));
#27378=DIRECTION('ref_axis',(1.,0.,0.));
#27379=DIRECTION('center_axis',(0.,1.,0.));
#27380=DIRECTION('ref_axis',(1.,0.,0.));
#27381=DIRECTION('center_axis',(0.,1.,0.));
#27382=DIRECTION('ref_axis',(1.,0.,0.));
#27383=DIRECTION('center_axis',(0.,1.,0.));
#27384=DIRECTION('ref_axis',(1.,0.,0.));
#27385=DIRECTION('center_axis',(0.,-1.,0.));
#27386=DIRECTION('ref_axis',(1.,0.,0.));
#27387=DIRECTION('center_axis',(0.,-1.,0.));
#27388=DIRECTION('ref_axis',(0.,0.,-1.));
#27389=DIRECTION('center_axis',(8.96625347776458E-17,0.,1.));
#27390=DIRECTION('ref_axis',(1.,0.,0.));
#27391=DIRECTION('center_axis',(0.,-1.,0.));
#27392=DIRECTION('ref_axis',(0.,0.,-1.));
#27393=DIRECTION('center_axis',(0.,1.,0.));
#27394=DIRECTION('ref_axis',(1.,0.,0.));
#27395=DIRECTION('center_axis',(0.,-1.,0.));
#27396=DIRECTION('ref_axis',(1.,0.,0.));
#27397=DIRECTION('center_axis',(0.,-1.,0.));
#27398=DIRECTION('ref_axis',(0.,0.,-1.));
#27399=DIRECTION('center_axis',(0.,0.,1.));
#27400=DIRECTION('ref_axis',(1.,0.,0.));
#27401=DIRECTION('center_axis',(0.,-1.,0.));
#27402=DIRECTION('ref_axis',(0.,0.,-1.));
#27403=DIRECTION('center_axis',(0.,1.,0.));
#27404=DIRECTION('ref_axis',(1.,0.,0.));
#27405=DIRECTION('center_axis',(0.,-1.,0.));
#27406=DIRECTION('ref_axis',(1.,0.,0.));
#27407=DIRECTION('center_axis',(0.,-1.,0.));
#27408=DIRECTION('ref_axis',(1.,0.,0.));
#27409=DIRECTION('center_axis',(0.,-1.,0.));
#27410=DIRECTION('ref_axis',(0.,0.,-1.));
#27411=DIRECTION('center_axis',(0.,0.,1.));
#27412=DIRECTION('ref_axis',(1.,0.,0.));
#27413=DIRECTION('center_axis',(0.,-1.,0.));
#27414=DIRECTION('ref_axis',(0.,0.,-1.));
#27415=DIRECTION('center_axis',(0.,1.,0.));
#27416=DIRECTION('ref_axis',(1.,0.,0.));
#27417=DIRECTION('center_axis',(0.,-1.,0.));
#27418=DIRECTION('ref_axis',(1.,0.,0.));
#27419=DIRECTION('center_axis',(0.,-1.,0.));
#27420=DIRECTION('ref_axis',(0.,0.,-1.));
#27421=DIRECTION('center_axis',(8.96625347776458E-17,0.,1.));
#27422=DIRECTION('ref_axis',(1.,0.,0.));
#27423=DIRECTION('center_axis',(0.,-1.,0.));
#27424=DIRECTION('ref_axis',(0.,0.,-1.));
#27425=DIRECTION('center_axis',(0.,1.,0.));
#27426=DIRECTION('ref_axis',(1.,0.,0.));
#27427=DIRECTION('center_axis',(0.,-1.,0.));
#27428=DIRECTION('ref_axis',(1.,0.,0.));
#27429=DIRECTION('center_axis',(0.,-1.,0.));
#27430=DIRECTION('ref_axis',(0.,0.,-1.));
#27431=DIRECTION('center_axis',(0.,0.,1.));
#27432=DIRECTION('ref_axis',(1.,0.,0.));
#27433=DIRECTION('center_axis',(0.,-1.,0.));
#27434=DIRECTION('ref_axis',(0.,0.,-1.));
#27435=DIRECTION('center_axis',(0.,1.,0.));
#27436=DIRECTION('ref_axis',(1.,0.,0.));
#27437=DIRECTION('center_axis',(0.,1.,0.));
#27438=DIRECTION('ref_axis',(1.,0.,0.));
#27439=DIRECTION('',(0.,1.,0.));
#27440=DIRECTION('center_axis',(0.,-1.,0.));
#27441=DIRECTION('ref_axis',(1.,0.,0.));
#27442=DIRECTION('center_axis',(0.,-1.,0.));
#27443=DIRECTION('ref_axis',(1.,0.,0.));
#27444=DIRECTION('center_axis',(0.,1.,0.));
#27445=DIRECTION('ref_axis',(1.,0.,0.));
#27446=DIRECTION('center_axis',(0.,-1.,0.));
#27447=DIRECTION('ref_axis',(0.,0.,-1.));
#27448=DIRECTION('center_axis',(0.,0.,1.));
#27449=DIRECTION('ref_axis',(1.,0.,0.));
#27450=DIRECTION('center_axis',(0.,-1.,0.));
#27451=DIRECTION('ref_axis',(0.,0.,-1.));
#27452=DIRECTION('center_axis',(0.,-1.,0.));
#27453=DIRECTION('ref_axis',(-1.,0.,0.));
#27454=DIRECTION('center_axis',(0.,1.,0.));
#27455=DIRECTION('ref_axis',(1.,0.,0.));
#27456=DIRECTION('axis',(0.,0.,1.));
#27457=DIRECTION('refdir',(1.,0.,0.));
#27458=DIRECTION('center_axis',(0.,1.,0.));
#27459=DIRECTION('ref_axis',(0.,0.,1.));
#27460=DIRECTION('center_axis',(0.,-1.,0.));
#27461=DIRECTION('ref_axis',(1.,0.,0.));
#27462=DIRECTION('center_axis',(0.,-1.,0.));
#27463=DIRECTION('ref_axis',(1.,0.,0.));
#27464=DIRECTION('center_axis',(0.,-1.,0.));
#27465=DIRECTION('ref_axis',(1.,0.,0.));
#27466=DIRECTION('center_axis',(0.,-1.,0.));
#27467=DIRECTION('ref_axis',(1.,0.,0.));
#27468=DIRECTION('',(0.,1.,0.));
#27469=DIRECTION('center_axis',(0.,-1.,0.));
#27470=DIRECTION('ref_axis',(0.,0.,-1.));
#27471=DIRECTION('center_axis',(0.,-1.,0.));
#27472=DIRECTION('ref_axis',(1.,0.,0.));
#27473=DIRECTION('center_axis',(0.,-1.,0.));
#27474=DIRECTION('ref_axis',(1.,0.,0.));
#27475=DIRECTION('',(0.,1.,0.));
#27476=DIRECTION('center_axis',(0.,1.,0.));
#27477=DIRECTION('ref_axis',(0.,0.,1.));
#27478=DIRECTION('center_axis',(0.,-1.,0.));
#27479=DIRECTION('ref_axis',(1.,0.,0.));
#27480=DIRECTION('center_axis',(0.,-1.,0.));
#27481=DIRECTION('ref_axis',(1.,0.,0.));
#27482=DIRECTION('center_axis',(0.,-1.,0.));
#27483=DIRECTION('ref_axis',(1.,0.,0.));
#27484=DIRECTION('center_axis',(0.,-1.,0.));
#27485=DIRECTION('ref_axis',(1.,0.,0.));
#27486=DIRECTION('',(0.,1.,0.));
#27487=DIRECTION('center_axis',(0.,-1.,0.));
#27488=DIRECTION('ref_axis',(0.,0.,-1.));
#27489=DIRECTION('center_axis',(0.,-1.,0.));
#27490=DIRECTION('ref_axis',(1.,0.,0.));
#27491=DIRECTION('center_axis',(0.,-1.,0.));
#27492=DIRECTION('ref_axis',(1.,0.,0.));
#27493=DIRECTION('',(0.,1.,0.));
#27494=DIRECTION('',(0.,0.,1.));
#27495=DIRECTION('',(1.,0.,0.));
#27496=DIRECTION('',(0.,0.,1.));
#27497=DIRECTION('',(1.,0.,0.));
#27498=DIRECTION('',(0.,0.,1.));
#27499=DIRECTION('',(1.,0.,0.));
#27500=DIRECTION('',(0.,0.,1.));
#27501=DIRECTION('',(1.,0.,0.));
#27502=DIRECTION('',(0.,0.,1.));
#27503=DIRECTION('',(1.,0.,0.));
#27504=DIRECTION('axis',(0.,0.,1.));
#27505=DIRECTION('refdir',(1.,0.,0.));
#27506=DIRECTION('axis',(0.,0.,1.));
#27507=DIRECTION('refdir',(1.,0.,0.));
#27508=DIRECTION('center_axis',(0.,-1.,0.));
#27509=DIRECTION('ref_axis',(0.,0.,-1.));
#27510=DIRECTION('center_axis',(0.,-1.,0.));
#27511=DIRECTION('ref_axis',(1.,0.,0.));
#27512=DIRECTION('center_axis',(0.,-1.,0.));
#27513=DIRECTION('ref_axis',(1.,0.,0.));
#27514=DIRECTION('center_axis',(1.,0.,1.22464679914735E-16));
#27515=DIRECTION('ref_axis',(-1.22464679914735E-16,0.,1.));
#27516=DIRECTION('center_axis',(0.,1.,0.));
#27517=DIRECTION('ref_axis',(1.,0.,0.));
#27518=DIRECTION('center_axis',(0.,1.,0.));
#27519=DIRECTION('ref_axis',(1.,0.,0.));
#27520=DIRECTION('center_axis',(0.,-1.,0.));
#27521=DIRECTION('ref_axis',(1.,0.,0.));
#27522=DIRECTION('',(0.,1.,0.));
#27523=DIRECTION('center_axis',(0.,-1.,0.));
#27524=DIRECTION('ref_axis',(1.,0.,0.));
#27525=DIRECTION('center_axis',(0.,-1.,0.));
#27526=DIRECTION('ref_axis',(1.,0.,0.));
#27527=DIRECTION('center_axis',(0.,-1.,0.));
#27528=DIRECTION('ref_axis',(1.,0.,0.));
#27529=DIRECTION('',(0.,1.,0.));
#27530=DIRECTION('center_axis',(0.,-1.,0.));
#27531=DIRECTION('ref_axis',(1.,0.,0.));
#27532=DIRECTION('center_axis',(0.,1.,0.));
#27533=DIRECTION('ref_axis',(1.,0.,0.));
#27534=DIRECTION('',(-0.707106781186548,0.707106781186547,-8.65956056235494E-17));
#27535=DIRECTION('center_axis',(0.,-1.,0.));
#27536=DIRECTION('ref_axis',(1.,0.,0.));
#27537=DIRECTION('center_axis',(0.,1.,0.));
#27538=DIRECTION('ref_axis',(0.,0.,1.));
#27539=DIRECTION('center_axis',(0.,-1.,0.));
#27540=DIRECTION('ref_axis',(1.,0.,0.));
#27541=DIRECTION('center_axis',(0.,-1.,0.));
#27542=DIRECTION('ref_axis',(1.,0.,0.));
#27543=DIRECTION('',(0.,1.,0.));
#27544=DIRECTION('center_axis',(0.,-1.,0.));
#27545=DIRECTION('ref_axis',(0.,0.,-1.));
#27546=DIRECTION('center_axis',(0.,-1.,0.));
#27547=DIRECTION('ref_axis',(1.,0.,0.));
#27548=DIRECTION('center_axis',(0.,-1.,0.));
#27549=DIRECTION('ref_axis',(1.,0.,0.));
#27550=DIRECTION('',(0.707106781186548,0.707106781186547,8.65956056235494E-17));
#27551=DIRECTION('axis',(0.,0.,1.));
#27552=DIRECTION('refdir',(1.,0.,0.));
#27553=DIRECTION('center_axis',(0.,-1.,0.));
#27554=DIRECTION('ref_axis',(0.,0.,-1.));
#27555=DIRECTION('center_axis',(0.,-1.,0.));
#27556=DIRECTION('ref_axis',(1.,0.,0.));
#27557=DIRECTION('center_axis',(0.,-1.,0.));
#27558=DIRECTION('ref_axis',(1.,0.,0.));
#27559=DIRECTION('center_axis',(1.,0.,1.22464679914735E-16));
#27560=DIRECTION('ref_axis',(-1.22464679914735E-16,0.,1.));
#27561=DIRECTION('center_axis',(0.,1.,0.));
#27562=DIRECTION('ref_axis',(1.,0.,0.));
#27563=DIRECTION('center_axis',(0.,1.,0.));
#27564=DIRECTION('ref_axis',(1.,0.,0.));
#27565=DIRECTION('center_axis',(0.,-1.,0.));
#27566=DIRECTION('ref_axis',(1.,0.,0.));
#27567=DIRECTION('center_axis',(0.,-1.,0.));
#27568=DIRECTION('ref_axis',(1.,0.,0.));
#27569=DIRECTION('',(0.,1.,0.));
#27570=DIRECTION('center_axis',(0.,1.,0.));
#27571=DIRECTION('ref_axis',(0.,0.,1.));
#27572=DIRECTION('center_axis',(0.,-1.,0.));
#27573=DIRECTION('ref_axis',(1.,0.,0.));
#27574=DIRECTION('center_axis',(0.,-1.,0.));
#27575=DIRECTION('ref_axis',(1.,0.,0.));
#27576=DIRECTION('center_axis',(0.,-1.,0.));
#27577=DIRECTION('ref_axis',(1.,0.,0.));
#27578=DIRECTION('center_axis',(0.,-1.,0.));
#27579=DIRECTION('ref_axis',(1.,0.,0.));
#27580=DIRECTION('',(0.707106781186548,0.707106781186547,8.65956056235494E-17));
#27581=DIRECTION('center_axis',(0.,-1.,0.));
#27582=DIRECTION('ref_axis',(1.,0.,0.));
#27583=DIRECTION('center_axis',(0.,-1.,0.));
#27584=DIRECTION('ref_axis',(1.,0.,0.));
#27585=DIRECTION('',(0.,1.,0.));
#27586=DIRECTION('center_axis',(0.,1.,0.));
#27587=DIRECTION('ref_axis',(1.,0.,0.));
#27588=DIRECTION('center_axis',(0.,-1.,0.));
#27589=DIRECTION('ref_axis',(1.,0.,0.));
#27590=DIRECTION('',(-0.707106781186548,0.707106781186547,-8.65956056235494E-17));
#27591=DIRECTION('center_axis',(0.,-1.,0.));
#27592=DIRECTION('ref_axis',(0.,0.,-1.));
#27593=DIRECTION('center_axis',(0.,-1.,0.));
#27594=DIRECTION('ref_axis',(1.,0.,0.));
#27595=DIRECTION('',(0.,1.,0.));
#27596=DIRECTION('axis',(0.,0.,1.));
#27597=DIRECTION('refdir',(1.,0.,0.));
#27598=DIRECTION('center_axis',(0.,0.,1.));
#27599=DIRECTION('ref_axis',(1.,0.,0.));
#27600=DIRECTION('center_axis',(1.22464679914735E-16,-1.,0.));
#27601=DIRECTION('ref_axis',(-1.,-1.22464679914735E-16,0.));
#27602=DIRECTION('center_axis',(0.707106781186548,0.,0.707106781186548));
#27603=DIRECTION('ref_axis',(0.707106781186548,0.,-0.707106781186548));
#27604=DIRECTION('center_axis',(8.65956056235493E-17,-1.,-8.65956056235493E-17));
#27605=DIRECTION('ref_axis',(-0.707106781186548,-1.22464679914735E-16,0.707106781186548));
#27606=DIRECTION('center_axis',(1.,0.,0.));
#27607=DIRECTION('ref_axis',(6.12323399573677E-17,0.,-1.));
#27608=DIRECTION('center_axis',(7.49879891330929E-33,-1.,-1.22464679914735E-16));
#27609=DIRECTION('ref_axis',(-6.12323399573677E-17,-1.22464679914735E-16,
1.));
#27610=DIRECTION('center_axis',(0.707106781186548,0.,-0.707106781186548));
#27611=DIRECTION('ref_axis',(-0.707106781186548,0.,-0.707106781186548));
#27612=DIRECTION('center_axis',(-8.65956056235493E-17,-1.,-8.65956056235493E-17));
#27613=DIRECTION('ref_axis',(0.707106781186548,-1.22464679914735E-16,0.707106781186548));
#27614=DIRECTION('center_axis',(0.,0.,-1.));
#27615=DIRECTION('ref_axis',(-1.,0.,-1.22464679914735E-16));
#27616=DIRECTION('center_axis',(-1.22464679914735E-16,-1.,-1.49975978266186E-32));
#27617=DIRECTION('ref_axis',(1.,-1.22464679914735E-16,1.22464679914735E-16));
#27618=DIRECTION('center_axis',(-0.707106781186548,0.,-0.707106781186548));
#27619=DIRECTION('ref_axis',(-0.707106781186548,0.,0.707106781186548));
#27620=DIRECTION('center_axis',(-8.65956056235493E-17,-1.,8.65956056235493E-17));
#27621=DIRECTION('ref_axis',(0.707106781186548,-1.22464679914735E-16,-0.707106781186548));
#27622=DIRECTION('center_axis',(-1.,0.,0.));
#27623=DIRECTION('ref_axis',(-1.83697019872103E-16,0.,1.));
#27624=DIRECTION('center_axis',(-2.24963967399279E-32,-1.,1.22464679914735E-16));
#27625=DIRECTION('ref_axis',(1.83697019872103E-16,-1.22464679914735E-16,
-1.));
#27626=DIRECTION('center_axis',(-0.707106781186548,0.,0.707106781186548));
#27627=DIRECTION('ref_axis',(0.707106781186548,0.,0.707106781186548));
#27628=DIRECTION('center_axis',(8.65956056235493E-17,-1.,8.65956056235494E-17));
#27629=DIRECTION('ref_axis',(-0.707106781186548,-1.22464679914735E-16,-0.707106781186548));
#27630=DIRECTION('axis',(0.,0.,1.));
#27631=DIRECTION('refdir',(1.,0.,0.));
#27632=DIRECTION('center_axis',(0.,0.,1.));
#27633=DIRECTION('ref_axis',(1.,0.,0.));
#27634=DIRECTION('center_axis',(0.,-1.,0.));
#27635=DIRECTION('ref_axis',(0.,0.,-1.));
#27636=DIRECTION('center_axis',(0.,-1.,0.));
#27637=DIRECTION('ref_axis',(0.,0.,-1.));
#27638=DIRECTION('center_axis',(0.,1.,0.));
#27639=DIRECTION('ref_axis',(1.,0.,0.));
#27640=DIRECTION('center_axis',(0.,1.,0.));
#27641=DIRECTION('ref_axis',(1.,0.,0.));
#27642=DIRECTION('center_axis',(0.,1.,0.));
#27643=DIRECTION('ref_axis',(1.,0.,0.));
#27644=DIRECTION('center_axis',(0.,1.,0.));
#27645=DIRECTION('ref_axis',(1.,0.,0.));
#27646=DIRECTION('',(0.,-1.,0.));
#27647=DIRECTION('center_axis',(0.,-1.,0.));
#27648=DIRECTION('ref_axis',(1.,0.,0.));
#27649=DIRECTION('center_axis',(0.,1.,0.));
#27650=DIRECTION('ref_axis',(1.,0.,0.));
#27651=DIRECTION('center_axis',(0.,1.,0.));
#27652=DIRECTION('ref_axis',(1.,0.,0.));
#27653=DIRECTION('center_axis',(0.,1.,0.));
#27654=DIRECTION('ref_axis',(1.,0.,0.));
#27655=DIRECTION('center_axis',(0.,1.,0.));
#27656=DIRECTION('ref_axis',(1.,0.,0.));
#27657=DIRECTION('center_axis',(0.,1.,0.));
#27658=DIRECTION('ref_axis',(1.,0.,0.));
#27659=DIRECTION('center_axis',(0.,1.,0.));
#27660=DIRECTION('ref_axis',(1.,0.,0.));
#27661=DIRECTION('center_axis',(0.,-1.,0.));
#27662=DIRECTION('ref_axis',(1.,0.,0.));
#27663=DIRECTION('center_axis',(0.,-1.,0.));
#27664=DIRECTION('ref_axis',(0.,0.,-1.));
#27665=DIRECTION('center_axis',(6.12323399573677E-17,0.,1.));
#27666=DIRECTION('ref_axis',(1.,0.,0.));
#27667=DIRECTION('center_axis',(0.,-1.,0.));
#27668=DIRECTION('ref_axis',(0.,0.,-1.));
#27669=DIRECTION('center_axis',(0.,1.,0.));
#27670=DIRECTION('ref_axis',(1.,0.,0.));
#27671=DIRECTION('center_axis',(0.,-1.,0.));
#27672=DIRECTION('ref_axis',(1.,0.,0.));
#27673=DIRECTION('center_axis',(0.,-1.,0.));
#27674=DIRECTION('ref_axis',(0.,0.,-1.));
#27675=DIRECTION('center_axis',(0.,0.,1.));
#27676=DIRECTION('ref_axis',(1.,0.,0.));
#27677=DIRECTION('center_axis',(0.,-1.,0.));
#27678=DIRECTION('ref_axis',(0.,0.,-1.));
#27679=DIRECTION('center_axis',(0.,1.,0.));
#27680=DIRECTION('ref_axis',(1.,0.,0.));
#27681=DIRECTION('center_axis',(0.,-1.,0.));
#27682=DIRECTION('ref_axis',(1.,0.,0.));
#27683=DIRECTION('center_axis',(0.,-1.,0.));
#27684=DIRECTION('ref_axis',(0.,0.,-1.));
#27685=DIRECTION('center_axis',(0.,0.,1.));
#27686=DIRECTION('ref_axis',(1.,0.,0.));
#27687=DIRECTION('center_axis',(0.,-1.,0.));
#27688=DIRECTION('ref_axis',(0.,0.,-1.));
#27689=DIRECTION('center_axis',(0.,1.,0.));
#27690=DIRECTION('ref_axis',(1.,0.,0.));
#27691=DIRECTION('center_axis',(0.,-1.,0.));
#27692=DIRECTION('ref_axis',(1.,0.,0.));
#27693=DIRECTION('center_axis',(0.,-1.,0.));
#27694=DIRECTION('ref_axis',(0.,0.,-1.));
#27695=DIRECTION('center_axis',(0.,0.,1.));
#27696=DIRECTION('ref_axis',(1.,0.,0.));
#27697=DIRECTION('center_axis',(0.,-1.,0.));
#27698=DIRECTION('ref_axis',(0.,0.,-1.));
#27699=DIRECTION('center_axis',(0.,1.,0.));
#27700=DIRECTION('ref_axis',(1.,0.,0.));
#27701=DIRECTION('center_axis',(0.,-1.,0.));
#27702=DIRECTION('ref_axis',(1.,0.,0.));
#27703=DIRECTION('center_axis',(0.,-1.,0.));
#27704=DIRECTION('ref_axis',(0.,0.,-1.));
#27705=DIRECTION('center_axis',(6.12323399573676E-17,0.,1.));
#27706=DIRECTION('ref_axis',(1.,0.,0.));
#27707=DIRECTION('center_axis',(0.,-1.,0.));
#27708=DIRECTION('ref_axis',(0.,0.,-1.));
#27709=DIRECTION('center_axis',(0.,1.,0.));
#27710=DIRECTION('ref_axis',(1.,0.,0.));
#27711=DIRECTION('center_axis',(0.,-1.,0.));
#27712=DIRECTION('ref_axis',(1.,0.,0.));
#27713=DIRECTION('center_axis',(0.,-1.,0.));
#27714=DIRECTION('ref_axis',(0.,0.,-1.));
#27715=DIRECTION('center_axis',(0.,0.,1.));
#27716=DIRECTION('ref_axis',(1.,0.,0.));
#27717=DIRECTION('center_axis',(0.,-1.,0.));
#27718=DIRECTION('ref_axis',(0.,0.,-1.));
#27719=DIRECTION('center_axis',(0.,1.,0.));
#27720=DIRECTION('ref_axis',(1.,0.,0.));
#27721=DIRECTION('center_axis',(0.,1.,0.));
#27722=DIRECTION('ref_axis',(1.,0.,0.));
#27723=DIRECTION('',(0.,1.,0.));
#27724=DIRECTION('center_axis',(0.,-1.,0.));
#27725=DIRECTION('ref_axis',(1.,0.,0.));
#27726=DIRECTION('center_axis',(0.,-1.,0.));
#27727=DIRECTION('ref_axis',(1.,0.,0.));
#27728=DIRECTION('center_axis',(0.,1.,0.));
#27729=DIRECTION('ref_axis',(1.,0.,0.));
#27730=DIRECTION('center_axis',(0.,-1.,0.));
#27731=DIRECTION('ref_axis',(0.,0.,-1.));
#27732=DIRECTION('center_axis',(0.,0.,1.));
#27733=DIRECTION('ref_axis',(1.,0.,0.));
#27734=DIRECTION('center_axis',(0.,-1.,0.));
#27735=DIRECTION('ref_axis',(0.,0.,-1.));
#27736=DIRECTION('center_axis',(0.,-1.,0.));
#27737=DIRECTION('ref_axis',(-1.,0.,0.));
#27738=DIRECTION('center_axis',(0.,1.,0.));
#27739=DIRECTION('ref_axis',(1.,0.,0.));
#27740=DIRECTION('axis',(0.,0.,1.));
#27741=DIRECTION('refdir',(1.,0.,0.));
#27742=DIRECTION('center_axis',(0.,1.,0.));
#27743=DIRECTION('ref_axis',(0.,0.,1.));
#27744=DIRECTION('center_axis',(0.,-1.,0.));
#27745=DIRECTION('ref_axis',(1.,0.,0.));
#27746=DIRECTION('center_axis',(0.,-1.,0.));
#27747=DIRECTION('ref_axis',(1.,0.,0.));
#27748=DIRECTION('center_axis',(0.,-1.,0.));
#27749=DIRECTION('ref_axis',(1.,0.,0.));
#27750=DIRECTION('center_axis',(0.,-1.,0.));
#27751=DIRECTION('ref_axis',(1.,0.,0.));
#27752=DIRECTION('',(0.,1.,0.));
#27753=DIRECTION('center_axis',(0.,-1.,0.));
#27754=DIRECTION('ref_axis',(0.,0.,-1.));
#27755=DIRECTION('center_axis',(0.,-1.,0.));
#27756=DIRECTION('ref_axis',(1.,0.,0.));
#27757=DIRECTION('center_axis',(0.,-1.,0.));
#27758=DIRECTION('ref_axis',(1.,0.,0.));
#27759=DIRECTION('',(0.,1.,0.));
#27760=DIRECTION('center_axis',(0.,1.,0.));
#27761=DIRECTION('ref_axis',(0.,0.,1.));
#27762=DIRECTION('center_axis',(0.,-1.,0.));
#27763=DIRECTION('ref_axis',(1.,0.,0.));
#27764=DIRECTION('center_axis',(0.,-1.,0.));
#27765=DIRECTION('ref_axis',(1.,0.,0.));
#27766=DIRECTION('center_axis',(0.,-1.,0.));
#27767=DIRECTION('ref_axis',(1.,0.,0.));
#27768=DIRECTION('center_axis',(0.,-1.,0.));
#27769=DIRECTION('ref_axis',(1.,0.,0.));
#27770=DIRECTION('',(0.,1.,0.));
#27771=DIRECTION('center_axis',(0.,-1.,0.));
#27772=DIRECTION('ref_axis',(0.,0.,-1.));
#27773=DIRECTION('center_axis',(0.,-1.,0.));
#27774=DIRECTION('ref_axis',(1.,0.,0.));
#27775=DIRECTION('center_axis',(0.,-1.,0.));
#27776=DIRECTION('ref_axis',(1.,0.,0.));
#27777=DIRECTION('',(0.,1.,0.));
#27778=DIRECTION('',(0.,0.,1.));
#27779=DIRECTION('',(1.,0.,0.));
#27780=DIRECTION('',(0.,0.,1.));
#27781=DIRECTION('',(1.,0.,0.));
#27782=DIRECTION('',(0.,0.,1.));
#27783=DIRECTION('',(1.,0.,0.));
#27784=DIRECTION('',(0.,0.,1.));
#27785=DIRECTION('',(1.,0.,0.));
#27786=DIRECTION('',(0.,0.,1.));
#27787=DIRECTION('',(1.,0.,0.));
#27788=DIRECTION('axis',(0.,0.,1.));
#27789=DIRECTION('refdir',(1.,0.,0.));
#27790=DIRECTION('axis',(0.,0.,1.));
#27791=DIRECTION('refdir',(1.,0.,0.));
#27792=DIRECTION('center_axis',(0.,0.,1.));
#27793=DIRECTION('ref_axis',(1.,0.,0.));
#27794=DIRECTION('center_axis',(0.,0.,1.));
#27795=DIRECTION('ref_axis',(1.,0.,0.));
#27796=DIRECTION('',(0.,0.,1.));
#27797=DIRECTION('center_axis',(0.,0.,-1.));
#27798=DIRECTION('ref_axis',(1.,0.,0.));
#27799=DIRECTION('center_axis',(0.,0.,1.));
#27800=DIRECTION('ref_axis',(1.,0.,0.));
#27801=DIRECTION('center_axis',(0.,0.,1.));
#27802=DIRECTION('ref_axis',(1.,0.,0.));
#27803=DIRECTION('',(0.,0.,1.));
#27804=DIRECTION('center_axis',(0.,0.,-1.));
#27805=DIRECTION('ref_axis',(1.,0.,0.));
#27806=DIRECTION('center_axis',(0.,0.,1.));
#27807=DIRECTION('ref_axis',(1.,0.,0.));
#27808=DIRECTION('center_axis',(0.,0.,1.));
#27809=DIRECTION('ref_axis',(1.,0.,0.));
#27810=DIRECTION('',(0.,0.,1.));
#27811=DIRECTION('center_axis',(0.,0.,-1.));
#27812=DIRECTION('ref_axis',(1.,0.,0.));
#27813=DIRECTION('center_axis',(0.,0.,1.));
#27814=DIRECTION('ref_axis',(1.,0.,0.));
#27815=DIRECTION('center_axis',(0.,0.,1.));
#27816=DIRECTION('ref_axis',(1.,0.,0.));
#27817=DIRECTION('',(0.,0.,1.));
#27818=DIRECTION('center_axis',(0.,0.,-1.));
#27819=DIRECTION('ref_axis',(1.,0.,0.));
#27820=DIRECTION('center_axis',(0.,1.,0.));
#27821=DIRECTION('ref_axis',(-1.,0.,0.));
#27822=DIRECTION('',(-1.,0.,0.));
#27823=DIRECTION('',(0.,0.,1.));
#27824=DIRECTION('',(-1.,0.,0.));
#27825=DIRECTION('',(0.,0.,1.));
#27826=DIRECTION('center_axis',(1.,0.,0.));
#27827=DIRECTION('ref_axis',(0.,1.,0.));
#27828=DIRECTION('',(0.,1.,0.));
#27829=DIRECTION('',(0.,1.,0.));
#27830=DIRECTION('',(0.,0.,1.));
#27831=DIRECTION('center_axis',(0.,-1.,0.));
#27832=DIRECTION('ref_axis',(1.,0.,0.));
#27833=DIRECTION('',(1.,0.,0.));
#27834=DIRECTION('',(1.,0.,0.));
#27835=DIRECTION('',(0.,0.,1.));
#27836=DIRECTION('center_axis',(-1.,0.,0.));
#27837=DIRECTION('ref_axis',(0.,-1.,0.));
#27838=DIRECTION('',(0.,-1.,0.));
#27839=DIRECTION('',(0.,-1.,0.));
#27840=DIRECTION('center_axis',(0.,0.,1.));
#27841=DIRECTION('ref_axis',(1.,0.,0.));
#27842=DIRECTION('center_axis',(0.,0.,1.));
#27843=DIRECTION('ref_axis',(1.,0.,0.));
#27844=DIRECTION('axis',(0.,0.,1.));
#27845=DIRECTION('refdir',(1.,0.,0.));
#27846=DIRECTION('center_axis',(0.,0.,1.));
#27847=DIRECTION('ref_axis',(1.,0.,0.));
#27848=DIRECTION('center_axis',(0.,0.,1.));
#27849=DIRECTION('ref_axis',(1.,0.,0.));
#27850=DIRECTION('',(0.,0.,1.));
#27851=DIRECTION('center_axis',(0.,0.,-1.));
#27852=DIRECTION('ref_axis',(1.,0.,0.));
#27853=DIRECTION('center_axis',(0.,0.,1.));
#27854=DIRECTION('ref_axis',(1.,0.,0.));
#27855=DIRECTION('center_axis',(0.,0.,1.));
#27856=DIRECTION('ref_axis',(1.,0.,0.));
#27857=DIRECTION('',(0.,0.,1.));
#27858=DIRECTION('center_axis',(0.,0.,-1.));
#27859=DIRECTION('ref_axis',(1.,0.,0.));
#27860=DIRECTION('center_axis',(0.,0.,1.));
#27861=DIRECTION('ref_axis',(1.,0.,0.));
#27862=DIRECTION('center_axis',(0.,0.,1.));
#27863=DIRECTION('ref_axis',(1.,0.,0.));
#27864=DIRECTION('',(0.,0.,1.));
#27865=DIRECTION('center_axis',(0.,0.,-1.));
#27866=DIRECTION('ref_axis',(1.,0.,0.));
#27867=DIRECTION('center_axis',(0.,0.,1.));
#27868=DIRECTION('ref_axis',(1.,0.,0.));
#27869=DIRECTION('center_axis',(0.,0.,1.));
#27870=DIRECTION('ref_axis',(1.,0.,0.));
#27871=DIRECTION('',(0.,0.,1.));
#27872=DIRECTION('center_axis',(0.,0.,-1.));
#27873=DIRECTION('ref_axis',(1.,0.,0.));
#27874=DIRECTION('center_axis',(0.,0.,1.));
#27875=DIRECTION('ref_axis',(1.,0.,0.));
#27876=DIRECTION('center_axis',(0.,0.,1.));
#27877=DIRECTION('ref_axis',(1.,0.,0.));
#27878=DIRECTION('',(0.,0.,1.));
#27879=DIRECTION('center_axis',(0.,0.,-1.));
#27880=DIRECTION('ref_axis',(1.,0.,0.));
#27881=DIRECTION('center_axis',(0.,0.,1.));
#27882=DIRECTION('ref_axis',(1.,0.,0.));
#27883=DIRECTION('center_axis',(0.,0.,1.));
#27884=DIRECTION('ref_axis',(1.,0.,0.));
#27885=DIRECTION('',(0.,0.,1.));
#27886=DIRECTION('center_axis',(0.,0.,-1.));
#27887=DIRECTION('ref_axis',(1.,0.,0.));
#27888=DIRECTION('center_axis',(0.,0.,1.));
#27889=DIRECTION('ref_axis',(1.,0.,0.));
#27890=DIRECTION('center_axis',(0.,0.,1.));
#27891=DIRECTION('ref_axis',(1.,0.,0.));
#27892=DIRECTION('',(0.,0.,1.));
#27893=DIRECTION('center_axis',(0.,0.,-1.));
#27894=DIRECTION('ref_axis',(1.,0.,0.));
#27895=DIRECTION('center_axis',(0.,0.,1.));
#27896=DIRECTION('ref_axis',(1.,0.,0.));
#27897=DIRECTION('center_axis',(0.,0.,1.));
#27898=DIRECTION('ref_axis',(1.,0.,0.));
#27899=DIRECTION('',(0.,0.,1.));
#27900=DIRECTION('center_axis',(0.,0.,-1.));
#27901=DIRECTION('ref_axis',(1.,0.,0.));
#27902=DIRECTION('center_axis',(0.,0.,1.));
#27903=DIRECTION('ref_axis',(1.,0.,0.));
#27904=DIRECTION('center_axis',(0.,0.,1.));
#27905=DIRECTION('ref_axis',(1.,0.,0.));
#27906=DIRECTION('',(0.,0.,1.));
#27907=DIRECTION('center_axis',(0.,0.,-1.));
#27908=DIRECTION('ref_axis',(1.,0.,0.));
#27909=DIRECTION('center_axis',(0.,0.,1.));
#27910=DIRECTION('ref_axis',(1.,0.,0.));
#27911=DIRECTION('center_axis',(0.,0.,1.));
#27912=DIRECTION('ref_axis',(1.,0.,0.));
#27913=DIRECTION('',(0.,0.,1.));
#27914=DIRECTION('center_axis',(0.,0.,-1.));
#27915=DIRECTION('ref_axis',(1.,0.,0.));
#27916=DIRECTION('center_axis',(0.,0.,1.));
#27917=DIRECTION('ref_axis',(1.,0.,0.));
#27918=DIRECTION('center_axis',(0.,0.,1.));
#27919=DIRECTION('ref_axis',(1.,0.,0.));
#27920=DIRECTION('',(0.,0.,1.));
#27921=DIRECTION('center_axis',(0.,0.,-1.));
#27922=DIRECTION('ref_axis',(1.,0.,0.));
#27923=DIRECTION('center_axis',(0.,0.,1.));
#27924=DIRECTION('ref_axis',(1.,0.,0.));
#27925=DIRECTION('center_axis',(0.,0.,1.));
#27926=DIRECTION('ref_axis',(1.,0.,0.));
#27927=DIRECTION('',(0.,0.,1.));
#27928=DIRECTION('center_axis',(0.,0.,-1.));
#27929=DIRECTION('ref_axis',(1.,0.,0.));
#27930=DIRECTION('center_axis',(0.,1.,0.));
#27931=DIRECTION('ref_axis',(-1.,0.,0.));
#27932=DIRECTION('',(-1.,0.,0.));
#27933=DIRECTION('',(0.,0.,1.));
#27934=DIRECTION('',(-1.,0.,0.));
#27935=DIRECTION('',(0.,0.,1.));
#27936=DIRECTION('center_axis',(1.,0.,0.));
#27937=DIRECTION('ref_axis',(0.,1.,0.));
#27938=DIRECTION('',(0.,1.,0.));
#27939=DIRECTION('',(0.,1.,0.));
#27940=DIRECTION('',(0.,0.,1.));
#27941=DIRECTION('center_axis',(0.,-1.,0.));
#27942=DIRECTION('ref_axis',(1.,0.,0.));
#27943=DIRECTION('',(1.,0.,0.));
#27944=DIRECTION('',(1.,0.,0.));
#27945=DIRECTION('',(0.,0.,1.));
#27946=DIRECTION('center_axis',(-1.,0.,0.));
#27947=DIRECTION('ref_axis',(0.,-1.,0.));
#27948=DIRECTION('',(0.,-1.,0.));
#27949=DIRECTION('',(0.,-1.,0.));
#27950=DIRECTION('center_axis',(0.,0.,1.));
#27951=DIRECTION('ref_axis',(1.,0.,0.));
#27952=DIRECTION('center_axis',(0.,0.,1.));
#27953=DIRECTION('ref_axis',(1.,0.,0.));
#27954=DIRECTION('axis',(0.,0.,1.));
#27955=DIRECTION('refdir',(1.,0.,0.));
#27956=DIRECTION('center_axis',(0.,0.,1.));
#27957=DIRECTION('ref_axis',(1.,0.,0.));
#27958=DIRECTION('center_axis',(0.,0.,1.));
#27959=DIRECTION('ref_axis',(1.,0.,0.));
#27960=DIRECTION('',(0.,0.,1.));
#27961=DIRECTION('center_axis',(0.,0.,-1.));
#27962=DIRECTION('ref_axis',(1.,0.,0.));
#27963=DIRECTION('center_axis',(0.,0.,1.));
#27964=DIRECTION('ref_axis',(1.,0.,0.));
#27965=DIRECTION('center_axis',(0.,0.,1.));
#27966=DIRECTION('ref_axis',(1.,0.,0.));
#27967=DIRECTION('center_axis',(0.,0.,1.));
#27968=DIRECTION('ref_axis',(1.,0.,0.));
#27969=DIRECTION('',(0.,0.,1.));
#27970=DIRECTION('center_axis',(0.,0.,-1.));
#27971=DIRECTION('ref_axis',(1.,0.,0.));
#27972=DIRECTION('center_axis',(0.,0.,1.));
#27973=DIRECTION('ref_axis',(1.,0.,0.));
#27974=DIRECTION('center_axis',(0.,0.,1.));
#27975=DIRECTION('ref_axis',(1.,0.,0.));
#27976=DIRECTION('center_axis',(0.,0.,1.));
#27977=DIRECTION('ref_axis',(1.,0.,0.));
#27978=DIRECTION('',(0.,0.,1.));
#27979=DIRECTION('center_axis',(0.,0.,-1.));
#27980=DIRECTION('ref_axis',(1.,0.,0.));
#27981=DIRECTION('center_axis',(0.,0.,1.));
#27982=DIRECTION('ref_axis',(1.,0.,0.));
#27983=DIRECTION('center_axis',(0.,0.,1.));
#27984=DIRECTION('ref_axis',(1.,0.,0.));
#27985=DIRECTION('center_axis',(0.,0.,1.));
#27986=DIRECTION('ref_axis',(1.,0.,0.));
#27987=DIRECTION('',(0.,0.,1.));
#27988=DIRECTION('center_axis',(0.,0.,-1.));
#27989=DIRECTION('ref_axis',(1.,0.,0.));
#27990=DIRECTION('center_axis',(0.,0.,1.));
#27991=DIRECTION('ref_axis',(1.,0.,0.));
#27992=DIRECTION('center_axis',(1.,0.,0.));
#27993=DIRECTION('ref_axis',(0.,0.,-1.));
#27994=DIRECTION('center_axis',(1.,0.,0.));
#27995=DIRECTION('ref_axis',(0.,0.,-1.));
#27996=DIRECTION('',(1.,0.,0.));
#27997=DIRECTION('center_axis',(-1.,0.,0.));
#27998=DIRECTION('ref_axis',(0.,0.,-1.));
#27999=DIRECTION('center_axis',(1.,0.,0.));
#28000=DIRECTION('ref_axis',(0.,0.,-1.));
#28001=DIRECTION('center_axis',(1.,0.,0.));
#28002=DIRECTION('ref_axis',(0.,0.,-1.));
#28003=DIRECTION('center_axis',(1.,0.,0.));
#28004=DIRECTION('ref_axis',(0.,0.,-1.));
#28005=DIRECTION('',(1.,0.,0.));
#28006=DIRECTION('center_axis',(-1.,0.,0.));
#28007=DIRECTION('ref_axis',(0.,0.,-1.));
#28008=DIRECTION('center_axis',(1.,0.,0.));
#28009=DIRECTION('ref_axis',(0.,0.,-1.));
#28010=DIRECTION('center_axis',(1.,0.,0.));
#28011=DIRECTION('ref_axis',(0.,0.,-1.));
#28012=DIRECTION('center_axis',(1.,0.,0.));
#28013=DIRECTION('ref_axis',(0.,0.,-1.));
#28014=DIRECTION('',(1.,0.,0.));
#28015=DIRECTION('center_axis',(-1.,0.,0.));
#28016=DIRECTION('ref_axis',(0.,0.,-1.));
#28017=DIRECTION('center_axis',(1.,0.,0.));
#28018=DIRECTION('ref_axis',(0.,0.,-1.));
#28019=DIRECTION('center_axis',(1.,0.,0.));
#28020=DIRECTION('ref_axis',(0.,0.,-1.));
#28021=DIRECTION('center_axis',(1.,0.,0.));
#28022=DIRECTION('ref_axis',(0.,0.,-1.));
#28023=DIRECTION('',(1.,0.,0.));
#28024=DIRECTION('center_axis',(-1.,0.,0.));
#28025=DIRECTION('ref_axis',(0.,0.,-1.));
#28026=DIRECTION('center_axis',(0.,1.,0.));
#28027=DIRECTION('ref_axis',(-1.,0.,0.));
#28028=DIRECTION('',(-1.,0.,0.));
#28029=DIRECTION('',(0.,0.,1.));
#28030=DIRECTION('',(-1.,0.,0.));
#28031=DIRECTION('',(0.,0.,1.));
#28032=DIRECTION('center_axis',(1.,0.,0.));
#28033=DIRECTION('ref_axis',(0.,1.,0.));
#28034=DIRECTION('',(0.,1.,0.));
#28035=DIRECTION('',(0.,1.,0.));
#28036=DIRECTION('',(0.,0.,1.));
#28037=DIRECTION('center_axis',(0.,-1.,0.));
#28038=DIRECTION('ref_axis',(1.,0.,0.));
#28039=DIRECTION('',(1.,0.,0.));
#28040=DIRECTION('',(1.,0.,0.));
#28041=DIRECTION('',(0.,0.,1.));
#28042=DIRECTION('center_axis',(-1.,0.,0.));
#28043=DIRECTION('ref_axis',(0.,-1.,0.));
#28044=DIRECTION('',(0.,-1.,0.));
#28045=DIRECTION('',(0.,-1.,0.));
#28046=DIRECTION('center_axis',(0.,0.,1.));
#28047=DIRECTION('ref_axis',(1.,0.,0.));
#28048=DIRECTION('center_axis',(0.,0.,1.));
#28049=DIRECTION('ref_axis',(1.,0.,0.));
#28050=DIRECTION('axis',(0.,0.,1.));
#28051=DIRECTION('refdir',(1.,0.,0.));
#28052=DIRECTION('axis',(0.,0.,1.));
#28053=DIRECTION('refdir',(1.,0.,0.));
#28054=DIRECTION('center_axis',(0.,0.,1.));
#28055=DIRECTION('ref_axis',(1.,0.,0.));
#28056=DIRECTION('',(-1.,0.,0.));
#28057=DIRECTION('center_axis',(0.,0.,1.));
#28058=DIRECTION('ref_axis',(1.,0.,0.));
#28059=DIRECTION('center_axis',(0.,0.,1.));
#28060=DIRECTION('ref_axis',(1.,0.,0.));
#28061=DIRECTION('',(0.,0.,-1.));
#28062=DIRECTION('center_axis',(0.,0.,1.));
#28063=DIRECTION('ref_axis',(1.,0.,0.));
#28064=DIRECTION('',(0.,0.,1.));
#28065=DIRECTION('center_axis',(0.,0.,-1.));
#28066=DIRECTION('ref_axis',(1.,0.,0.));
#28067=DIRECTION('center_axis',(0.,0.,1.));
#28068=DIRECTION('ref_axis',(1.,0.,0.));
#28069=DIRECTION('',(0.,0.,1.));
#28070=DIRECTION('center_axis',(0.,0.,1.));
#28071=DIRECTION('ref_axis',(1.,0.,0.));
#28072=DIRECTION('',(1.,0.,0.));
#28073=DIRECTION('center_axis',(0.,0.,1.));
#28074=DIRECTION('ref_axis',(1.,0.,0.));
#28075=DIRECTION('center_axis',(0.,0.,1.));
#28076=DIRECTION('ref_axis',(1.,0.,0.));
#28077=DIRECTION('',(0.,0.,-1.));
#28078=DIRECTION('center_axis',(0.,0.,1.));
#28079=DIRECTION('ref_axis',(1.,0.,0.));
#28080=DIRECTION('',(0.,0.,1.));
#28081=DIRECTION('center_axis',(0.,0.,-1.));
#28082=DIRECTION('ref_axis',(1.,0.,0.));
#28083=DIRECTION('center_axis',(0.,0.,1.));
#28084=DIRECTION('ref_axis',(1.,0.,0.));
#28085=DIRECTION('',(0.,0.,1.));
#28086=DIRECTION('center_axis',(0.,0.,1.));
#28087=DIRECTION('ref_axis',(1.,0.,0.));
#28088=DIRECTION('',(-1.,0.,0.));
#28089=DIRECTION('center_axis',(0.,0.,1.));
#28090=DIRECTION('ref_axis',(1.,0.,0.));
#28091=DIRECTION('center_axis',(0.,0.,1.));
#28092=DIRECTION('ref_axis',(1.,0.,0.));
#28093=DIRECTION('',(0.,0.,-1.));
#28094=DIRECTION('center_axis',(0.,0.,1.));
#28095=DIRECTION('ref_axis',(1.,0.,0.));
#28096=DIRECTION('',(0.,0.,1.));
#28097=DIRECTION('center_axis',(0.,0.,-1.));
#28098=DIRECTION('ref_axis',(1.,0.,0.));
#28099=DIRECTION('center_axis',(0.,0.,1.));
#28100=DIRECTION('ref_axis',(1.,0.,0.));
#28101=DIRECTION('',(0.,0.,1.));
#28102=DIRECTION('center_axis',(0.,0.,1.));
#28103=DIRECTION('ref_axis',(1.,0.,0.));
#28104=DIRECTION('',(1.,0.,0.));
#28105=DIRECTION('center_axis',(0.,0.,1.));
#28106=DIRECTION('ref_axis',(1.,0.,0.));
#28107=DIRECTION('center_axis',(0.,0.,1.));
#28108=DIRECTION('ref_axis',(1.,0.,0.));
#28109=DIRECTION('',(0.,0.,-1.));
#28110=DIRECTION('center_axis',(0.,0.,1.));
#28111=DIRECTION('ref_axis',(1.,0.,0.));
#28112=DIRECTION('',(0.,0.,1.));
#28113=DIRECTION('center_axis',(0.,0.,-1.));
#28114=DIRECTION('ref_axis',(1.,0.,0.));
#28115=DIRECTION('center_axis',(0.,0.,1.));
#28116=DIRECTION('ref_axis',(1.,0.,0.));
#28117=DIRECTION('',(0.,0.,1.));
#28118=DIRECTION('center_axis',(0.,-1.,0.));
#28119=DIRECTION('ref_axis',(0.,0.,-1.));
#28120=DIRECTION('',(-1.,0.,0.));
#28121=DIRECTION('',(-1.,0.,0.));
#28122=DIRECTION('',(0.,0.,1.));
#28123=DIRECTION('',(1.,0.,0.));
#28124=DIRECTION('',(0.,0.,-1.));
#28125=DIRECTION('',(-1.,0.,0.));
#28126=DIRECTION('center_axis',(0.,1.,0.));
#28127=DIRECTION('ref_axis',(0.,0.,1.));
#28128=DIRECTION('',(1.,0.,0.));
#28129=DIRECTION('',(1.,0.,0.));
#28130=DIRECTION('',(0.,0.,1.));
#28131=DIRECTION('',(1.,0.,0.));
#28132=DIRECTION('',(0.,0.,-1.));
#28133=DIRECTION('',(1.,0.,0.));
#28134=DIRECTION('center_axis',(-1.,0.,0.));
#28135=DIRECTION('ref_axis',(0.,0.,1.));
#28136=DIRECTION('',(0.,-1.,0.));
#28137=DIRECTION('',(0.,0.,1.));
#28138=DIRECTION('',(0.,1.,0.));
#28139=DIRECTION('',(0.,0.,-1.));
#28140=DIRECTION('',(0.,-1.,0.));
#28141=DIRECTION('',(0.,-1.,0.));
#28142=DIRECTION('',(0.,0.,1.));
#28143=DIRECTION('',(0.,-1.,0.));
#28144=DIRECTION('',(0.,0.,-1.));
#28145=DIRECTION('',(0.,-1.,0.));
#28146=DIRECTION('center_axis',(0.,0.,-1.));
#28147=DIRECTION('ref_axis',(0.,1.,0.));
#28148=DIRECTION('',(0.,1.,0.));
#28149=DIRECTION('',(1.,0.,0.));
#28150=DIRECTION('center_axis',(0.,-1.,0.));
#28151=DIRECTION('ref_axis',(0.,0.,-1.));
#28152=DIRECTION('',(0.,0.,-1.));
#28153=DIRECTION('',(1.,0.,0.));
#28154=DIRECTION('center_axis',(0.,0.,1.));
#28155=DIRECTION('ref_axis',(0.,-1.,0.));
#28156=DIRECTION('',(0.,-1.,0.));
#28157=DIRECTION('',(1.,0.,0.));
#28158=DIRECTION('center_axis',(0.,1.,0.));
#28159=DIRECTION('ref_axis',(0.,0.,1.));
#28160=DIRECTION('',(0.,0.,1.));
#28161=DIRECTION('',(1.,0.,0.));
#28162=DIRECTION('center_axis',(0.,0.,-1.));
#28163=DIRECTION('ref_axis',(0.,1.,0.));
#28164=DIRECTION('',(0.,1.,0.));
#28165=DIRECTION('center_axis',(0.,0.,-1.));
#28166=DIRECTION('ref_axis',(0.,1.,0.));
#28167=DIRECTION('',(0.,1.,0.));
#28168=DIRECTION('',(1.,0.,0.));
#28169=DIRECTION('center_axis',(0.,-1.,0.));
#28170=DIRECTION('ref_axis',(0.,0.,-1.));
#28171=DIRECTION('',(0.,0.,-1.));
#28172=DIRECTION('',(1.,0.,0.));
#28173=DIRECTION('center_axis',(0.,0.,-1.));
#28174=DIRECTION('ref_axis',(0.,1.,0.));
#28175=DIRECTION('',(0.,1.,0.));
#28176=DIRECTION('',(1.,0.,0.));
#28177=DIRECTION('center_axis',(0.,1.,0.));
#28178=DIRECTION('ref_axis',(0.,0.,1.));
#28179=DIRECTION('',(0.,0.,1.));
#28180=DIRECTION('',(1.,0.,0.));
#28181=DIRECTION('center_axis',(0.,0.,-1.));
#28182=DIRECTION('ref_axis',(0.,1.,0.));
#28183=DIRECTION('',(0.,1.,0.));
#28184=DIRECTION('center_axis',(1.,0.,0.));
#28185=DIRECTION('ref_axis',(0.,0.,-1.));
#28186=DIRECTION('axis',(0.,0.,1.));
#28187=DIRECTION('refdir',(1.,0.,0.));
#28188=DIRECTION('center_axis',(0.,0.,1.));
#28189=DIRECTION('ref_axis',(0.,-1.,0.));
#28190=DIRECTION('',(0.,-1.,0.));
#28191=DIRECTION('',(1.,0.,0.));
#28192=DIRECTION('',(0.,-1.,0.));
#28193=DIRECTION('',(1.,0.,0.));
#28194=DIRECTION('center_axis',(0.,1.,0.));
#28195=DIRECTION('ref_axis',(0.,0.,1.));
#28196=DIRECTION('',(0.,0.,1.));
#28197=DIRECTION('',(0.,0.,1.));
#28198=DIRECTION('',(1.,0.,0.));
#28199=DIRECTION('center_axis',(0.,0.,-1.));
#28200=DIRECTION('ref_axis',(0.,1.,0.));
#28201=DIRECTION('',(0.,1.,0.));
#28202=DIRECTION('',(0.,1.,0.));
#28203=DIRECTION('',(1.,0.,0.));
#28204=DIRECTION('center_axis',(0.,-1.,0.));
#28205=DIRECTION('ref_axis',(0.,0.,-1.));
#28206=DIRECTION('',(0.,0.,-1.));
#28207=DIRECTION('',(0.,0.,-1.));
#28208=DIRECTION('',(1.,0.,0.));
#28209=DIRECTION('center_axis',(0.,0.,-1.));
#28210=DIRECTION('ref_axis',(0.,1.,0.));
#28211=DIRECTION('',(0.,1.,0.));
#28212=DIRECTION('',(0.,1.,0.));
#28213=DIRECTION('',(1.,0.,0.));
#28214=DIRECTION('center_axis',(0.,1.,0.));
#28215=DIRECTION('ref_axis',(0.,0.,1.));
#28216=DIRECTION('',(0.,0.,1.));
#28217=DIRECTION('',(0.,0.,1.));
#28218=DIRECTION('',(1.,0.,0.));
#28219=DIRECTION('center_axis',(0.,0.,-1.));
#28220=DIRECTION('ref_axis',(0.,1.,0.));
#28221=DIRECTION('',(0.,1.,0.));
#28222=DIRECTION('',(0.,1.,0.));
#28223=DIRECTION('',(1.,0.,0.));
#28224=DIRECTION('center_axis',(0.,-1.,0.));
#28225=DIRECTION('ref_axis',(0.,0.,-1.));
#28226=DIRECTION('',(0.,0.,-1.));
#28227=DIRECTION('',(0.,0.,-1.));
#28228=DIRECTION('center_axis',(1.,0.,0.));
#28229=DIRECTION('ref_axis',(0.,0.,-1.));
#28230=DIRECTION('center_axis',(1.,0.,0.));
#28231=DIRECTION('ref_axis',(0.,0.,-1.));
#28232=DIRECTION('axis',(0.,0.,1.));
#28233=DIRECTION('refdir',(1.,0.,0.));
#28234=DIRECTION('center_axis',(0.,0.,-1.));
#28235=DIRECTION('ref_axis',(0.,-1.,0.));
#28236=DIRECTION('',(0.,1.,0.));
#28237=DIRECTION('',(-1.,0.,0.));
#28238=DIRECTION('',(0.,-1.,0.));
#28239=DIRECTION('',(-1.,0.,0.));
#28240=DIRECTION('center_axis',(0.,1.,0.));
#28241=DIRECTION('ref_axis',(0.,0.,-1.));
#28242=DIRECTION('',(0.,0.,1.));
#28243=DIRECTION('',(0.,0.,-1.));
#28244=DIRECTION('',(-1.,0.,0.));
#28245=DIRECTION('center_axis',(0.,0.,-1.));
#28246=DIRECTION('ref_axis',(0.,-1.,0.));
#28247=DIRECTION('',(0.,1.,0.));
#28248=DIRECTION('',(0.,-1.,0.));
#28249=DIRECTION('',(-1.,0.,0.));
#28250=DIRECTION('center_axis',(0.,-1.,0.));
#28251=DIRECTION('ref_axis',(0.,0.,1.));
#28252=DIRECTION('',(0.,0.,-1.));
#28253=DIRECTION('',(0.,0.,1.));
#28254=DIRECTION('',(-1.,0.,0.));
#28255=DIRECTION('center_axis',(0.,0.,-1.));
#28256=DIRECTION('ref_axis',(0.,-1.,0.));
#28257=DIRECTION('',(0.,1.,0.));
#28258=DIRECTION('',(0.,-1.,0.));
#28259=DIRECTION('',(-1.,0.,0.));
#28260=DIRECTION('center_axis',(0.,1.,0.));
#28261=DIRECTION('ref_axis',(0.,0.,-1.));
#28262=DIRECTION('',(0.,0.,1.));
#28263=DIRECTION('',(0.,0.,-1.));
#28264=DIRECTION('',(-1.,0.,0.));
#28265=DIRECTION('center_axis',(0.,0.,1.));
#28266=DIRECTION('ref_axis',(0.,1.,0.));
#28267=DIRECTION('',(0.,-1.,0.));
#28268=DIRECTION('',(0.,1.,0.));
#28269=DIRECTION('',(-1.,0.,0.));
#28270=DIRECTION('center_axis',(0.,-1.,0.));
#28271=DIRECTION('ref_axis',(0.,0.,1.));
#28272=DIRECTION('',(0.,0.,-1.));
#28273=DIRECTION('',(0.,0.,1.));
#28274=DIRECTION('center_axis',(1.,0.,0.));
#28275=DIRECTION('ref_axis',(0.,0.,-1.));
#28276=DIRECTION('center_axis',(-1.,0.,0.));
#28277=DIRECTION('ref_axis',(0.,0.,1.));
#28278=DIRECTION('',(0.,0.,1.));
#28279=DIRECTION('',(1.,0.,0.));
#28280=DIRECTION('',(0.,0.,1.));
#28281=DIRECTION('',(1.,0.,0.));
#28282=DIRECTION('',(0.,0.,1.));
#28283=DIRECTION('',(1.,0.,0.));
#28284=DIRECTION('axis',(0.,0.,1.));
#28285=DIRECTION('refdir',(1.,0.,0.));
#28286=DIRECTION('center_axis',(0.,1.,0.));
#28287=DIRECTION('ref_axis',(1.,0.,0.));
#28288=DIRECTION('center_axis',(0.,1.,0.));
#28289=DIRECTION('ref_axis',(1.,0.,0.));
#28290=DIRECTION('',(0.707106781186548,-0.707106781186547,-8.65956056235494E-17));
#28291=DIRECTION('center_axis',(0.,-1.,0.));
#28292=DIRECTION('ref_axis',(1.,0.,0.));
#28293=DIRECTION('center_axis',(0.,1.,0.));
#28294=DIRECTION('ref_axis',(1.,0.,0.));
#28295=DIRECTION('',(0.,-1.,0.));
#28296=DIRECTION('center_axis',(0.,-1.,0.));
#28297=DIRECTION('ref_axis',(1.,0.,0.));
#28298=DIRECTION('center_axis',(0.,1.,0.));
#28299=DIRECTION('ref_axis',(1.,0.,0.));
#28300=DIRECTION('center_axis',(0.,1.,0.));
#28301=DIRECTION('ref_axis',(1.,0.,0.));
#28302=DIRECTION('center_axis',(0.,1.,0.));
#28303=DIRECTION('ref_axis',(1.,0.,0.));
#28304=DIRECTION('',(0.,-1.,0.));
#28305=DIRECTION('center_axis',(0.,1.,0.));
#28306=DIRECTION('ref_axis',(1.,0.,0.));
#28307=DIRECTION('center_axis',(0.,1.,0.));
#28308=DIRECTION('ref_axis',(1.,0.,0.));
#28309=DIRECTION('axis',(0.,0.,1.));
#28310=DIRECTION('refdir',(1.,0.,0.));
#28311=DIRECTION('center_axis',(0.866025403784439,0.,-0.5));
#28312=DIRECTION('ref_axis',(0.5,0.,0.866025403784439));
#28313=DIRECTION('',(-0.5,0.,-0.866025403784439));
#28314=DIRECTION('',(0.,-1.,0.));
#28315=DIRECTION('',(0.5,0.,0.866025403784439));
#28316=DIRECTION('',(0.,-1.,0.));
#28317=DIRECTION('center_axis',(1.20185167898973E-16,0.,-1.));
#28318=DIRECTION('ref_axis',(1.,0.,1.20185167898973E-16));
#28319=DIRECTION('',(-1.,0.,-1.20185167898973E-16));
#28320=DIRECTION('',(0.,-1.,0.));
#28321=DIRECTION('',(1.,0.,1.20185167898973E-16));
#28322=DIRECTION('center_axis',(-0.866025403784439,0.,-0.5));
#28323=DIRECTION('ref_axis',(0.5,0.,-0.866025403784439));
#28324=DIRECTION('',(-0.5,0.,0.866025403784439));
#28325=DIRECTION('',(0.,-1.,0.));
#28326=DIRECTION('',(0.5,0.,-0.866025403784439));
#28327=DIRECTION('center_axis',(-0.866025403784439,0.,0.5));
#28328=DIRECTION('ref_axis',(-0.5,0.,-0.866025403784439));
#28329=DIRECTION('',(0.5,0.,0.866025403784439));
#28330=DIRECTION('',(0.,-1.,0.));
#28331=DIRECTION('',(-0.5,0.,-0.866025403784439));
#28332=DIRECTION('center_axis',(-2.40370335797945E-16,0.,1.));
#28333=DIRECTION('ref_axis',(-1.,0.,-2.40370335797945E-16));
#28334=DIRECTION('',(1.,0.,2.40370335797945E-16));
#28335=DIRECTION('',(0.,-1.,0.));
#28336=DIRECTION('',(-1.,0.,-2.40370335797945E-16));
#28337=DIRECTION('center_axis',(0.866025403784439,0.,0.5));
#28338=DIRECTION('ref_axis',(-0.5,0.,0.866025403784439));
#28339=DIRECTION('',(0.5,0.,-0.866025403784439));
#28340=DIRECTION('',(-0.5,0.,0.866025403784439));
#28341=DIRECTION('center_axis',(0.,1.,0.));
#28342=DIRECTION('ref_axis',(1.,0.,0.));
#28343=DIRECTION('center_axis',(0.,-1.,0.));
#28344=DIRECTION('ref_axis',(0.,0.,-1.));
#28345=DIRECTION('center_axis',(0.,1.,0.));
#28346=DIRECTION('ref_axis',(1.,0.,0.));
#28347=DIRECTION('center_axis',(0.,1.,0.));
#28348=DIRECTION('ref_axis',(1.,0.,0.));
#28349=DIRECTION('center_axis',(0.,1.,0.));
#28350=DIRECTION('ref_axis',(1.,0.,0.));
#28351=DIRECTION('center_axis',(0.,1.,0.));
#28352=DIRECTION('ref_axis',(1.,0.,0.));
#28353=DIRECTION('',(0.,-1.,0.));
#28354=DIRECTION('center_axis',(0.,1.,0.));
#28355=DIRECTION('ref_axis',(1.,0.,0.));
#28356=DIRECTION('center_axis',(0.,1.,0.));
#28357=DIRECTION('ref_axis',(1.,0.,0.));
#28358=DIRECTION('center_axis',(0.,1.,0.));
#28359=DIRECTION('ref_axis',(0.,0.,1.));
#28360=DIRECTION('center_axis',(0.,-1.,0.));
#28361=DIRECTION('ref_axis',(1.,0.,0.));
#28362=DIRECTION('center_axis',(0.,-1.,0.));
#28363=DIRECTION('ref_axis',(1.,0.,0.));
#28364=DIRECTION('center_axis',(0.,-1.,0.));
#28365=DIRECTION('ref_axis',(1.,0.,0.));
#28366=DIRECTION('',(0.707106781186548,0.707106781186547,8.65956056235493E-17));
#28367=DIRECTION('center_axis',(0.,-1.,0.));
#28368=DIRECTION('ref_axis',(1.,0.,0.));
#28369=DIRECTION('center_axis',(0.,-1.,0.));
#28370=DIRECTION('ref_axis',(1.,0.,0.));
#28371=DIRECTION('',(0.,1.,0.));
#28372=DIRECTION('center_axis',(0.,1.,0.));
#28373=DIRECTION('ref_axis',(1.,0.,0.));
#28374=DIRECTION('center_axis',(0.,-1.,0.));
#28375=DIRECTION('ref_axis',(1.,0.,0.));
#28376=DIRECTION('',(-0.707106781186547,0.707106781186548,-8.65956056235493E-17));
#28377=DIRECTION('center_axis',(0.,-1.,0.));
#28378=DIRECTION('ref_axis',(0.,0.,-1.));
#28379=DIRECTION('center_axis',(0.,-1.,0.));
#28380=DIRECTION('ref_axis',(1.,0.,0.));
#28381=DIRECTION('center_axis',(0.,1.,0.));
#28382=DIRECTION('ref_axis',(1.,0.,0.));
#28383=DIRECTION('center_axis',(0.,1.,0.));
#28384=DIRECTION('ref_axis',(1.,0.,0.));
#28385=DIRECTION('',(-0.447213595499958,0.894427190999916,-5.47678698264203E-17));
#28386=DIRECTION('center_axis',(0.,-1.,0.));
#28387=DIRECTION('ref_axis',(1.,0.,0.));
#28388=DIRECTION('',(0.,1.,0.));
#28389=DIRECTION('axis',(0.,0.,1.));
#28390=DIRECTION('refdir',(1.,0.,0.));
#28391=DIRECTION('center_axis',(1.,0.,0.));
#28392=DIRECTION('ref_axis',(0.,0.207879895528894,-0.978154358490978));
#28393=DIRECTION('',(-1.,0.,0.));
#28394=DIRECTION('center_axis',(1.,0.,0.));
#28395=DIRECTION('ref_axis',(0.,0.,-1.));
#28396=DIRECTION('center_axis',(1.,0.,0.));
#28397=DIRECTION('ref_axis',(0.,0.,-1.));
#28398=DIRECTION('',(-1.,0.,0.));
#28399=DIRECTION('center_axis',(1.,0.,0.));
#28400=DIRECTION('ref_axis',(0.,0.,-1.));
#28401=DIRECTION('',(-1.,0.,0.));
#28402=DIRECTION('center_axis',(1.,0.,0.));
#28403=DIRECTION('ref_axis',(0.,0.,-1.));
#28404=DIRECTION('',(-1.,0.,0.));
#28405=DIRECTION('center_axis',(1.,0.,0.));
#28406=DIRECTION('ref_axis',(0.,0.,-1.));
#28407=DIRECTION('',(-1.,0.,0.));
#28408=DIRECTION('center_axis',(1.,0.,0.));
#28409=DIRECTION('ref_axis',(0.,0.,-1.));
#28410=DIRECTION('',(-1.,0.,0.));
#28411=DIRECTION('center_axis',(1.,0.,0.));
#28412=DIRECTION('ref_axis',(0.,0.,-1.));
#28413=DIRECTION('',(-1.,0.,0.));
#28414=DIRECTION('center_axis',(1.,0.,0.));
#28415=DIRECTION('ref_axis',(0.,0.,-1.));
#28416=DIRECTION('',(-1.,0.,0.));
#28417=DIRECTION('center_axis',(1.,0.,0.));
#28418=DIRECTION('ref_axis',(0.,0.,-1.));
#28419=DIRECTION('',(-1.,0.,0.));
#28420=DIRECTION('center_axis',(1.,0.,0.));
#28421=DIRECTION('ref_axis',(0.,0.,-1.));
#28422=DIRECTION('center_axis',(1.,0.,0.));
#28423=DIRECTION('ref_axis',(0.,2.68771689099506E-14,-1.));
#28424=DIRECTION('',(1.,3.30650148539799E-30,-1.22464679914735E-16));
#28425=DIRECTION('center_axis',(-1.,0.,0.));
#28426=DIRECTION('ref_axis',(0.,2.68771689099506E-14,-1.));
#28427=DIRECTION('center_axis',(1.,0.,0.));
#28428=DIRECTION('ref_axis',(0.,2.68771689099506E-14,-1.));
#28429=DIRECTION('',(1.,3.30650148539799E-30,-1.22464679914735E-16));
#28430=DIRECTION('center_axis',(1.,0.,0.));
#28431=DIRECTION('ref_axis',(0.,2.68771689099506E-14,-1.));
#28432=DIRECTION('',(1.,3.30650148539799E-30,-1.22464679914735E-16));
#28433=DIRECTION('center_axis',(1.,0.,0.));
#28434=DIRECTION('ref_axis',(0.,2.68771689099506E-14,-1.));
#28435=DIRECTION('',(1.,3.30650148539799E-30,-1.22464679914735E-16));
#28436=DIRECTION('center_axis',(1.,0.,0.));
#28437=DIRECTION('ref_axis',(0.,2.68771689099506E-14,-1.));
#28438=DIRECTION('',(1.,3.30650148539799E-30,-1.22464679914735E-16));
#28439=DIRECTION('center_axis',(1.,0.,0.));
#28440=DIRECTION('ref_axis',(0.,2.68771689099506E-14,-1.));
#28441=DIRECTION('',(1.,3.30650148539799E-30,-1.22464679914735E-16));
#28442=DIRECTION('center_axis',(1.,0.,0.));
#28443=DIRECTION('ref_axis',(0.,2.68771689099506E-14,-1.));
#28444=DIRECTION('',(1.,3.30650148539799E-30,-1.22464679914735E-16));
#28445=DIRECTION('center_axis',(1.,0.,0.));
#28446=DIRECTION('ref_axis',(0.,2.68771689099506E-14,-1.));
#28447=DIRECTION('',(1.,3.30650148539799E-30,-1.22464679914735E-16));
#28448=DIRECTION('center_axis',(1.,0.,0.));
#28449=DIRECTION('ref_axis',(0.,2.68771689099506E-14,-1.));
#28450=DIRECTION('',(1.,3.30650148539799E-30,-1.22464679914735E-16));
#28451=DIRECTION('center_axis',(1.,0.,0.));
#28452=DIRECTION('ref_axis',(0.,2.68771689099506E-14,-1.));
#28453=DIRECTION('center_axis',(1.,0.,0.));
#28454=DIRECTION('ref_axis',(0.,2.68771689099506E-14,-1.));
#28455=DIRECTION('center_axis',(1.,0.,0.));
#28456=DIRECTION('ref_axis',(0.,0.,-1.));
#28457=DIRECTION('',(0.,1.,0.));
#28458=DIRECTION('center_axis',(1.,0.,0.));
#28459=DIRECTION('ref_axis',(0.,0.,-1.));
#28460=DIRECTION('center_axis',(1.,0.,0.));
#28461=DIRECTION('ref_axis',(0.,0.,-1.));
#28462=DIRECTION('center_axis',(-1.,0.,0.));
#28463=DIRECTION('ref_axis',(0.,0.,-1.));
#28464=DIRECTION('center_axis',(-1.,0.,0.));
#28465=DIRECTION('ref_axis',(0.,0.,-1.));
#28466=DIRECTION('center_axis',(-1.,0.,0.));
#28467=DIRECTION('ref_axis',(0.,0.,-1.));
#28468=DIRECTION('center_axis',(1.,0.,0.));
#28469=DIRECTION('ref_axis',(0.,0.,-1.));
#28470=DIRECTION('center_axis',(1.,0.,0.));
#28471=DIRECTION('ref_axis',(0.,0.,-1.));
#28472=DIRECTION('',(1.,0.,0.));
#28473=DIRECTION('center_axis',(1.,0.,0.));
#28474=DIRECTION('ref_axis',(0.,0.,-1.));
#28475=DIRECTION('center_axis',(1.,0.,0.));
#28476=DIRECTION('ref_axis',(0.,0.,-1.));
#28477=DIRECTION('',(1.,0.,0.));
#28478=DIRECTION('center_axis',(1.,0.,0.));
#28479=DIRECTION('ref_axis',(0.,0.,-1.));
#28480=DIRECTION('center_axis',(1.,0.,0.));
#28481=DIRECTION('ref_axis',(0.,0.,-1.));
#28482=DIRECTION('',(1.,0.,0.));
#28483=DIRECTION('center_axis',(0.,0.,1.));
#28484=DIRECTION('ref_axis',(0.,-1.,0.));
#28485=DIRECTION('',(0.,-1.,0.));
#28486=DIRECTION('',(-1.,0.,0.));
#28487=DIRECTION('',(1.,0.,0.));
#28488=DIRECTION('center_axis',(1.,0.,0.));
#28489=DIRECTION('ref_axis',(0.,0.,-1.));
#28490=DIRECTION('center_axis',(1.,0.,0.));
#28491=DIRECTION('ref_axis',(0.,0.,-1.));
#28492=DIRECTION('center_axis',(1.,0.,0.));
#28493=DIRECTION('ref_axis',(0.,0.,-1.));
#28494=DIRECTION('center_axis',(1.,0.,0.));
#28495=DIRECTION('ref_axis',(0.,-1.22464679914735E-16,1.));
#28496=DIRECTION('center_axis',(1.,0.,0.));
#28497=DIRECTION('ref_axis',(0.,0.,-1.));
#28498=DIRECTION('center_axis',(1.,0.,0.));
#28499=DIRECTION('ref_axis',(0.,0.,-1.));
#28500=DIRECTION('',(-1.,0.,0.));
#28501=DIRECTION('center_axis',(1.,0.,0.));
#28502=DIRECTION('ref_axis',(0.,0.,-1.));
#28503=DIRECTION('center_axis',(1.,0.,0.));
#28504=DIRECTION('ref_axis',(0.,0.,-1.));
#28505=DIRECTION('axis',(0.,0.,1.));
#28506=DIRECTION('refdir',(1.,0.,0.));
#28507=DIRECTION('center_axis',(0.,1.,0.));
#28508=DIRECTION('ref_axis',(0.,0.,1.));
#28509=DIRECTION('center_axis',(0.,-1.,0.));
#28510=DIRECTION('ref_axis',(1.,0.,0.));
#28511=DIRECTION('center_axis',(0.,-1.,0.));
#28512=DIRECTION('ref_axis',(1.,0.,0.));
#28513=DIRECTION('center_axis',(0.,-1.,0.));
#28514=DIRECTION('ref_axis',(1.,0.,0.));
#28515=DIRECTION('',(0.707106781186547,0.707106781186548,8.65956056235493E-17));
#28516=DIRECTION('center_axis',(0.,-1.,0.));
#28517=DIRECTION('ref_axis',(1.,0.,0.));
#28518=DIRECTION('center_axis',(0.,-1.,0.));
#28519=DIRECTION('ref_axis',(1.,0.,0.));
#28520=DIRECTION('',(0.,1.,0.));
#28521=DIRECTION('center_axis',(0.,1.,0.));
#28522=DIRECTION('ref_axis',(1.,0.,0.));
#28523=DIRECTION('center_axis',(0.,-1.,0.));
#28524=DIRECTION('ref_axis',(1.,0.,0.));
#28525=DIRECTION('',(-0.707106781186547,0.707106781186548,-8.65956056235493E-17));
#28526=DIRECTION('center_axis',(0.,-1.,0.));
#28527=DIRECTION('ref_axis',(0.,0.,-1.));
#28528=DIRECTION('center_axis',(0.,-1.,0.));
#28529=DIRECTION('ref_axis',(1.,0.,0.));
#28530=DIRECTION('center_axis',(0.,1.,0.));
#28531=DIRECTION('ref_axis',(1.,0.,0.));
#28532=DIRECTION('center_axis',(0.,1.,0.));
#28533=DIRECTION('ref_axis',(1.,0.,0.));
#28534=DIRECTION('',(-0.447213595499958,0.894427190999916,-5.47678698264203E-17));
#28535=DIRECTION('center_axis',(0.,-1.,0.));
#28536=DIRECTION('ref_axis',(1.,0.,0.));
#28537=DIRECTION('center_axis',(0.,1.,0.));
#28538=DIRECTION('ref_axis',(1.,0.,0.));
#28539=DIRECTION('',(0.,1.,0.));
#28540=DIRECTION('center_axis',(0.,1.,0.));
#28541=DIRECTION('ref_axis',(1.,0.,0.));
#28542=DIRECTION('center_axis',(0.,-1.,0.));
#28543=DIRECTION('ref_axis',(1.,0.,0.));
#28544=DIRECTION('',(-0.707106781186547,0.707106781186548,-8.65956056235493E-17));
#28545=DIRECTION('center_axis',(0.,-1.,0.));
#28546=DIRECTION('ref_axis',(0.,0.,-1.));
#28547=DIRECTION('center_axis',(0.866025403784439,0.,-0.5));
#28548=DIRECTION('ref_axis',(0.5,0.,0.866025403784439));
#28549=DIRECTION('',(-0.5,0.,-0.866025403784439));
#28550=DIRECTION('',(0.,-1.,0.));
#28551=DIRECTION('',(0.5,0.,0.866025403784439));
#28552=DIRECTION('',(0.,-1.,0.));
#28553=DIRECTION('center_axis',(1.60246890531964E-16,0.,-1.));
#28554=DIRECTION('ref_axis',(1.,0.,1.60246890531964E-16));
#28555=DIRECTION('',(-1.,0.,-1.60246890531964E-16));
#28556=DIRECTION('',(0.,-1.,0.));
#28557=DIRECTION('',(1.,0.,1.60246890531964E-16));
#28558=DIRECTION('center_axis',(-0.866025403784439,0.,-0.5));
#28559=DIRECTION('ref_axis',(0.5,0.,-0.866025403784439));
#28560=DIRECTION('',(-0.5,0.,0.866025403784439));
#28561=DIRECTION('',(0.,-1.,0.));
#28562=DIRECTION('',(0.5,0.,-0.866025403784439));
#28563=DIRECTION('center_axis',(-0.866025403784439,0.,0.5));
#28564=DIRECTION('ref_axis',(-0.5,0.,-0.866025403784439));
#28565=DIRECTION('',(0.5,0.,0.866025403784439));
#28566=DIRECTION('',(0.,-1.,0.));
#28567=DIRECTION('',(-0.5,0.,-0.866025403784439));
#28568=DIRECTION('center_axis',(-1.60246890531964E-16,0.,1.));
#28569=DIRECTION('ref_axis',(-1.,0.,-1.60246890531964E-16));
#28570=DIRECTION('',(1.,0.,1.60246890531964E-16));
#28571=DIRECTION('',(0.,-1.,0.));
#28572=DIRECTION('',(-1.,0.,-1.60246890531964E-16));
#28573=DIRECTION('center_axis',(0.866025403784439,0.,0.5));
#28574=DIRECTION('ref_axis',(-0.5,0.,0.866025403784439));
#28575=DIRECTION('',(0.5,0.,-0.866025403784439));
#28576=DIRECTION('',(-0.5,0.,0.866025403784439));
#28577=DIRECTION('center_axis',(0.,1.,0.));
#28578=DIRECTION('ref_axis',(1.,0.,0.));
#28579=DIRECTION('center_axis',(0.,-1.,0.));
#28580=DIRECTION('ref_axis',(0.,0.,-1.));
#28581=DIRECTION('axis',(0.,0.,1.));
#28582=DIRECTION('refdir',(1.,0.,0.));
#28583=DIRECTION('center_axis',(0.,1.,0.));
#28584=DIRECTION('ref_axis',(0.,0.,1.));
#28585=DIRECTION('center_axis',(0.,-1.,0.));
#28586=DIRECTION('ref_axis',(1.,0.,0.));
#28587=DIRECTION('center_axis',(0.,-1.,0.));
#28588=DIRECTION('ref_axis',(1.,0.,0.));
#28589=DIRECTION('center_axis',(0.,-1.,0.));
#28590=DIRECTION('ref_axis',(1.,0.,0.));
#28591=DIRECTION('',(0.707106781186548,0.707106781186547,8.65956056235493E-17));
#28592=DIRECTION('center_axis',(0.,-1.,0.));
#28593=DIRECTION('ref_axis',(1.,0.,0.));
#28594=DIRECTION('center_axis',(0.,-1.,0.));
#28595=DIRECTION('ref_axis',(1.,0.,0.));
#28596=DIRECTION('',(0.,1.,0.));
#28597=DIRECTION('center_axis',(0.,1.,0.));
#28598=DIRECTION('ref_axis',(1.,0.,0.));
#28599=DIRECTION('center_axis',(0.,-1.,0.));
#28600=DIRECTION('ref_axis',(1.,0.,0.));
#28601=DIRECTION('',(-0.707106781186547,0.707106781186548,-8.65956056235493E-17));
#28602=DIRECTION('center_axis',(0.,-1.,0.));
#28603=DIRECTION('ref_axis',(0.,0.,-1.));
#28604=DIRECTION('center_axis',(0.,-1.,0.));
#28605=DIRECTION('ref_axis',(1.,0.,0.));
#28606=DIRECTION('center_axis',(0.,1.,0.));
#28607=DIRECTION('ref_axis',(1.,0.,0.));
#28608=DIRECTION('center_axis',(0.,1.,0.));
#28609=DIRECTION('ref_axis',(1.,0.,0.));
#28610=DIRECTION('',(-0.447213595499958,0.894427190999916,-5.47678698264203E-17));
#28611=DIRECTION('center_axis',(0.,-1.,0.));
#28612=DIRECTION('ref_axis',(1.,0.,0.));
#28613=DIRECTION('center_axis',(0.,1.,0.));
#28614=DIRECTION('ref_axis',(1.,0.,0.));
#28615=DIRECTION('',(0.,1.,0.));
#28616=DIRECTION('center_axis',(0.,1.,0.));
#28617=DIRECTION('ref_axis',(1.,0.,0.));
#28618=DIRECTION('center_axis',(0.,-1.,0.));
#28619=DIRECTION('ref_axis',(1.,0.,0.));
#28620=DIRECTION('',(-0.707106781186547,0.707106781186548,-8.65956056235493E-17));
#28621=DIRECTION('center_axis',(0.,-1.,0.));
#28622=DIRECTION('ref_axis',(0.,0.,-1.));
#28623=DIRECTION('center_axis',(0.866025403784439,0.,-0.5));
#28624=DIRECTION('ref_axis',(0.5,0.,0.866025403784439));
#28625=DIRECTION('',(-0.5,0.,-0.866025403784439));
#28626=DIRECTION('',(0.,-1.,0.));
#28627=DIRECTION('',(0.5,0.,0.866025403784439));
#28628=DIRECTION('',(0.,-1.,0.));
#28629=DIRECTION('center_axis',(1.20185167898973E-16,0.,-1.));
#28630=DIRECTION('ref_axis',(1.,0.,1.20185167898973E-16));
#28631=DIRECTION('',(-1.,0.,-1.20185167898973E-16));
#28632=DIRECTION('',(0.,-1.,0.));
#28633=DIRECTION('',(1.,0.,1.20185167898973E-16));
#28634=DIRECTION('center_axis',(-0.866025403784439,0.,-0.5));
#28635=DIRECTION('ref_axis',(0.5,0.,-0.866025403784439));
#28636=DIRECTION('',(-0.5,0.,0.866025403784439));
#28637=DIRECTION('',(0.,-1.,0.));
#28638=DIRECTION('',(0.5,0.,-0.866025403784439));
#28639=DIRECTION('center_axis',(-0.866025403784439,0.,0.5));
#28640=DIRECTION('ref_axis',(-0.5,0.,-0.866025403784439));
#28641=DIRECTION('',(0.5,0.,0.866025403784439));
#28642=DIRECTION('',(0.,-1.,0.));
#28643=DIRECTION('',(-0.5,0.,-0.866025403784439));
#28644=DIRECTION('center_axis',(-2.40370335797945E-16,0.,1.));
#28645=DIRECTION('ref_axis',(-1.,0.,-2.40370335797945E-16));
#28646=DIRECTION('',(1.,0.,2.40370335797945E-16));
#28647=DIRECTION('',(0.,-1.,0.));
#28648=DIRECTION('',(-1.,0.,-2.40370335797945E-16));
#28649=DIRECTION('center_axis',(0.866025403784439,0.,0.5));
#28650=DIRECTION('ref_axis',(-0.5,0.,0.866025403784439));
#28651=DIRECTION('',(0.5,0.,-0.866025403784439));
#28652=DIRECTION('',(-0.5,0.,0.866025403784439));
#28653=DIRECTION('center_axis',(0.,1.,0.));
#28654=DIRECTION('ref_axis',(1.,0.,0.));
#28655=DIRECTION('center_axis',(0.,-1.,0.));
#28656=DIRECTION('ref_axis',(0.,0.,-1.));
#28657=DIRECTION('',(0.,0.,1.));
#28658=DIRECTION('',(1.,0.,0.));
#28659=DIRECTION('',(0.,0.,1.));
#28660=DIRECTION('',(1.,0.,0.));
#28661=DIRECTION('',(0.,0.,1.));
#28662=DIRECTION('',(1.,0.,0.));
#28663=DIRECTION('',(0.,0.,1.));
#28664=DIRECTION('',(1.,0.,0.));
#28665=DIRECTION('',(0.,-1.,2.22044604925031E-16));
#28666=DIRECTION('',(1.,0.,0.));
#28667=DIRECTION('',(0.,-1.,2.22044604925031E-16));
#28668=DIRECTION('',(1.,0.,0.));
#28669=DIRECTION('',(0.,-1.,2.22044604925031E-16));
#28670=DIRECTION('',(1.,0.,0.));
#28671=DIRECTION('',(0.,-1.,2.22044604925031E-16));
#28672=DIRECTION('',(1.,0.,0.));
#28673=DIRECTION('',(0.,-1.,2.22044604925031E-16));
#28674=DIRECTION('',(1.,0.,0.));
#28675=DIRECTION('',(0.,-1.,2.22044604925031E-16));
#28676=DIRECTION('',(1.,0.,0.));
#28677=DIRECTION('',(0.,-1.,2.22044604925031E-16));
#28678=DIRECTION('',(1.,0.,0.));
#28679=DIRECTION('',(0.,-1.,2.22044604925031E-16));
#28680=DIRECTION('',(1.,0.,0.));
#28681=DIRECTION('',(0.,0.,1.));
#28682=DIRECTION('',(1.,0.,0.));
#28683=DIRECTION('',(0.,0.,1.));
#28684=DIRECTION('',(2.22044604925031E-16,-1.,0.));
#28685=DIRECTION('',(0.,0.,1.));
#28686=DIRECTION('',(2.22044604925031E-16,-1.,0.));
#28687=DIRECTION('',(0.,0.,1.));
#28688=DIRECTION('',(2.22044604925031E-16,-1.,0.));
#28689=DIRECTION('',(0.,-1.,2.22044604925031E-16));
#28690=DIRECTION('',(1.,0.,0.));
#28691=DIRECTION('',(0.,-1.,2.22044604925031E-16));
#28692=DIRECTION('',(1.,0.,0.));
#28693=DIRECTION('',(0.,-1.,2.22044604925031E-16));
#28694=DIRECTION('',(1.,0.,0.));
#28695=DIRECTION('',(0.,-1.,2.22044604925031E-16));
#28696=DIRECTION('',(1.,0.,0.));
#28697=DIRECTION('axis',(0.,0.,1.));
#28698=DIRECTION('refdir',(1.,0.,0.));
#28699=DIRECTION('axis',(0.,0.,1.));
#28700=DIRECTION('refdir',(1.,0.,0.));
#28701=DIRECTION('center_axis',(1.,0.,0.));
#28702=DIRECTION('ref_axis',(0.,0.975560628713931,0.219730425074181));
#28703=DIRECTION('',(-1.,0.,0.));
#28704=DIRECTION('center_axis',(-1.,0.,0.));
#28705=DIRECTION('ref_axis',(0.,0.,-1.));
#28706=DIRECTION('center_axis',(1.,0.,0.));
#28707=DIRECTION('ref_axis',(0.,0.,-1.));
#28708=DIRECTION('',(-1.,0.,0.));
#28709=DIRECTION('center_axis',(1.,0.,0.));
#28710=DIRECTION('ref_axis',(0.,0.,-1.));
#28711=DIRECTION('',(-1.,0.,0.));
#28712=DIRECTION('center_axis',(1.,0.,0.));
#28713=DIRECTION('ref_axis',(0.,0.,-1.));
#28714=DIRECTION('',(-1.,0.,0.));
#28715=DIRECTION('center_axis',(1.,0.,0.));
#28716=DIRECTION('ref_axis',(0.,0.,-1.));
#28717=DIRECTION('',(-1.,0.,0.));
#28718=DIRECTION('center_axis',(1.,0.,0.));
#28719=DIRECTION('ref_axis',(0.,0.,-1.));
#28720=DIRECTION('',(-1.,0.,0.));
#28721=DIRECTION('center_axis',(1.,0.,0.));
#28722=DIRECTION('ref_axis',(0.,0.,-1.));
#28723=DIRECTION('',(-1.,0.,0.));
#28724=DIRECTION('center_axis',(1.,0.,0.));
#28725=DIRECTION('ref_axis',(0.,0.,-1.));
#28726=DIRECTION('',(-1.,0.,0.));
#28727=DIRECTION('center_axis',(1.,0.,0.));
#28728=DIRECTION('ref_axis',(0.,0.,-1.));
#28729=DIRECTION('',(-1.,0.,0.));
#28730=DIRECTION('center_axis',(1.,0.,0.));
#28731=DIRECTION('ref_axis',(0.,0.,-1.));
#28732=DIRECTION('',(-1.,0.,0.));
#28733=DIRECTION('center_axis',(1.,0.,0.));
#28734=DIRECTION('ref_axis',(0.,0.,-1.));
#28735=DIRECTION('',(-1.,0.,0.));
#28736=DIRECTION('center_axis',(1.,0.,0.));
#28737=DIRECTION('ref_axis',(0.,0.,-1.));
#28738=DIRECTION('',(-1.,0.,0.));
#28739=DIRECTION('center_axis',(1.,0.,0.));
#28740=DIRECTION('ref_axis',(0.,0.,-1.));
#28741=DIRECTION('',(-1.,0.,0.));
#28742=DIRECTION('center_axis',(1.,0.,0.));
#28743=DIRECTION('ref_axis',(0.,0.,-1.));
#28744=DIRECTION('',(-1.,0.,0.));
#28745=DIRECTION('center_axis',(1.,0.,0.));
#28746=DIRECTION('ref_axis',(0.,0.,-1.));
#28747=DIRECTION('',(-1.,0.,0.));
#28748=DIRECTION('center_axis',(1.,0.,0.));
#28749=DIRECTION('ref_axis',(0.,0.,-1.));
#28750=DIRECTION('',(-1.,0.,0.));
#28751=DIRECTION('center_axis',(1.,0.,0.));
#28752=DIRECTION('ref_axis',(0.,0.,-1.));
#28753=DIRECTION('',(-1.,0.,0.));
#28754=DIRECTION('center_axis',(1.,0.,0.));
#28755=DIRECTION('ref_axis',(0.,0.,-1.));
#28756=DIRECTION('',(-1.,0.,0.));
#28757=DIRECTION('center_axis',(1.,0.,0.));
#28758=DIRECTION('ref_axis',(0.,0.,-1.));
#28759=DIRECTION('',(-1.,0.,0.));
#28760=DIRECTION('center_axis',(1.,0.,0.));
#28761=DIRECTION('ref_axis',(0.,0.,-1.));
#28762=DIRECTION('',(-1.,0.,0.));
#28763=DIRECTION('center_axis',(1.,0.,0.));
#28764=DIRECTION('ref_axis',(0.,0.,-1.));
#28765=DIRECTION('',(-1.,0.,0.));
#28766=DIRECTION('center_axis',(1.,0.,0.));
#28767=DIRECTION('ref_axis',(0.,0.,-1.));
#28768=DIRECTION('',(-1.,0.,0.));
#28769=DIRECTION('center_axis',(1.,0.,0.));
#28770=DIRECTION('ref_axis',(0.,0.,-1.));
#28771=DIRECTION('',(-1.,0.,0.));
#28772=DIRECTION('center_axis',(1.,0.,0.));
#28773=DIRECTION('ref_axis',(0.,0.,-1.));
#28774=DIRECTION('',(-1.,0.,0.));
#28775=DIRECTION('center_axis',(1.,0.,0.));
#28776=DIRECTION('ref_axis',(0.,0.,-1.));
#28777=DIRECTION('',(-1.,0.,0.));
#28778=DIRECTION('center_axis',(1.,0.,0.));
#28779=DIRECTION('ref_axis',(0.,0.,-1.));
#28780=DIRECTION('',(-1.,0.,0.));
#28781=DIRECTION('center_axis',(1.,0.,0.));
#28782=DIRECTION('ref_axis',(0.,0.,-1.));
#28783=DIRECTION('',(-1.,0.,0.));
#28784=DIRECTION('center_axis',(1.,0.,0.));
#28785=DIRECTION('ref_axis',(0.,0.,-1.));
#28786=DIRECTION('',(-1.,0.,0.));
#28787=DIRECTION('center_axis',(1.,0.,0.));
#28788=DIRECTION('ref_axis',(0.,0.,-1.));
#28789=DIRECTION('',(-1.,0.,0.));
#28790=DIRECTION('center_axis',(1.,0.,0.));
#28791=DIRECTION('ref_axis',(0.,0.,-1.));
#28792=DIRECTION('',(-1.,0.,0.));
#28793=DIRECTION('center_axis',(1.,0.,0.));
#28794=DIRECTION('ref_axis',(0.,0.,-1.));
#28795=DIRECTION('',(-1.,0.,0.));
#28796=DIRECTION('center_axis',(1.,0.,0.));
#28797=DIRECTION('ref_axis',(0.,0.,-1.));
#28798=DIRECTION('',(-1.,0.,0.));
#28799=DIRECTION('center_axis',(1.,0.,0.));
#28800=DIRECTION('ref_axis',(0.,0.,-1.));
#28801=DIRECTION('',(-1.,0.,0.));
#28802=DIRECTION('center_axis',(1.,0.,0.));
#28803=DIRECTION('ref_axis',(0.,0.,-1.));
#28804=DIRECTION('',(-1.,0.,0.));
#28805=DIRECTION('center_axis',(1.,0.,0.));
#28806=DIRECTION('ref_axis',(0.,0.,-1.));
#28807=DIRECTION('',(-1.,0.,0.));
#28808=DIRECTION('center_axis',(1.,0.,0.));
#28809=DIRECTION('ref_axis',(0.,0.,-1.));
#28810=DIRECTION('',(-1.,0.,0.));
#28811=DIRECTION('center_axis',(1.,0.,0.));
#28812=DIRECTION('ref_axis',(0.,0.,-1.));
#28813=DIRECTION('',(-1.,0.,0.));
#28814=DIRECTION('center_axis',(1.,0.,0.));
#28815=DIRECTION('ref_axis',(0.,0.,-1.));
#28816=DIRECTION('',(-1.,0.,0.));
#28817=DIRECTION('center_axis',(1.,0.,0.));
#28818=DIRECTION('ref_axis',(0.,0.,-1.));
#28819=DIRECTION('',(-1.,0.,0.));
#28820=DIRECTION('center_axis',(1.,0.,0.));
#28821=DIRECTION('ref_axis',(0.,0.,-1.));
#28822=DIRECTION('',(-1.,0.,0.));
#28823=DIRECTION('center_axis',(1.,0.,0.));
#28824=DIRECTION('ref_axis',(0.,0.,-1.));
#28825=DIRECTION('',(-1.,0.,0.));
#28826=DIRECTION('center_axis',(1.,0.,0.));
#28827=DIRECTION('ref_axis',(0.,0.,-1.));
#28828=DIRECTION('',(-1.,0.,0.));
#28829=DIRECTION('center_axis',(1.,0.,0.));
#28830=DIRECTION('ref_axis',(0.,0.,-1.));
#28831=DIRECTION('',(-1.,0.,0.));
#28832=DIRECTION('center_axis',(1.,0.,0.));
#28833=DIRECTION('ref_axis',(0.,0.,-1.));
#28834=DIRECTION('',(-1.,0.,0.));
#28835=DIRECTION('center_axis',(1.,0.,0.));
#28836=DIRECTION('ref_axis',(0.,0.,-1.));
#28837=DIRECTION('',(-1.,0.,0.));
#28838=DIRECTION('center_axis',(1.,0.,0.));
#28839=DIRECTION('ref_axis',(0.,0.,-1.));
#28840=DIRECTION('',(-1.,0.,0.));
#28841=DIRECTION('center_axis',(1.,0.,0.));
#28842=DIRECTION('ref_axis',(0.,0.,-1.));
#28843=DIRECTION('',(-1.,0.,0.));
#28844=DIRECTION('center_axis',(1.,0.,0.));
#28845=DIRECTION('ref_axis',(0.,0.,-1.));
#28846=DIRECTION('',(-1.,0.,0.));
#28847=DIRECTION('center_axis',(1.,0.,0.));
#28848=DIRECTION('ref_axis',(0.,0.,-1.));
#28849=DIRECTION('',(-1.,0.,0.));
#28850=DIRECTION('center_axis',(1.,0.,0.));
#28851=DIRECTION('ref_axis',(0.,0.,-1.));
#28852=DIRECTION('',(-1.,0.,0.));
#28853=DIRECTION('center_axis',(1.,0.,0.));
#28854=DIRECTION('ref_axis',(0.,0.,-1.));
#28855=DIRECTION('',(-1.,0.,0.));
#28856=DIRECTION('center_axis',(1.,0.,0.));
#28857=DIRECTION('ref_axis',(0.,0.,-1.));
#28858=DIRECTION('',(-1.,0.,0.));
#28859=DIRECTION('center_axis',(1.,0.,0.));
#28860=DIRECTION('ref_axis',(0.,0.,-1.));
#28861=DIRECTION('',(-1.,0.,0.));
#28862=DIRECTION('center_axis',(1.,0.,0.));
#28863=DIRECTION('ref_axis',(0.,0.,-1.));
#28864=DIRECTION('',(-1.,0.,0.));
#28865=DIRECTION('center_axis',(1.,0.,0.));
#28866=DIRECTION('ref_axis',(0.,0.,-1.));
#28867=DIRECTION('',(-1.,0.,0.));
#28868=DIRECTION('center_axis',(1.,0.,0.));
#28869=DIRECTION('ref_axis',(0.,0.,-1.));
#28870=DIRECTION('',(-1.,0.,0.));
#28871=DIRECTION('center_axis',(1.,0.,0.));
#28872=DIRECTION('ref_axis',(0.,0.,-1.));
#28873=DIRECTION('',(-1.,0.,0.));
#28874=DIRECTION('center_axis',(1.,0.,0.));
#28875=DIRECTION('ref_axis',(0.,0.,-1.));
#28876=DIRECTION('',(-1.,0.,0.));
#28877=DIRECTION('center_axis',(1.,0.,0.));
#28878=DIRECTION('ref_axis',(0.,0.,-1.));
#28879=DIRECTION('',(-1.,0.,0.));
#28880=DIRECTION('center_axis',(1.,0.,0.));
#28881=DIRECTION('ref_axis',(0.,0.,-1.));
#28882=DIRECTION('',(-1.,0.,0.));
#28883=DIRECTION('center_axis',(1.,0.,0.));
#28884=DIRECTION('ref_axis',(0.,0.,-1.));
#28885=DIRECTION('',(-1.,0.,0.));
#28886=DIRECTION('center_axis',(1.,0.,0.));
#28887=DIRECTION('ref_axis',(0.,0.,-1.));
#28888=DIRECTION('',(-1.,0.,0.));
#28889=DIRECTION('center_axis',(1.,0.,0.));
#28890=DIRECTION('ref_axis',(0.,0.,-1.));
#28891=DIRECTION('',(-1.,0.,0.));
#28892=DIRECTION('center_axis',(1.,0.,0.));
#28893=DIRECTION('ref_axis',(0.,-1.17203152359781E-12,-1.));
#28894=DIRECTION('',(1.,0.,0.));
#28895=DIRECTION('center_axis',(1.,0.,0.));
#28896=DIRECTION('ref_axis',(0.,-1.17203152359781E-12,-1.));
#28897=DIRECTION('center_axis',(1.,0.,0.));
#28898=DIRECTION('ref_axis',(0.,-1.17203152359781E-12,-1.));
#28899=DIRECTION('',(1.,0.,0.));
#28900=DIRECTION('center_axis',(1.,0.,0.));
#28901=DIRECTION('ref_axis',(0.,-1.17203152359781E-12,-1.));
#28902=DIRECTION('center_axis',(1.,0.,0.));
#28903=DIRECTION('ref_axis',(0.,-1.17203152359781E-12,-1.));
#28904=DIRECTION('',(1.,0.,0.));
#28905=DIRECTION('center_axis',(1.,0.,0.));
#28906=DIRECTION('ref_axis',(0.,-1.17203152359781E-12,-1.));
#28907=DIRECTION('',(1.,0.,0.));
#28908=DIRECTION('center_axis',(1.,0.,0.));
#28909=DIRECTION('ref_axis',(0.,-1.17203152359781E-12,-1.));
#28910=DIRECTION('',(1.,0.,0.));
#28911=DIRECTION('center_axis',(1.,0.,0.));
#28912=DIRECTION('ref_axis',(0.,-1.17203152359781E-12,-1.));
#28913=DIRECTION('',(1.,0.,0.));
#28914=DIRECTION('center_axis',(1.,0.,0.));
#28915=DIRECTION('ref_axis',(0.,-1.17203152359781E-12,-1.));
#28916=DIRECTION('',(1.,0.,0.));
#28917=DIRECTION('center_axis',(1.,0.,0.));
#28918=DIRECTION('ref_axis',(0.,-1.17203152359781E-12,-1.));
#28919=DIRECTION('',(1.,0.,0.));
#28920=DIRECTION('center_axis',(1.,0.,0.));
#28921=DIRECTION('ref_axis',(0.,-1.17203152359781E-12,-1.));
#28922=DIRECTION('',(1.,0.,0.));
#28923=DIRECTION('center_axis',(1.,0.,0.));
#28924=DIRECTION('ref_axis',(0.,-1.17203152359781E-12,-1.));
#28925=DIRECTION('',(1.,0.,0.));
#28926=DIRECTION('center_axis',(1.,0.,0.));
#28927=DIRECTION('ref_axis',(0.,-1.17203152359781E-12,-1.));
#28928=DIRECTION('',(1.,0.,0.));
#28929=DIRECTION('center_axis',(1.,0.,0.));
#28930=DIRECTION('ref_axis',(0.,-1.17203152359781E-12,-1.));
#28931=DIRECTION('',(1.,0.,0.));
#28932=DIRECTION('center_axis',(1.,0.,0.));
#28933=DIRECTION('ref_axis',(0.,-1.17203152359781E-12,-1.));
#28934=DIRECTION('',(1.,0.,0.));
#28935=DIRECTION('center_axis',(1.,0.,0.));
#28936=DIRECTION('ref_axis',(0.,-1.17203152359781E-12,-1.));
#28937=DIRECTION('',(1.,0.,0.));
#28938=DIRECTION('center_axis',(1.,0.,0.));
#28939=DIRECTION('ref_axis',(0.,-1.17203152359781E-12,-1.));
#28940=DIRECTION('',(1.,0.,0.));
#28941=DIRECTION('center_axis',(1.,0.,0.));
#28942=DIRECTION('ref_axis',(0.,-1.17203152359781E-12,-1.));
#28943=DIRECTION('',(1.,0.,0.));
#28944=DIRECTION('center_axis',(1.,0.,0.));
#28945=DIRECTION('ref_axis',(0.,-1.17203152359781E-12,-1.));
#28946=DIRECTION('',(1.,0.,0.));
#28947=DIRECTION('center_axis',(1.,0.,0.));
#28948=DIRECTION('ref_axis',(0.,-1.17203152359781E-12,-1.));
#28949=DIRECTION('',(1.,0.,0.));
#28950=DIRECTION('center_axis',(1.,0.,0.));
#28951=DIRECTION('ref_axis',(0.,-1.17203152359781E-12,-1.));
#28952=DIRECTION('',(1.,0.,0.));
#28953=DIRECTION('center_axis',(1.,0.,0.));
#28954=DIRECTION('ref_axis',(0.,-1.17203152359781E-12,-1.));
#28955=DIRECTION('',(1.,0.,0.));
#28956=DIRECTION('center_axis',(1.,0.,0.));
#28957=DIRECTION('ref_axis',(0.,-1.17203152359781E-12,-1.));
#28958=DIRECTION('',(1.,0.,0.));
#28959=DIRECTION('center_axis',(1.,0.,0.));
#28960=DIRECTION('ref_axis',(0.,-1.17203152359781E-12,-1.));
#28961=DIRECTION('',(1.,0.,0.));
#28962=DIRECTION('center_axis',(1.,0.,0.));
#28963=DIRECTION('ref_axis',(0.,-1.17203152359781E-12,-1.));
#28964=DIRECTION('',(1.,0.,0.));
#28965=DIRECTION('center_axis',(1.,0.,0.));
#28966=DIRECTION('ref_axis',(0.,-1.17203152359781E-12,-1.));
#28967=DIRECTION('',(1.,0.,0.));
#28968=DIRECTION('center_axis',(1.,0.,0.));
#28969=DIRECTION('ref_axis',(0.,-1.17203152359781E-12,-1.));
#28970=DIRECTION('',(1.,0.,0.));
#28971=DIRECTION('center_axis',(1.,0.,0.));
#28972=DIRECTION('ref_axis',(0.,-1.17203152359781E-12,-1.));
#28973=DIRECTION('',(1.,0.,0.));
#28974=DIRECTION('center_axis',(1.,0.,0.));
#28975=DIRECTION('ref_axis',(0.,-1.17203152359781E-12,-1.));
#28976=DIRECTION('',(1.,0.,0.));
#28977=DIRECTION('center_axis',(1.,0.,0.));
#28978=DIRECTION('ref_axis',(0.,-1.17203152359781E-12,-1.));
#28979=DIRECTION('',(1.,0.,0.));
#28980=DIRECTION('center_axis',(1.,0.,0.));
#28981=DIRECTION('ref_axis',(0.,-1.17203152359781E-12,-1.));
#28982=DIRECTION('',(1.,0.,0.));
#28983=DIRECTION('center_axis',(1.,0.,0.));
#28984=DIRECTION('ref_axis',(0.,-1.17203152359781E-12,-1.));
#28985=DIRECTION('',(1.,0.,0.));
#28986=DIRECTION('center_axis',(1.,0.,0.));
#28987=DIRECTION('ref_axis',(0.,-1.17203152359781E-12,-1.));
#28988=DIRECTION('',(1.,0.,0.));
#28989=DIRECTION('center_axis',(1.,0.,0.));
#28990=DIRECTION('ref_axis',(0.,-1.17203152359781E-12,-1.));
#28991=DIRECTION('',(1.,0.,0.));
#28992=DIRECTION('center_axis',(1.,0.,0.));
#28993=DIRECTION('ref_axis',(0.,-1.17203152359781E-12,-1.));
#28994=DIRECTION('',(1.,0.,0.));
#28995=DIRECTION('center_axis',(1.,0.,0.));
#28996=DIRECTION('ref_axis',(0.,-1.17203152359781E-12,-1.));
#28997=DIRECTION('',(1.,0.,0.));
#28998=DIRECTION('center_axis',(1.,0.,0.));
#28999=DIRECTION('ref_axis',(0.,-1.17203152359781E-12,-1.));
#29000=DIRECTION('',(1.,0.,0.));
#29001=DIRECTION('center_axis',(1.,0.,0.));
#29002=DIRECTION('ref_axis',(0.,-1.17203152359781E-12,-1.));
#29003=DIRECTION('',(1.,0.,0.));
#29004=DIRECTION('center_axis',(1.,0.,0.));
#29005=DIRECTION('ref_axis',(0.,-1.17203152359781E-12,-1.));
#29006=DIRECTION('',(1.,0.,0.));
#29007=DIRECTION('center_axis',(1.,0.,0.));
#29008=DIRECTION('ref_axis',(0.,-1.17203152359781E-12,-1.));
#29009=DIRECTION('',(1.,0.,0.));
#29010=DIRECTION('center_axis',(1.,0.,0.));
#29011=DIRECTION('ref_axis',(0.,-1.17203152359781E-12,-1.));
#29012=DIRECTION('',(1.,0.,0.));
#29013=DIRECTION('center_axis',(1.,0.,0.));
#29014=DIRECTION('ref_axis',(0.,-1.17203152359781E-12,-1.));
#29015=DIRECTION('',(1.,0.,0.));
#29016=DIRECTION('center_axis',(1.,0.,0.));
#29017=DIRECTION('ref_axis',(0.,-1.17203152359781E-12,-1.));
#29018=DIRECTION('',(1.,0.,0.));
#29019=DIRECTION('center_axis',(1.,0.,0.));
#29020=DIRECTION('ref_axis',(0.,-1.17203152359781E-12,-1.));
#29021=DIRECTION('',(1.,0.,0.));
#29022=DIRECTION('center_axis',(1.,0.,0.));
#29023=DIRECTION('ref_axis',(0.,-1.17203152359781E-12,-1.));
#29024=DIRECTION('',(1.,0.,0.));
#29025=DIRECTION('center_axis',(1.,0.,0.));
#29026=DIRECTION('ref_axis',(0.,-1.17203152359781E-12,-1.));
#29027=DIRECTION('',(1.,0.,0.));
#29028=DIRECTION('center_axis',(1.,0.,0.));
#29029=DIRECTION('ref_axis',(0.,-1.17203152359781E-12,-1.));
#29030=DIRECTION('',(1.,0.,0.));
#29031=DIRECTION('center_axis',(1.,0.,0.));
#29032=DIRECTION('ref_axis',(0.,-1.17203152359781E-12,-1.));
#29033=DIRECTION('',(1.,0.,0.));
#29034=DIRECTION('center_axis',(1.,0.,0.));
#29035=DIRECTION('ref_axis',(0.,-1.17203152359781E-12,-1.));
#29036=DIRECTION('',(1.,0.,0.));
#29037=DIRECTION('center_axis',(1.,0.,0.));
#29038=DIRECTION('ref_axis',(0.,-1.17203152359781E-12,-1.));
#29039=DIRECTION('',(1.,0.,0.));
#29040=DIRECTION('center_axis',(1.,0.,0.));
#29041=DIRECTION('ref_axis',(0.,-1.17203152359781E-12,-1.));
#29042=DIRECTION('',(1.,0.,0.));
#29043=DIRECTION('center_axis',(1.,0.,0.));
#29044=DIRECTION('ref_axis',(0.,-1.17203152359781E-12,-1.));
#29045=DIRECTION('',(1.,0.,0.));
#29046=DIRECTION('center_axis',(1.,0.,0.));
#29047=DIRECTION('ref_axis',(0.,-1.17203152359781E-12,-1.));
#29048=DIRECTION('',(1.,0.,0.));
#29049=DIRECTION('center_axis',(1.,0.,0.));
#29050=DIRECTION('ref_axis',(0.,-1.17203152359781E-12,-1.));
#29051=DIRECTION('',(1.,0.,0.));
#29052=DIRECTION('center_axis',(1.,0.,0.));
#29053=DIRECTION('ref_axis',(0.,-1.17203152359781E-12,-1.));
#29054=DIRECTION('',(1.,0.,0.));
#29055=DIRECTION('center_axis',(1.,0.,0.));
#29056=DIRECTION('ref_axis',(0.,-1.17203152359781E-12,-1.));
#29057=DIRECTION('',(1.,0.,0.));
#29058=DIRECTION('center_axis',(1.,0.,0.));
#29059=DIRECTION('ref_axis',(0.,-1.17203152359781E-12,-1.));
#29060=DIRECTION('',(1.,0.,0.));
#29061=DIRECTION('center_axis',(1.,0.,0.));
#29062=DIRECTION('ref_axis',(0.,-1.17203152359781E-12,-1.));
#29063=DIRECTION('',(1.,0.,0.));
#29064=DIRECTION('center_axis',(1.,0.,0.));
#29065=DIRECTION('ref_axis',(0.,-1.17203152359781E-12,-1.));
#29066=DIRECTION('',(1.,0.,0.));
#29067=DIRECTION('center_axis',(1.,0.,0.));
#29068=DIRECTION('ref_axis',(0.,-1.17203152359781E-12,-1.));
#29069=DIRECTION('',(1.,0.,0.));
#29070=DIRECTION('center_axis',(1.,0.,0.));
#29071=DIRECTION('ref_axis',(0.,-1.17203152359781E-12,-1.));
#29072=DIRECTION('',(1.,0.,0.));
#29073=DIRECTION('center_axis',(1.,0.,0.));
#29074=DIRECTION('ref_axis',(0.,-1.17203152359781E-12,-1.));
#29075=DIRECTION('',(1.,0.,0.));
#29076=DIRECTION('center_axis',(1.,0.,0.));
#29077=DIRECTION('ref_axis',(0.,-1.17203152359781E-12,-1.));
#29078=DIRECTION('',(1.,0.,0.));
#29079=DIRECTION('center_axis',(1.,0.,0.));
#29080=DIRECTION('ref_axis',(0.,-1.17203152359781E-12,-1.));
#29081=DIRECTION('',(1.,0.,0.));
#29082=DIRECTION('center_axis',(1.,0.,0.));
#29083=DIRECTION('ref_axis',(0.,-1.17203152359781E-12,-1.));
#29084=DIRECTION('',(1.,0.,0.));
#29085=DIRECTION('center_axis',(1.,0.,0.));
#29086=DIRECTION('ref_axis',(0.,0.,-1.));
#29087=DIRECTION('center_axis',(1.,0.,0.));
#29088=DIRECTION('ref_axis',(0.,0.,-1.));
#29089=DIRECTION('center_axis',(-1.,0.,0.));
#29090=DIRECTION('ref_axis',(0.,-1.17203152359781E-12,-1.));
#29091=DIRECTION('center_axis',(1.,0.,0.));
#29092=DIRECTION('ref_axis',(0.,0.,-1.));
#29093=DIRECTION('',(-1.,0.,0.));
#29094=DIRECTION('center_axis',(1.,0.,0.));
#29095=DIRECTION('ref_axis',(0.,0.,-1.));
#29096=DIRECTION('center_axis',(1.,0.,0.));
#29097=DIRECTION('ref_axis',(0.,0.,-1.));
#29098=DIRECTION('center_axis',(1.,0.,0.));
#29099=DIRECTION('ref_axis',(0.,-1.17203152359781E-12,-1.));
#29100=DIRECTION('center_axis',(0.,1.,0.));
#29101=DIRECTION('ref_axis',(0.,0.,1.));
#29102=DIRECTION('',(-1.,0.,0.));
#29103=DIRECTION('',(0.,0.,1.));
#29104=DIRECTION('',(1.,0.,0.));
#29105=DIRECTION('',(0.,0.,1.));
#29106=DIRECTION('center_axis',(1.,0.,0.));
#29107=DIRECTION('ref_axis',(0.,0.,-1.));
#29108=DIRECTION('center_axis',(-1.,0.,0.));
#29109=DIRECTION('ref_axis',(0.,0.,-1.));
#29110=DIRECTION('',(0.,-1.,0.));
#29111=DIRECTION('',(0.,0.,-1.));
#29112=DIRECTION('center_axis',(0.,0.,1.));
#29113=DIRECTION('ref_axis',(0.,-1.,0.));
#29114=DIRECTION('',(0.,-1.,0.));
#29115=DIRECTION('',(1.,0.,0.));
#29116=DIRECTION('center_axis',(0.,-1.,0.));
#29117=DIRECTION('ref_axis',(0.,0.,-1.));
#29118=DIRECTION('',(1.,0.,0.));
#29119=DIRECTION('',(0.,0.,-1.));
#29120=DIRECTION('center_axis',(1.,0.,0.));
#29121=DIRECTION('ref_axis',(0.,0.,-1.));
#29122=DIRECTION('center_axis',(1.,0.,0.));
#29123=DIRECTION('ref_axis',(0.,0.,-1.));
#29124=DIRECTION('center_axis',(1.,0.,0.));
#29125=DIRECTION('ref_axis',(0.,0.,-1.));
#29126=DIRECTION('center_axis',(1.,0.,0.));
#29127=DIRECTION('ref_axis',(0.,0.,-1.));
#29128=DIRECTION('',(-1.,0.,0.));
#29129=DIRECTION('center_axis',(-1.,0.,0.));
#29130=DIRECTION('ref_axis',(0.,0.,-1.));
#29131=DIRECTION('center_axis',(1.,0.,0.));
#29132=DIRECTION('ref_axis',(0.,0.,-1.));
#29133=DIRECTION('center_axis',(1.,0.,0.));
#29134=DIRECTION('ref_axis',(0.,0.,-1.));
#29135=DIRECTION('center_axis',(1.,0.,0.));
#29136=DIRECTION('ref_axis',(0.,0.,-1.));
#29137=DIRECTION('center_axis',(-1.,0.,0.));
#29138=DIRECTION('ref_axis',(0.,0.,-1.));
#29139=DIRECTION('center_axis',(1.,0.,0.));
#29140=DIRECTION('ref_axis',(0.,0.,-1.));
#29141=DIRECTION('center_axis',(1.,0.,0.));
#29142=DIRECTION('ref_axis',(0.,0.,-1.));
#29143=DIRECTION('',(-1.,0.,0.));
#29144=DIRECTION('center_axis',(1.,0.,0.));
#29145=DIRECTION('ref_axis',(0.,0.,-1.));
#29146=DIRECTION('center_axis',(1.,0.,0.));
#29147=DIRECTION('ref_axis',(0.,0.,-1.));
#29148=DIRECTION('axis',(0.,0.,1.));
#29149=DIRECTION('refdir',(1.,0.,0.));
#29150=DIRECTION('center_axis',(1.,0.,0.));
#29151=DIRECTION('ref_axis',(0.,0.,-1.));
#29152=DIRECTION('center_axis',(-1.,0.,0.));
#29153=DIRECTION('ref_axis',(0.,0.,-1.));
#29154=DIRECTION('',(-1.,0.,0.));
#29155=DIRECTION('center_axis',(-1.,0.,0.));
#29156=DIRECTION('ref_axis',(0.,0.,-1.));
#29157=DIRECTION('center_axis',(1.,0.,0.));
#29158=DIRECTION('ref_axis',(0.,0.,-1.));
#29159=DIRECTION('center_axis',(1.,0.,0.));
#29160=DIRECTION('ref_axis',(0.,0.,-1.));
#29161=DIRECTION('',(-1.,0.,0.));
#29162=DIRECTION('center_axis',(1.,0.,0.));
#29163=DIRECTION('ref_axis',(0.,0.,-1.));
#29164=DIRECTION('center_axis',(1.,0.,0.));
#29165=DIRECTION('ref_axis',(0.,0.,-1.));
#29166=DIRECTION('center_axis',(1.,0.,0.));
#29167=DIRECTION('ref_axis',(0.,0.,-1.));
#29168=DIRECTION('axis',(0.,0.,1.));
#29169=DIRECTION('refdir',(1.,0.,0.));
#29170=DIRECTION('center_axis',(0.,1.,0.));
#29171=DIRECTION('ref_axis',(1.,0.,0.));
#29172=DIRECTION('',(1.,0.,0.));
#29173=DIRECTION('center_axis',(0.,1.,0.));
#29174=DIRECTION('ref_axis',(1.,0.,0.));
#29175=DIRECTION('center_axis',(0.,1.,0.));
#29176=DIRECTION('ref_axis',(1.,0.,0.));
#29177=DIRECTION('center_axis',(0.,1.,0.));
#29178=DIRECTION('ref_axis',(1.,0.,0.));
#29179=DIRECTION('',(0.,1.,0.));
#29180=DIRECTION('center_axis',(0.,1.,0.));
#29181=DIRECTION('ref_axis',(1.,0.,0.));
#29182=DIRECTION('',(-1.,0.,0.));
#29183=DIRECTION('center_axis',(1.,0.,0.));
#29184=DIRECTION('ref_axis',(0.,0.,-1.));
#29185=DIRECTION('center_axis',(-1.,0.,0.));
#29186=DIRECTION('ref_axis',(0.,0.,-1.));
#29187=DIRECTION('',(-1.,0.,0.));
#29188=DIRECTION('center_axis',(-1.,0.,0.));
#29189=DIRECTION('ref_axis',(0.,0.,-1.));
#29190=DIRECTION('center_axis',(1.,0.,0.));
#29191=DIRECTION('ref_axis',(0.,0.,-1.));
#29192=DIRECTION('center_axis',(1.,0.,0.));
#29193=DIRECTION('ref_axis',(0.,0.,-1.));
#29194=DIRECTION('',(-1.,0.,0.));
#29195=DIRECTION('center_axis',(1.,0.,0.));
#29196=DIRECTION('ref_axis',(0.,0.,-1.));
#29197=DIRECTION('center_axis',(1.,0.,0.));
#29198=DIRECTION('ref_axis',(0.,0.,-1.));
#29199=DIRECTION('center_axis',(1.,0.,0.));
#29200=DIRECTION('ref_axis',(0.,0.,-1.));
#29201=DIRECTION('axis',(0.,0.,1.));
#29202=DIRECTION('refdir',(1.,0.,0.));
#29203=DIRECTION('center_axis',(1.,0.,0.));
#29204=DIRECTION('ref_axis',(0.,0.,-1.));
#29205=DIRECTION('center_axis',(1.,0.,0.));
#29206=DIRECTION('ref_axis',(0.,0.,-1.));
#29207=DIRECTION('',(1.,0.,0.));
#29208=DIRECTION('center_axis',(-1.,0.,0.));
#29209=DIRECTION('ref_axis',(0.,0.,-1.));
#29210=DIRECTION('center_axis',(0.,1.,0.));
#29211=DIRECTION('ref_axis',(1.,0.,0.));
#29212=DIRECTION('',(1.,0.,0.));
#29213=DIRECTION('center_axis',(0.,1.,0.));
#29214=DIRECTION('ref_axis',(1.,0.,0.));
#29215=DIRECTION('center_axis',(0.,1.,0.));
#29216=DIRECTION('ref_axis',(1.,0.,0.));
#29217=DIRECTION('center_axis',(0.,1.,0.));
#29218=DIRECTION('ref_axis',(1.,0.,0.));
#29219=DIRECTION('',(0.,1.,0.));
#29220=DIRECTION('center_axis',(0.,1.,0.));
#29221=DIRECTION('ref_axis',(1.,0.,0.));
#29222=DIRECTION('',(-1.,0.,0.));
#29223=DIRECTION('center_axis',(0.,-1.,0.));
#29224=DIRECTION('ref_axis',(0.,0.,-1.));
#29225=DIRECTION('',(0.,0.,1.));
#29226=DIRECTION('',(1.,0.,0.));
#29227=DIRECTION('',(0.,0.,-1.));
#29228=DIRECTION('',(1.,0.,0.));
#29229=DIRECTION('',(0.,0.,-1.));
#29230=DIRECTION('',(-1.,0.,0.));
#29231=DIRECTION('center_axis',(0.,0.,-1.));
#29232=DIRECTION('ref_axis',(0.,1.,0.));
#29233=DIRECTION('',(0.,-1.,0.));
#29234=DIRECTION('',(1.,0.,0.));
#29235=DIRECTION('',(0.,1.,0.));
#29236=DIRECTION('center_axis',(0.,1.,0.));
#29237=DIRECTION('ref_axis',(0.,0.,1.));
#29238=DIRECTION('',(0.,0.,-1.));
#29239=DIRECTION('',(1.,0.,0.));
#29240=DIRECTION('',(0.,0.,1.));
#29241=DIRECTION('',(-1.,0.,0.));
#29242=DIRECTION('',(0.,0.,1.));
#29243=DIRECTION('center_axis',(1.,0.,0.));
#29244=DIRECTION('ref_axis',(0.,0.,-1.));
#29245=DIRECTION('center_axis',(1.,0.,0.));
#29246=DIRECTION('ref_axis',(0.,0.,-1.));
#29247=DIRECTION('center_axis',(-1.,0.,0.));
#29248=DIRECTION('ref_axis',(0.,0.,-1.));
#29249=DIRECTION('center_axis',(1.,0.,0.));
#29250=DIRECTION('ref_axis',(0.,0.,-1.));
#29251=DIRECTION('center_axis',(1.,0.,0.));
#29252=DIRECTION('ref_axis',(0.,0.,-1.));
#29253=DIRECTION('center_axis',(1.,0.,0.));
#29254=DIRECTION('ref_axis',(0.,0.,-1.));
#29255=DIRECTION('center_axis',(1.,0.,0.));
#29256=DIRECTION('ref_axis',(0.,0.,-1.));
#29257=DIRECTION('',(-1.,0.,0.));
#29258=DIRECTION('center_axis',(1.,0.,0.));
#29259=DIRECTION('ref_axis',(0.,1.22464679914735E-16,1.));
#29260=DIRECTION('center_axis',(-1.,0.,0.));
#29261=DIRECTION('ref_axis',(0.,0.,-1.));
#29262=DIRECTION('center_axis',(1.,0.,0.));
#29263=DIRECTION('ref_axis',(0.,1.22464679914735E-16,1.));
#29264=DIRECTION('center_axis',(1.,0.,0.));
#29265=DIRECTION('ref_axis',(0.,0.,-1.));
#29266=DIRECTION('center_axis',(1.,0.,0.));
#29267=DIRECTION('ref_axis',(0.,0.,-1.));
#29268=DIRECTION('axis',(0.,0.,1.));
#29269=DIRECTION('refdir',(1.,0.,0.));
#29270=DIRECTION('center_axis',(1.,0.,0.));
#29271=DIRECTION('ref_axis',(0.,0.,-1.));
#29272=DIRECTION('center_axis',(-1.,0.,0.));
#29273=DIRECTION('ref_axis',(0.,0.,-1.));
#29274=DIRECTION('',(-1.,0.,0.));
#29275=DIRECTION('center_axis',(-1.,0.,0.));
#29276=DIRECTION('ref_axis',(0.,0.,-1.));
#29277=DIRECTION('center_axis',(1.,0.,0.));
#29278=DIRECTION('ref_axis',(0.,0.,-1.));
#29279=DIRECTION('center_axis',(1.,0.,0.));
#29280=DIRECTION('ref_axis',(0.,0.,-1.));
#29281=DIRECTION('',(-1.,0.,0.));
#29282=DIRECTION('center_axis',(1.,0.,0.));
#29283=DIRECTION('ref_axis',(0.,0.,-1.));
#29284=DIRECTION('center_axis',(1.,0.,0.));
#29285=DIRECTION('ref_axis',(0.,0.,-1.));
#29286=DIRECTION('center_axis',(1.,0.,0.));
#29287=DIRECTION('ref_axis',(0.,0.,-1.));
#29288=DIRECTION('axis',(0.,0.,1.));
#29289=DIRECTION('refdir',(1.,0.,0.));
#29290=DIRECTION('center_axis',(1.,0.,0.));
#29291=DIRECTION('ref_axis',(0.,0.,-1.));
#29292=DIRECTION('center_axis',(-1.,0.,0.));
#29293=DIRECTION('ref_axis',(0.,0.,-1.));
#29294=DIRECTION('',(-1.,0.,0.));
#29295=DIRECTION('center_axis',(-1.,0.,0.));
#29296=DIRECTION('ref_axis',(0.,0.,-1.));
#29297=DIRECTION('center_axis',(1.,0.,0.));
#29298=DIRECTION('ref_axis',(0.,0.,-1.));
#29299=DIRECTION('center_axis',(1.,0.,0.));
#29300=DIRECTION('ref_axis',(0.,0.,-1.));
#29301=DIRECTION('',(-1.,0.,0.));
#29302=DIRECTION('center_axis',(1.,0.,0.));
#29303=DIRECTION('ref_axis',(0.,0.,-1.));
#29304=DIRECTION('center_axis',(1.,0.,0.));
#29305=DIRECTION('ref_axis',(0.,0.,-1.));
#29306=DIRECTION('center_axis',(1.,0.,0.));
#29307=DIRECTION('ref_axis',(0.,0.,-1.));
#29308=DIRECTION('axis',(0.,0.,1.));
#29309=DIRECTION('refdir',(1.,0.,0.));
#29310=DIRECTION('center_axis',(1.,0.,0.));
#29311=DIRECTION('ref_axis',(0.,0.,-1.));
#29312=DIRECTION('',(0.,-0.707106781186547,-0.707106781186548));
#29313=DIRECTION('',(0.,-1.,0.));
#29314=DIRECTION('',(0.,-0.707106781186547,0.707106781186548));
#29315=DIRECTION('',(0.,0.,1.));
#29316=DIRECTION('',(0.,0.707106781186547,0.707106781186548));
#29317=DIRECTION('',(0.,1.,0.));
#29318=DIRECTION('',(0.,0.707106781186547,-0.707106781186548));
#29319=DIRECTION('',(0.,0.,-1.));
#29320=DIRECTION('center_axis',(0.,0.707106781186548,-0.707106781186547));
#29321=DIRECTION('ref_axis',(-1.,0.,0.));
#29322=DIRECTION('',(1.,0.,0.));
#29323=DIRECTION('',(0.,-0.707106781186547,-0.707106781186548));
#29324=DIRECTION('',(-1.,0.,0.));
#29325=DIRECTION('center_axis',(0.,1.,0.));
#29326=DIRECTION('ref_axis',(-1.,0.,0.));
#29327=DIRECTION('',(-1.,0.,0.));
#29328=DIRECTION('',(0.,0.,-1.));
#29329=DIRECTION('center_axis',(0.,0.707106781186548,0.707106781186547));
#29330=DIRECTION('ref_axis',(1.,0.,0.));
#29331=DIRECTION('',(1.,0.,0.));
#29332=DIRECTION('',(0.,0.707106781186547,-0.707106781186548));
#29333=DIRECTION('center_axis',(0.,0.,1.));
#29334=DIRECTION('ref_axis',(1.,0.,0.));
#29335=DIRECTION('',(-1.,0.,0.));
#29336=DIRECTION('',(0.,1.,0.));
#29337=DIRECTION('center_axis',(1.,0.,0.));
#29338=DIRECTION('ref_axis',(0.,0.,-1.));
#29339=DIRECTION('',(0.,-0.707106781186547,0.707106781186548));
#29340=DIRECTION('',(0.,-1.,0.));
#29341=DIRECTION('',(0.,0.707106781186547,0.707106781186548));
#29342=DIRECTION('',(0.,0.,1.));
#29343=DIRECTION('center_axis',(0.,0.,1.));
#29344=DIRECTION('ref_axis',(1.,0.,0.));
#29345=DIRECTION('',(1.,0.,0.));
#29346=DIRECTION('center_axis',(0.,-0.707106781186548,0.707106781186547));
#29347=DIRECTION('ref_axis',(1.,0.,0.));
#29348=DIRECTION('',(1.,0.,0.));
#29349=DIRECTION('center_axis',(0.,-0.707106781186548,-0.707106781186547));
#29350=DIRECTION('ref_axis',(-1.,0.,0.));
#29351=DIRECTION('',(-1.,0.,0.));
#29352=DIRECTION('center_axis',(0.,-1.,0.));
#29353=DIRECTION('ref_axis',(1.,0.,0.));
#29354=DIRECTION('axis',(0.,0.,1.));
#29355=DIRECTION('refdir',(1.,0.,0.));
#29356=DIRECTION('center_axis',(0.866025403784439,0.,-0.5));
#29357=DIRECTION('ref_axis',(0.5,0.,0.866025403784439));
#29358=DIRECTION('',(0.5,0.,0.866025403784439));
#29359=DIRECTION('',(0.,-1.,0.));
#29360=DIRECTION('',(0.5,0.,0.866025403784439));
#29361=DIRECTION('',(0.,-1.,0.));
#29362=DIRECTION('center_axis',(1.92296268638356E-16,0.,-1.));
#29363=DIRECTION('ref_axis',(1.,0.,1.92296268638356E-16));
#29364=DIRECTION('',(1.,0.,1.92296268638356E-16));
#29365=DIRECTION('',(0.,-1.,0.));
#29366=DIRECTION('',(1.,0.,1.92296268638356E-16));
#29367=DIRECTION('center_axis',(-0.866025403784439,0.,-0.5));
#29368=DIRECTION('ref_axis',(0.5,0.,-0.866025403784439));
#29369=DIRECTION('',(0.5,0.,-0.866025403784439));
#29370=DIRECTION('',(0.,-1.,0.));
#29371=DIRECTION('',(0.5,0.,-0.866025403784438));
#29372=DIRECTION('center_axis',(-0.866025403784439,0.,0.5));
#29373=DIRECTION('ref_axis',(-0.5,0.,-0.866025403784439));
#29374=DIRECTION('',(-0.5,0.,-0.866025403784439));
#29375=DIRECTION('',(0.,-1.,0.));
#29376=DIRECTION('',(-0.5,0.,-0.866025403784439));
#29377=DIRECTION('center_axis',(-1.92296268638356E-16,0.,1.));
#29378=DIRECTION('ref_axis',(-1.,0.,-1.92296268638356E-16));
#29379=DIRECTION('',(-1.,0.,-1.92296268638356E-16));
#29380=DIRECTION('',(0.,-1.,0.));
#29381=DIRECTION('',(-1.,0.,-1.92296268638356E-16));
#29382=DIRECTION('center_axis',(0.866025403784439,0.,0.5));
#29383=DIRECTION('ref_axis',(-0.5,0.,0.866025403784439));
#29384=DIRECTION('',(-0.5,0.,0.866025403784439));
#29385=DIRECTION('',(-0.5,0.,0.866025403784439));
#29386=DIRECTION('center_axis',(0.,-1.,0.));
#29387=DIRECTION('ref_axis',(0.,0.,-1.));
#29388=DIRECTION('center_axis',(0.,1.,0.));
#29389=DIRECTION('ref_axis',(0.,0.,1.));
#29390=DIRECTION('center_axis',(0.,-1.,0.));
#29391=DIRECTION('ref_axis',(1.,0.,0.));
#29392=DIRECTION('center_axis',(0.,-1.,0.));
#29393=DIRECTION('ref_axis',(1.,0.,0.));
#29394=DIRECTION('center_axis',(0.,-1.,0.));
#29395=DIRECTION('ref_axis',(1.,0.,0.));
#29396=DIRECTION('',(0.707106781186547,0.707106781186548,8.65956056235493E-17));
#29397=DIRECTION('center_axis',(0.,-1.,0.));
#29398=DIRECTION('ref_axis',(1.,0.,0.));
#29399=DIRECTION('center_axis',(0.,1.,0.));
#29400=DIRECTION('ref_axis',(1.,0.,0.));
#29401=DIRECTION('',(0.,1.,0.));
#29402=DIRECTION('center_axis',(0.,1.,0.));
#29403=DIRECTION('ref_axis',(1.,0.,0.));
#29404=DIRECTION('center_axis',(0.,-1.,0.));
#29405=DIRECTION('ref_axis',(1.,0.,0.));
#29406=DIRECTION('',(-0.707106781186547,0.707106781186548,-8.65956056235493E-17));
#29407=DIRECTION('center_axis',(0.,-1.,0.));
#29408=DIRECTION('ref_axis',(0.,0.,-1.));
#29409=DIRECTION('axis',(0.,0.,1.));
#29410=DIRECTION('refdir',(1.,0.,0.));
#29411=DIRECTION('center_axis',(0.,1.,0.));
#29412=DIRECTION('ref_axis',(1.,0.,0.));
#29413=DIRECTION('center_axis',(0.,-1.,0.));
#29414=DIRECTION('ref_axis',(1.,0.,0.));
#29415=DIRECTION('',(0.,-1.,0.));
#29416=DIRECTION('center_axis',(0.,-1.,0.));
#29417=DIRECTION('ref_axis',(1.,0.,0.));
#29418=DIRECTION('center_axis',(0.,1.,0.));
#29419=DIRECTION('ref_axis',(1.,0.,0.));
#29420=DIRECTION('center_axis',(0.,1.,0.));
#29421=DIRECTION('ref_axis',(1.,0.,0.));
#29422=DIRECTION('',(0.,-1.,0.));
#29423=DIRECTION('center_axis',(0.,1.,0.));
#29424=DIRECTION('ref_axis',(1.,0.,0.));
#29425=DIRECTION('center_axis',(0.,1.,0.));
#29426=DIRECTION('ref_axis',(1.,0.,0.));
#29427=DIRECTION('center_axis',(0.,1.,0.));
#29428=DIRECTION('ref_axis',(1.,0.,0.));
#29429=DIRECTION('axis',(0.,0.,1.));
#29430=DIRECTION('refdir',(1.,0.,0.));
#29431=DIRECTION('center_axis',(0.,1.,0.));
#29432=DIRECTION('ref_axis',(0.,0.,1.));
#29433=DIRECTION('center_axis',(0.,-1.,0.));
#29434=DIRECTION('ref_axis',(1.,0.,0.));
#29435=DIRECTION('center_axis',(0.,-1.,0.));
#29436=DIRECTION('ref_axis',(1.,0.,0.));
#29437=DIRECTION('center_axis',(0.,-1.,0.));
#29438=DIRECTION('ref_axis',(1.,0.,0.));
#29439=DIRECTION('',(0.707106781186548,0.707106781186547,8.65956056235494E-17));
#29440=DIRECTION('center_axis',(0.,-1.,0.));
#29441=DIRECTION('ref_axis',(1.,0.,0.));
#29442=DIRECTION('center_axis',(0.,-1.,0.));
#29443=DIRECTION('ref_axis',(1.,0.,0.));
#29444=DIRECTION('',(0.,1.,0.));
#29445=DIRECTION('center_axis',(0.,1.,0.));
#29446=DIRECTION('ref_axis',(1.,0.,0.));
#29447=DIRECTION('center_axis',(0.,-1.,0.));
#29448=DIRECTION('ref_axis',(1.,0.,0.));
#29449=DIRECTION('',(-0.707106781186547,0.707106781186548,-8.65956056235493E-17));
#29450=DIRECTION('center_axis',(0.,-1.,0.));
#29451=DIRECTION('ref_axis',(0.,0.,-1.));
#29452=DIRECTION('center_axis',(0.,-1.,0.));
#29453=DIRECTION('ref_axis',(1.,0.,0.));
#29454=DIRECTION('center_axis',(0.,1.,0.));
#29455=DIRECTION('ref_axis',(1.,0.,0.));
#29456=DIRECTION('center_axis',(0.,1.,0.));
#29457=DIRECTION('ref_axis',(1.,0.,0.));
#29458=DIRECTION('',(-0.447213595499958,0.894427190999916,-5.47678698264203E-17));
#29459=DIRECTION('center_axis',(0.,-1.,0.));
#29460=DIRECTION('ref_axis',(1.,0.,0.));
#29461=DIRECTION('center_axis',(0.,1.,0.));
#29462=DIRECTION('ref_axis',(1.,0.,0.));
#29463=DIRECTION('',(0.,1.,0.));
#29464=DIRECTION('center_axis',(0.,1.,0.));
#29465=DIRECTION('ref_axis',(1.,0.,0.));
#29466=DIRECTION('center_axis',(0.,-1.,0.));
#29467=DIRECTION('ref_axis',(1.,0.,0.));
#29468=DIRECTION('',(-0.707106781186547,0.707106781186548,-8.65956056235493E-17));
#29469=DIRECTION('center_axis',(0.,-1.,0.));
#29470=DIRECTION('ref_axis',(0.,0.,-1.));
#29471=DIRECTION('center_axis',(0.866025403784439,0.,-0.5));
#29472=DIRECTION('ref_axis',(0.5,0.,0.866025403784439));
#29473=DIRECTION('',(-0.5,0.,-0.866025403784439));
#29474=DIRECTION('',(0.,-1.,0.));
#29475=DIRECTION('',(0.5,0.,0.866025403784439));
#29476=DIRECTION('',(0.,-1.,0.));
#29477=DIRECTION('center_axis',(1.92296268638356E-16,0.,-1.));
#29478=DIRECTION('ref_axis',(1.,0.,1.92296268638356E-16));
#29479=DIRECTION('',(-1.,0.,-1.92296268638356E-16));
#29480=DIRECTION('',(0.,-1.,0.));
#29481=DIRECTION('',(1.,0.,1.92296268638356E-16));
#29482=DIRECTION('center_axis',(-0.866025403784439,0.,-0.5));
#29483=DIRECTION('ref_axis',(0.5,0.,-0.866025403784439));
#29484=DIRECTION('',(-0.5,0.,0.866025403784438));
#29485=DIRECTION('',(0.,-1.,0.));
#29486=DIRECTION('',(0.5,0.,-0.866025403784438));
#29487=DIRECTION('center_axis',(-0.866025403784439,0.,0.5));
#29488=DIRECTION('ref_axis',(-0.5,0.,-0.866025403784439));
#29489=DIRECTION('',(0.5,0.,0.866025403784439));
#29490=DIRECTION('',(0.,-1.,0.));
#29491=DIRECTION('',(-0.5,0.,-0.866025403784439));
#29492=DIRECTION('center_axis',(-1.92296268638356E-16,0.,1.));
#29493=DIRECTION('ref_axis',(-1.,0.,-1.92296268638356E-16));
#29494=DIRECTION('',(1.,0.,1.92296268638356E-16));
#29495=DIRECTION('',(0.,-1.,0.));
#29496=DIRECTION('',(-1.,0.,-1.92296268638356E-16));
#29497=DIRECTION('center_axis',(0.866025403784439,0.,0.5));
#29498=DIRECTION('ref_axis',(-0.5,0.,0.866025403784439));
#29499=DIRECTION('',(0.5,0.,-0.866025403784439));
#29500=DIRECTION('',(-0.5,0.,0.866025403784439));
#29501=DIRECTION('center_axis',(0.,1.,0.));
#29502=DIRECTION('ref_axis',(1.,0.,0.));
#29503=DIRECTION('center_axis',(0.,-1.,0.));
#29504=DIRECTION('ref_axis',(0.,0.,-1.));
#29505=DIRECTION('',(0.,0.,1.));
#29506=DIRECTION('',(1.,0.,0.));
#29507=DIRECTION('',(0.,0.,1.));
#29508=DIRECTION('',(1.,0.,0.));
#29509=DIRECTION('',(0.,0.,1.));
#29510=DIRECTION('',(1.,0.,0.));
#29511=DIRECTION('',(0.,0.,1.));
#29512=DIRECTION('',(1.,0.,0.));
#29513=DIRECTION('',(0.,0.,1.));
#29514=DIRECTION('',(1.,0.,0.));
#29515=DIRECTION('',(0.,0.,1.));
#29516=DIRECTION('',(1.,0.,0.));
#29517=DIRECTION('',(0.,0.,1.));
#29518=DIRECTION('',(1.,0.,0.));
#29519=DIRECTION('',(0.,0.,1.));
#29520=DIRECTION('',(1.,0.,0.));
#29521=DIRECTION('',(0.,0.,1.));
#29522=DIRECTION('',(1.,0.,0.));
#29523=DIRECTION('',(0.,0.,1.));
#29524=DIRECTION('',(1.,0.,0.));
#29525=DIRECTION('',(0.,-1.,2.22044604925031E-16));
#29526=DIRECTION('',(1.,0.,0.));
#29527=DIRECTION('',(0.,-1.,2.22044604925031E-16));
#29528=DIRECTION('',(1.,0.,0.));
#29529=DIRECTION('',(0.,-1.,2.22044604925031E-16));
#29530=DIRECTION('',(1.,0.,0.));
#29531=DIRECTION('',(0.,-1.,2.22044604925031E-16));
#29532=DIRECTION('',(1.,0.,0.));
#29533=DIRECTION('',(0.,0.,1.));
#29534=DIRECTION('',(1.,0.,0.));
#29535=DIRECTION('',(0.,-1.,2.22044604925031E-16));
#29536=DIRECTION('',(1.,0.,0.));
#29537=DIRECTION('',(0.,-1.,2.22044604925031E-16));
#29538=DIRECTION('',(1.,0.,0.));
#29539=DIRECTION('',(0.,-1.,2.22044604925031E-16));
#29540=DIRECTION('',(1.,0.,0.));
#29541=DIRECTION('',(0.,-1.,2.22044604925031E-16));
#29542=DIRECTION('',(1.,0.,0.));
#29543=DIRECTION('',(0.,1.,2.22044604925031E-16));
#29544=DIRECTION('',(1.,0.,0.));
#29545=DIRECTION('',(0.,1.,2.22044604925031E-16));
#29546=DIRECTION('',(1.,0.,0.));
#29547=DIRECTION('',(0.,0.,1.));
#29548=DIRECTION('',(2.22044604925031E-16,-1.,0.));
#29549=DIRECTION('',(0.,0.,1.));
#29550=DIRECTION('',(2.22044604925031E-16,1.,0.));
#29551=DIRECTION('',(0.,0.,1.));
#29552=DIRECTION('',(2.22044604925031E-16,1.,0.));
#29553=DIRECTION('',(0.,0.,1.));
#29554=DIRECTION('',(2.22044604925031E-16,1.,0.));
#29555=DIRECTION('',(0.,1.,2.22044604925031E-16));
#29556=DIRECTION('',(1.,0.,0.));
#29557=DIRECTION('',(0.,1.,2.22044604925031E-16));
#29558=DIRECTION('',(1.,0.,0.));
#29559=DIRECTION('',(0.,0.,1.));
#29560=DIRECTION('',(2.22044604925031E-16,-1.,0.));
#29561=DIRECTION('',(0.,0.,1.));
#29562=DIRECTION('',(2.22044604925031E-16,-1.,0.));
#29563=DIRECTION('',(0.,0.,1.));
#29564=DIRECTION('',(2.22044604925031E-16,-1.,0.));
#29565=DIRECTION('',(0.,0.,1.));
#29566=DIRECTION('',(2.22044604925031E-16,-1.,0.));
#29567=DIRECTION('',(0.,-1.,2.22044604925031E-16));
#29568=DIRECTION('',(1.,0.,0.));
#29569=DIRECTION('',(0.,-1.,2.22044604925031E-16));
#29570=DIRECTION('',(1.,0.,0.));
#29571=DIRECTION('',(0.,0.,1.));
#29572=DIRECTION('',(1.,0.,0.));
#29573=DIRECTION('',(0.,0.,1.));
#29574=DIRECTION('',(1.,0.,0.));
#29575=DIRECTION('',(0.,0.,1.));
#29576=DIRECTION('',(1.,0.,0.));
#29577=DIRECTION('',(0.,0.,1.));
#29578=DIRECTION('',(1.,0.,0.));
#29579=DIRECTION('',(0.,0.,1.));
#29580=DIRECTION('',(1.,0.,0.));
#29581=DIRECTION('',(0.,0.,1.));
#29582=DIRECTION('',(1.,0.,0.));
#29583=DIRECTION('',(0.,-1.22464679914735E-16,-1.));
#29584=DIRECTION('',(1.,0.,0.));
#29585=DIRECTION('',(0.,0.,1.));
#29586=DIRECTION('',(1.,0.,0.));
#29587=DIRECTION('',(0.,0.,1.));
#29588=DIRECTION('',(1.,0.,0.));
#29589=DIRECTION('',(0.,0.,1.));
#29590=DIRECTION('',(2.22044604925031E-16,-1.,0.));
#29591=DIRECTION('',(0.,0.,1.));
#29592=DIRECTION('',(2.22044604925031E-16,-1.,0.));
#29593=DIRECTION('',(0.,0.,1.));
#29594=DIRECTION('',(1.,0.,0.));
#29595=DIRECTION('',(0.,0.,1.));
#29596=DIRECTION('',(1.,0.,0.));
#29597=DIRECTION('',(0.,0.866025403784439,-0.5));
#29598=DIRECTION('',(1.,0.,0.));
#29599=DIRECTION('axis',(0.,0.,1.));
#29600=DIRECTION('refdir',(1.,0.,0.));
#29601=DIRECTION('axis',(0.,0.,1.));
#29602=DIRECTION('refdir',(1.,0.,0.));
#29603=DIRECTION('axis',(0.,0.,1.));
#29604=DIRECTION('refdir',(1.,0.,0.));
#29605=DIRECTION('center_axis',(0.,0.,1.));
#29606=DIRECTION('ref_axis',(1.,0.,0.));
#29607=DIRECTION('center_axis',(0.,0.,1.));
#29608=DIRECTION('ref_axis',(1.,0.,0.));
#29609=DIRECTION('',(0.,0.,1.));
#29610=DIRECTION('center_axis',(0.,0.,1.));
#29611=DIRECTION('ref_axis',(1.,0.,0.));
#29612=DIRECTION('center_axis',(0.,0.,1.));
#29613=DIRECTION('ref_axis',(1.,0.,0.));
#29614=DIRECTION('center_axis',(0.,0.,1.));
#29615=DIRECTION('ref_axis',(1.,0.,0.));
#29616=DIRECTION('center_axis',(0.,0.,1.));
#29617=DIRECTION('ref_axis',(1.,0.,0.));
#29618=DIRECTION('',(0.,0.,1.));
#29619=DIRECTION('center_axis',(0.,0.,1.));
#29620=DIRECTION('ref_axis',(1.,0.,0.));
#29621=DIRECTION('center_axis',(0.,0.,1.));
#29622=DIRECTION('ref_axis',(1.,0.,0.));
#29623=DIRECTION('center_axis',(0.,0.,1.));
#29624=DIRECTION('ref_axis',(1.,0.,0.));
#29625=DIRECTION('center_axis',(0.,0.,1.));
#29626=DIRECTION('ref_axis',(1.,0.,0.));
#29627=DIRECTION('',(0.,0.,1.));
#29628=DIRECTION('center_axis',(0.,0.,1.));
#29629=DIRECTION('ref_axis',(1.,0.,0.));
#29630=DIRECTION('center_axis',(0.,0.,1.));
#29631=DIRECTION('ref_axis',(1.,0.,0.));
#29632=DIRECTION('center_axis',(0.,0.,1.));
#29633=DIRECTION('ref_axis',(1.,0.,0.));
#29634=DIRECTION('center_axis',(0.,0.,1.));
#29635=DIRECTION('ref_axis',(1.,0.,0.));
#29636=DIRECTION('',(0.,0.,1.));
#29637=DIRECTION('center_axis',(0.,0.,1.));
#29638=DIRECTION('ref_axis',(1.,0.,0.));
#29639=DIRECTION('center_axis',(0.,0.,1.));
#29640=DIRECTION('ref_axis',(1.,0.,0.));
#29641=DIRECTION('center_axis',(0.,0.,1.));
#29642=DIRECTION('ref_axis',(1.,0.,0.));
#29643=DIRECTION('center_axis',(0.,0.,1.));
#29644=DIRECTION('ref_axis',(1.,0.,0.));
#29645=DIRECTION('',(0.,0.,1.));
#29646=DIRECTION('center_axis',(0.,0.,1.));
#29647=DIRECTION('ref_axis',(1.,0.,0.));
#29648=DIRECTION('center_axis',(0.,0.,1.));
#29649=DIRECTION('ref_axis',(1.,0.,0.));
#29650=DIRECTION('center_axis',(0.,0.,1.));
#29651=DIRECTION('ref_axis',(1.,0.,0.));
#29652=DIRECTION('center_axis',(0.,0.,1.));
#29653=DIRECTION('ref_axis',(1.,0.,0.));
#29654=DIRECTION('',(0.,0.,1.));
#29655=DIRECTION('center_axis',(0.,0.,1.));
#29656=DIRECTION('ref_axis',(1.,0.,0.));
#29657=DIRECTION('center_axis',(0.,0.,1.));
#29658=DIRECTION('ref_axis',(1.,0.,0.));
#29659=DIRECTION('center_axis',(0.,0.,1.));
#29660=DIRECTION('ref_axis',(1.,0.,0.));
#29661=DIRECTION('center_axis',(0.,0.,1.));
#29662=DIRECTION('ref_axis',(1.,0.,0.));
#29663=DIRECTION('',(0.,0.,1.));
#29664=DIRECTION('center_axis',(0.,0.,1.));
#29665=DIRECTION('ref_axis',(1.,0.,0.));
#29666=DIRECTION('center_axis',(0.,0.,1.));
#29667=DIRECTION('ref_axis',(1.,0.,0.));
#29668=DIRECTION('center_axis',(0.,0.,1.));
#29669=DIRECTION('ref_axis',(1.,0.,0.));
#29670=DIRECTION('center_axis',(0.,0.,1.));
#29671=DIRECTION('ref_axis',(1.,0.,0.));
#29672=DIRECTION('',(0.,0.,1.));
#29673=DIRECTION('center_axis',(0.,0.,1.));
#29674=DIRECTION('ref_axis',(1.,0.,0.));
#29675=DIRECTION('center_axis',(0.,0.,1.));
#29676=DIRECTION('ref_axis',(1.,0.,0.));
#29677=DIRECTION('center_axis',(0.,0.,1.));
#29678=DIRECTION('ref_axis',(1.,0.,0.));
#29679=DIRECTION('center_axis',(0.,0.,1.));
#29680=DIRECTION('ref_axis',(1.,0.,0.));
#29681=DIRECTION('',(0.,0.,1.));
#29682=DIRECTION('center_axis',(0.,0.,-1.));
#29683=DIRECTION('ref_axis',(1.,0.,0.));
#29684=DIRECTION('center_axis',(0.,0.,1.));
#29685=DIRECTION('ref_axis',(1.,0.,0.));
#29686=DIRECTION('center_axis',(0.,0.,1.));
#29687=DIRECTION('ref_axis',(1.,0.,0.));
#29688=DIRECTION('center_axis',(0.,0.,1.));
#29689=DIRECTION('ref_axis',(1.,0.,0.));
#29690=DIRECTION('center_axis',(0.,0.,1.));
#29691=DIRECTION('ref_axis',(1.,0.,0.));
#29692=DIRECTION('',(0.,0.,1.));
#29693=DIRECTION('center_axis',(0.,0.,-1.));
#29694=DIRECTION('ref_axis',(1.,0.,0.));
#29695=DIRECTION('center_axis',(0.,0.,1.));
#29696=DIRECTION('ref_axis',(1.,0.,0.));
#29697=DIRECTION('center_axis',(0.,0.,1.));
#29698=DIRECTION('ref_axis',(1.,0.,0.));
#29699=DIRECTION('center_axis',(0.,0.,1.));
#29700=DIRECTION('ref_axis',(1.,0.,0.));
#29701=DIRECTION('center_axis',(0.,0.,1.));
#29702=DIRECTION('ref_axis',(1.,0.,0.));
#29703=DIRECTION('',(0.,0.,1.));
#29704=DIRECTION('center_axis',(0.,0.,-1.));
#29705=DIRECTION('ref_axis',(1.,0.,0.));
#29706=DIRECTION('center_axis',(0.,0.,1.));
#29707=DIRECTION('ref_axis',(1.,0.,0.));
#29708=DIRECTION('center_axis',(0.,0.,1.));
#29709=DIRECTION('ref_axis',(1.,0.,0.));
#29710=DIRECTION('center_axis',(0.,0.,1.));
#29711=DIRECTION('ref_axis',(1.,0.,0.));
#29712=DIRECTION('center_axis',(0.,0.,1.));
#29713=DIRECTION('ref_axis',(1.,0.,0.));
#29714=DIRECTION('',(0.,0.,1.));
#29715=DIRECTION('center_axis',(0.,0.,-1.));
#29716=DIRECTION('ref_axis',(1.,0.,0.));
#29717=DIRECTION('center_axis',(0.,0.,1.));
#29718=DIRECTION('ref_axis',(1.,0.,0.));
#29719=DIRECTION('center_axis',(0.,0.,1.));
#29720=DIRECTION('ref_axis',(1.,0.,0.));
#29721=DIRECTION('center_axis',(0.,0.,1.));
#29722=DIRECTION('ref_axis',(1.,0.,0.));
#29723=DIRECTION('center_axis',(0.,0.,1.));
#29724=DIRECTION('ref_axis',(1.,0.,0.));
#29725=DIRECTION('',(0.,0.,1.));
#29726=DIRECTION('center_axis',(0.,0.,1.));
#29727=DIRECTION('ref_axis',(1.,0.,0.));
#29728=DIRECTION('center_axis',(0.,0.,1.));
#29729=DIRECTION('ref_axis',(1.,0.,0.));
#29730=DIRECTION('',(0.,0.,1.));
#29731=DIRECTION('center_axis',(0.,0.,1.));
#29732=DIRECTION('ref_axis',(1.,0.,0.));
#29733=DIRECTION('center_axis',(0.,0.,1.));
#29734=DIRECTION('ref_axis',(1.,0.,0.));
#29735=DIRECTION('',(0.,0.,1.));
#29736=DIRECTION('center_axis',(0.,0.,1.));
#29737=DIRECTION('ref_axis',(1.,0.,0.));
#29738=DIRECTION('center_axis',(0.,0.,1.));
#29739=DIRECTION('ref_axis',(1.,0.,0.));
#29740=DIRECTION('',(0.,0.,1.));
#29741=DIRECTION('center_axis',(0.,0.,1.));
#29742=DIRECTION('ref_axis',(1.,0.,0.));
#29743=DIRECTION('center_axis',(0.,0.,1.));
#29744=DIRECTION('ref_axis',(1.,0.,0.));
#29745=DIRECTION('',(0.,0.,1.));
#29746=DIRECTION('center_axis',(0.,0.,-1.));
#29747=DIRECTION('ref_axis',(1.,0.,0.));
#29748=DIRECTION('center_axis',(0.,0.,1.));
#29749=DIRECTION('ref_axis',(1.,0.,0.));
#29750=DIRECTION('center_axis',(0.,0.,1.));
#29751=DIRECTION('ref_axis',(1.,0.,0.));
#29752=DIRECTION('',(0.,0.,1.));
#29753=DIRECTION('center_axis',(0.,0.,-1.));
#29754=DIRECTION('ref_axis',(1.,0.,0.));
#29755=DIRECTION('center_axis',(0.,0.,1.));
#29756=DIRECTION('ref_axis',(1.,0.,0.));
#29757=DIRECTION('center_axis',(0.,0.,1.));
#29758=DIRECTION('ref_axis',(1.,0.,0.));
#29759=DIRECTION('',(0.,0.,1.));
#29760=DIRECTION('center_axis',(0.,0.,-1.));
#29761=DIRECTION('ref_axis',(1.,0.,0.));
#29762=DIRECTION('center_axis',(0.,0.,1.));
#29763=DIRECTION('ref_axis',(1.,0.,0.));
#29764=DIRECTION('center_axis',(0.,0.,1.));
#29765=DIRECTION('ref_axis',(1.,0.,0.));
#29766=DIRECTION('',(0.,0.,1.));
#29767=DIRECTION('center_axis',(0.,0.,-1.));
#29768=DIRECTION('ref_axis',(1.,0.,0.));
#29769=DIRECTION('center_axis',(0.,0.,1.));
#29770=DIRECTION('ref_axis',(1.,0.,0.));
#29771=DIRECTION('center_axis',(0.,0.,1.));
#29772=DIRECTION('ref_axis',(1.,0.,0.));
#29773=DIRECTION('',(0.,0.,1.));
#29774=DIRECTION('center_axis',(0.,0.,-1.));
#29775=DIRECTION('ref_axis',(1.,0.,0.));
#29776=DIRECTION('center_axis',(0.,0.,1.));
#29777=DIRECTION('ref_axis',(1.,0.,0.));
#29778=DIRECTION('center_axis',(0.,0.,1.));
#29779=DIRECTION('ref_axis',(1.,0.,0.));
#29780=DIRECTION('',(0.,0.,1.));
#29781=DIRECTION('center_axis',(0.,0.,-1.));
#29782=DIRECTION('ref_axis',(1.,0.,0.));
#29783=DIRECTION('center_axis',(0.,0.,1.));
#29784=DIRECTION('ref_axis',(1.,0.,0.));
#29785=DIRECTION('center_axis',(0.,0.,1.));
#29786=DIRECTION('ref_axis',(1.,0.,0.));
#29787=DIRECTION('',(0.,0.,1.));
#29788=DIRECTION('center_axis',(0.,0.,-1.));
#29789=DIRECTION('ref_axis',(1.,0.,0.));
#29790=DIRECTION('center_axis',(0.,0.,1.));
#29791=DIRECTION('ref_axis',(1.,0.,0.));
#29792=DIRECTION('center_axis',(0.,0.,1.));
#29793=DIRECTION('ref_axis',(1.,0.,0.));
#29794=DIRECTION('',(0.,0.,1.));
#29795=DIRECTION('center_axis',(0.,0.,-1.));
#29796=DIRECTION('ref_axis',(1.,0.,0.));
#29797=DIRECTION('center_axis',(0.,0.,1.));
#29798=DIRECTION('ref_axis',(1.,0.,0.));
#29799=DIRECTION('center_axis',(0.,0.,1.));
#29800=DIRECTION('ref_axis',(1.,0.,0.));
#29801=DIRECTION('',(0.,0.,1.));
#29802=DIRECTION('center_axis',(0.,0.,-1.));
#29803=DIRECTION('ref_axis',(1.,0.,0.));
#29804=DIRECTION('center_axis',(0.,0.,1.));
#29805=DIRECTION('ref_axis',(1.,0.,0.));
#29806=DIRECTION('center_axis',(0.,0.,1.));
#29807=DIRECTION('ref_axis',(1.,0.,0.));
#29808=DIRECTION('',(0.,0.,1.));
#29809=DIRECTION('center_axis',(0.,0.,-1.));
#29810=DIRECTION('ref_axis',(1.,0.,0.));
#29811=DIRECTION('center_axis',(0.,1.,0.));
#29812=DIRECTION('ref_axis',(-1.,0.,0.));
#29813=DIRECTION('',(-1.,0.,0.));
#29814=DIRECTION('',(0.,0.,1.));
#29815=DIRECTION('',(-1.,0.,0.));
#29816=DIRECTION('',(0.,0.,1.));
#29817=DIRECTION('center_axis',(1.,0.,0.));
#29818=DIRECTION('ref_axis',(0.,1.,0.));
#29819=DIRECTION('',(0.,1.,0.));
#29820=DIRECTION('',(0.,1.,0.));
#29821=DIRECTION('',(0.,0.,1.));
#29822=DIRECTION('center_axis',(0.,-1.,0.));
#29823=DIRECTION('ref_axis',(1.,0.,0.));
#29824=DIRECTION('',(1.,0.,0.));
#29825=DIRECTION('',(1.,0.,0.));
#29826=DIRECTION('',(0.,0.,1.));
#29827=DIRECTION('center_axis',(-1.,0.,0.));
#29828=DIRECTION('ref_axis',(0.,-1.,0.));
#29829=DIRECTION('',(0.,-1.,0.));
#29830=DIRECTION('',(0.,-1.,0.));
#29831=DIRECTION('center_axis',(0.,0.,1.));
#29832=DIRECTION('ref_axis',(1.,0.,0.));
#29833=DIRECTION('center_axis',(0.,0.,1.));
#29834=DIRECTION('ref_axis',(1.,0.,0.));
#29835=DIRECTION('axis',(0.,0.,1.));
#29836=DIRECTION('refdir',(1.,0.,0.));
#29837=DIRECTION('center_axis',(0.,0.,1.));
#29838=DIRECTION('ref_axis',(1.,0.,0.));
#29839=DIRECTION('',(0.,0.,1.));
#29840=DIRECTION('center_axis',(0.,0.,1.));
#29841=DIRECTION('ref_axis',(1.,0.,0.));
#29842=DIRECTION('',(0.,0.,1.));
#29843=DIRECTION('center_axis',(0.,0.,-1.));
#29844=DIRECTION('ref_axis',(1.,0.,0.));
#29845=DIRECTION('center_axis',(0.,0.,1.));
#29846=DIRECTION('ref_axis',(1.,0.,0.));
#29847=DIRECTION('',(0.,0.,1.));
#29848=DIRECTION('center_axis',(0.,0.,1.));
#29849=DIRECTION('ref_axis',(1.,0.,0.));
#29850=DIRECTION('',(0.,0.,1.));
#29851=DIRECTION('center_axis',(0.,0.,-1.));
#29852=DIRECTION('ref_axis',(1.,0.,0.));
#29853=DIRECTION('center_axis',(0.,0.,1.));
#29854=DIRECTION('ref_axis',(1.,0.,0.));
#29855=DIRECTION('center_axis',(0.,0.,1.));
#29856=DIRECTION('ref_axis',(1.,0.,0.));
#29857=DIRECTION('',(0.,0.,1.));
#29858=DIRECTION('center_axis',(0.,0.,-1.));
#29859=DIRECTION('ref_axis',(1.,0.,0.));
#29860=DIRECTION('center_axis',(0.,0.,1.));
#29861=DIRECTION('ref_axis',(1.,0.,0.));
#29862=DIRECTION('center_axis',(0.,0.,1.));
#29863=DIRECTION('ref_axis',(1.,0.,0.));
#29864=DIRECTION('',(0.,0.,1.));
#29865=DIRECTION('center_axis',(0.,0.,-1.));
#29866=DIRECTION('ref_axis',(1.,0.,0.));
#29867=DIRECTION('center_axis',(0.,0.,1.));
#29868=DIRECTION('ref_axis',(1.,0.,0.));
#29869=DIRECTION('center_axis',(0.,0.,1.));
#29870=DIRECTION('ref_axis',(1.,0.,0.));
#29871=DIRECTION('',(0.,0.,1.));
#29872=DIRECTION('center_axis',(0.,0.,-1.));
#29873=DIRECTION('ref_axis',(1.,0.,0.));
#29874=DIRECTION('center_axis',(0.,0.,1.));
#29875=DIRECTION('ref_axis',(1.,0.,0.));
#29876=DIRECTION('center_axis',(0.,0.,1.));
#29877=DIRECTION('ref_axis',(1.,0.,0.));
#29878=DIRECTION('',(0.,0.,1.));
#29879=DIRECTION('center_axis',(0.,0.,-1.));
#29880=DIRECTION('ref_axis',(1.,0.,0.));
#29881=DIRECTION('center_axis',(0.,0.,1.));
#29882=DIRECTION('ref_axis',(1.,0.,0.));
#29883=DIRECTION('center_axis',(0.,0.,1.));
#29884=DIRECTION('ref_axis',(1.,0.,0.));
#29885=DIRECTION('',(0.,0.,1.));
#29886=DIRECTION('center_axis',(0.,0.,-1.));
#29887=DIRECTION('ref_axis',(1.,0.,0.));
#29888=DIRECTION('center_axis',(0.,0.,1.));
#29889=DIRECTION('ref_axis',(1.,0.,0.));
#29890=DIRECTION('center_axis',(0.,0.,1.));
#29891=DIRECTION('ref_axis',(1.,0.,0.));
#29892=DIRECTION('center_axis',(0.,0.,1.));
#29893=DIRECTION('ref_axis',(1.,0.,0.));
#29894=DIRECTION('center_axis',(0.,0.,-1.));
#29895=DIRECTION('ref_axis',(1.,0.,0.));
#29896=DIRECTION('',(0.,0.,1.));
#29897=DIRECTION('center_axis',(0.,0.,1.));
#29898=DIRECTION('ref_axis',(1.,0.,0.));
#29899=DIRECTION('center_axis',(0.,0.,1.));
#29900=DIRECTION('ref_axis',(1.,0.,0.));
#29901=DIRECTION('center_axis',(0.,0.,1.));
#29902=DIRECTION('ref_axis',(1.,0.,0.));
#29903=DIRECTION('center_axis',(0.,0.,1.));
#29904=DIRECTION('ref_axis',(1.,0.,0.));
#29905=DIRECTION('center_axis',(0.,0.,1.));
#29906=DIRECTION('ref_axis',(1.,0.,0.));
#29907=DIRECTION('',(0.,0.,1.));
#29908=DIRECTION('center_axis',(0.,0.,-1.));
#29909=DIRECTION('ref_axis',(1.,0.,0.));
#29910=DIRECTION('center_axis',(0.,0.,1.));
#29911=DIRECTION('ref_axis',(1.,0.,0.));
#29912=DIRECTION('center_axis',(0.,0.,1.));
#29913=DIRECTION('ref_axis',(1.,0.,0.));
#29914=DIRECTION('center_axis',(0.,0.,1.));
#29915=DIRECTION('ref_axis',(1.,0.,0.));
#29916=DIRECTION('center_axis',(0.,0.,-1.));
#29917=DIRECTION('ref_axis',(1.,0.,0.));
#29918=DIRECTION('',(0.,0.,1.));
#29919=DIRECTION('center_axis',(0.,0.,1.));
#29920=DIRECTION('ref_axis',(1.,0.,0.));
#29921=DIRECTION('center_axis',(0.,0.,1.));
#29922=DIRECTION('ref_axis',(1.,0.,0.));
#29923=DIRECTION('center_axis',(0.,0.,1.));
#29924=DIRECTION('ref_axis',(1.,0.,0.));
#29925=DIRECTION('center_axis',(0.,0.,1.));
#29926=DIRECTION('ref_axis',(1.,0.,0.));
#29927=DIRECTION('',(0.,-1.,0.));
#29928=DIRECTION('',(1.,0.,0.));
#29929=DIRECTION('',(0.,1.,0.));
#29930=DIRECTION('',(-1.,0.,0.));
#29931=DIRECTION('',(-1.,0.,0.));
#29932=DIRECTION('',(-1.,0.,0.));
#29933=DIRECTION('center_axis',(0.,0.,1.));
#29934=DIRECTION('ref_axis',(1.,0.,0.));
#29935=DIRECTION('center_axis',(0.,0.,1.));
#29936=DIRECTION('ref_axis',(1.,0.,0.));
#29937=DIRECTION('',(0.,0.,1.));
#29938=DIRECTION('center_axis',(0.,0.,1.));
#29939=DIRECTION('ref_axis',(1.,0.,0.));
#29940=DIRECTION('center_axis',(0.,0.,1.));
#29941=DIRECTION('ref_axis',(1.,0.,0.));
#29942=DIRECTION('',(0.,0.,1.));
#29943=DIRECTION('center_axis',(0.,0.,1.));
#29944=DIRECTION('ref_axis',(1.,0.,0.));
#29945=DIRECTION('center_axis',(0.,0.,1.));
#29946=DIRECTION('ref_axis',(1.,0.,0.));
#29947=DIRECTION('',(0.,0.,1.));
#29948=DIRECTION('center_axis',(0.,0.,1.));
#29949=DIRECTION('ref_axis',(1.,0.,0.));
#29950=DIRECTION('center_axis',(0.,0.,1.));
#29951=DIRECTION('ref_axis',(1.,0.,0.));
#29952=DIRECTION('',(0.,0.,1.));
#29953=DIRECTION('center_axis',(0.,1.,0.));
#29954=DIRECTION('ref_axis',(-1.,0.,0.));
#29955=DIRECTION('',(-1.,0.,0.));
#29956=DIRECTION('',(0.,0.,1.));
#29957=DIRECTION('',(0.,0.,1.));
#29958=DIRECTION('center_axis',(1.,0.,0.));
#29959=DIRECTION('ref_axis',(0.,1.,0.));
#29960=DIRECTION('',(0.,1.,0.));
#29961=DIRECTION('',(0.,0.,1.));
#29962=DIRECTION('center_axis',(0.,-1.,0.));
#29963=DIRECTION('ref_axis',(1.,0.,0.));
#29964=DIRECTION('',(1.,0.,0.));
#29965=DIRECTION('',(0.,0.,1.));
#29966=DIRECTION('center_axis',(-1.,0.,0.));
#29967=DIRECTION('ref_axis',(0.,-1.,0.));
#29968=DIRECTION('',(0.,-1.,0.));
#29969=DIRECTION('center_axis',(0.,0.,1.));
#29970=DIRECTION('ref_axis',(1.,0.,0.));
#29971=DIRECTION('axis',(0.,0.,1.));
#29972=DIRECTION('refdir',(1.,0.,0.));
#29973=DIRECTION('center_axis',(1.,0.,0.));
#29974=DIRECTION('ref_axis',(0.,0.,-1.));
#29975=DIRECTION('center_axis',(1.,0.,0.));
#29976=DIRECTION('ref_axis',(0.,0.,-1.));
#29977=DIRECTION('',(1.,0.,0.));
#29978=DIRECTION('center_axis',(-1.,0.,0.));
#29979=DIRECTION('ref_axis',(0.,0.,-1.));
#29980=DIRECTION('center_axis',(1.,0.,0.));
#29981=DIRECTION('ref_axis',(0.,0.,-1.));
#29982=DIRECTION('center_axis',(1.,0.,0.));
#29983=DIRECTION('ref_axis',(0.,0.,-1.));
#29984=DIRECTION('',(1.,0.,0.));
#29985=DIRECTION('center_axis',(-1.,0.,0.));
#29986=DIRECTION('ref_axis',(0.,0.,-1.));
#29987=DIRECTION('center_axis',(1.,0.,0.));
#29988=DIRECTION('ref_axis',(0.,0.,-1.));
#29989=DIRECTION('center_axis',(1.,0.,0.));
#29990=DIRECTION('ref_axis',(0.,0.,-1.));
#29991=DIRECTION('',(1.,0.,0.));
#29992=DIRECTION('center_axis',(-1.,0.,0.));
#29993=DIRECTION('ref_axis',(0.,0.,-1.));
#29994=DIRECTION('center_axis',(1.,0.,0.));
#29995=DIRECTION('ref_axis',(0.,0.,-1.));
#29996=DIRECTION('center_axis',(1.,0.,0.));
#29997=DIRECTION('ref_axis',(0.,0.,-1.));
#29998=DIRECTION('',(1.,0.,0.));
#29999=DIRECTION('center_axis',(1.,0.,0.));
#30000=DIRECTION('ref_axis',(0.,0.,-1.));
#30001=DIRECTION('center_axis',(1.,0.,0.));
#30002=DIRECTION('ref_axis',(0.,0.,-1.));
#30003=DIRECTION('center_axis',(-1.,0.,0.));
#30004=DIRECTION('ref_axis',(0.,0.,-1.));
#30005=DIRECTION('center_axis',(1.,0.,0.));
#30006=DIRECTION('ref_axis',(0.,0.,-1.));
#30007=DIRECTION('',(1.,0.,0.));
#30008=DIRECTION('center_axis',(-1.,0.,0.));
#30009=DIRECTION('ref_axis',(0.,0.,-1.));
#30010=DIRECTION('center_axis',(0.,0.,1.));
#30011=DIRECTION('ref_axis',(1.,0.,0.));
#30012=DIRECTION('center_axis',(0.,0.,1.));
#30013=DIRECTION('ref_axis',(1.,0.,0.));
#30014=DIRECTION('',(0.,0.,1.));
#30015=DIRECTION('center_axis',(0.,0.,1.));
#30016=DIRECTION('ref_axis',(1.,0.,0.));
#30017=DIRECTION('center_axis',(0.,0.,1.));
#30018=DIRECTION('ref_axis',(1.,0.,0.));
#30019=DIRECTION('center_axis',(0.,0.,1.));
#30020=DIRECTION('ref_axis',(1.,0.,0.));
#30021=DIRECTION('center_axis',(0.,0.,1.));
#30022=DIRECTION('ref_axis',(1.,0.,0.));
#30023=DIRECTION('',(0.,0.,1.));
#30024=DIRECTION('center_axis',(0.,0.,1.));
#30025=DIRECTION('ref_axis',(1.,0.,0.));
#30026=DIRECTION('center_axis',(0.,0.,1.));
#30027=DIRECTION('ref_axis',(1.,0.,0.));
#30028=DIRECTION('center_axis',(0.,1.,0.));
#30029=DIRECTION('ref_axis',(-1.,0.,0.));
#30030=DIRECTION('',(-1.,0.,0.));
#30031=DIRECTION('',(0.,0.,1.));
#30032=DIRECTION('',(-1.,0.,0.));
#30033=DIRECTION('',(0.,0.,1.));
#30034=DIRECTION('center_axis',(1.,0.,0.));
#30035=DIRECTION('ref_axis',(0.,1.,0.));
#30036=DIRECTION('',(0.,1.,0.));
#30037=DIRECTION('',(0.,1.,0.));
#30038=DIRECTION('',(0.,0.,1.));
#30039=DIRECTION('center_axis',(0.,-1.,0.));
#30040=DIRECTION('ref_axis',(1.,0.,0.));
#30041=DIRECTION('',(1.,0.,0.));
#30042=DIRECTION('',(1.,0.,0.));
#30043=DIRECTION('',(0.,0.,1.));
#30044=DIRECTION('center_axis',(-1.,0.,0.));
#30045=DIRECTION('ref_axis',(0.,-1.,0.));
#30046=DIRECTION('',(0.,-1.,0.));
#30047=DIRECTION('',(0.,-1.,0.));
#30048=DIRECTION('center_axis',(0.,0.,1.));
#30049=DIRECTION('ref_axis',(1.,0.,0.));
#30050=DIRECTION('center_axis',(0.,0.,1.));
#30051=DIRECTION('ref_axis',(1.,0.,0.));
#30052=DIRECTION('axis',(0.,0.,1.));
#30053=DIRECTION('refdir',(1.,0.,0.));
#30054=DIRECTION('center_axis',(1.,0.,0.));
#30055=DIRECTION('ref_axis',(0.,0.,-1.));
#30056=DIRECTION('center_axis',(1.,0.,0.));
#30057=DIRECTION('ref_axis',(0.,0.,-1.));
#30058=DIRECTION('',(1.,0.,0.));
#30059=DIRECTION('center_axis',(-1.,0.,0.));
#30060=DIRECTION('ref_axis',(0.,0.,-1.));
#30061=DIRECTION('center_axis',(1.,0.,0.));
#30062=DIRECTION('ref_axis',(0.,0.,-1.));
#30063=DIRECTION('center_axis',(1.,0.,0.));
#30064=DIRECTION('ref_axis',(0.,0.,-1.));
#30065=DIRECTION('',(1.,0.,0.));
#30066=DIRECTION('center_axis',(-1.,0.,0.));
#30067=DIRECTION('ref_axis',(0.,0.,-1.));
#30068=DIRECTION('center_axis',(1.,0.,0.));
#30069=DIRECTION('ref_axis',(0.,0.,-1.));
#30070=DIRECTION('center_axis',(1.,0.,0.));
#30071=DIRECTION('ref_axis',(0.,0.,-1.));
#30072=DIRECTION('',(1.,0.,0.));
#30073=DIRECTION('center_axis',(-1.,0.,0.));
#30074=DIRECTION('ref_axis',(0.,0.,-1.));
#30075=DIRECTION('center_axis',(1.,0.,0.));
#30076=DIRECTION('ref_axis',(0.,0.,-1.));
#30077=DIRECTION('center_axis',(1.,0.,0.));
#30078=DIRECTION('ref_axis',(0.,0.,-1.));
#30079=DIRECTION('',(-1.,0.,0.));
#30080=DIRECTION('center_axis',(-1.,0.,0.));
#30081=DIRECTION('ref_axis',(0.,0.,-1.));
#30082=DIRECTION('center_axis',(1.,0.,0.));
#30083=DIRECTION('ref_axis',(0.,0.,-1.));
#30084=DIRECTION('center_axis',(-1.,0.,0.));
#30085=DIRECTION('ref_axis',(0.,0.,-1.));
#30086=DIRECTION('center_axis',(1.,0.,0.));
#30087=DIRECTION('ref_axis',(0.,0.,-1.));
#30088=DIRECTION('',(-1.,0.,0.));
#30089=DIRECTION('center_axis',(-1.,0.,0.));
#30090=DIRECTION('ref_axis',(0.,0.,-1.));
#30091=DIRECTION('center_axis',(1.,0.,0.));
#30092=DIRECTION('ref_axis',(0.,0.,-1.));
#30093=DIRECTION('center_axis',(1.,0.,0.));
#30094=DIRECTION('ref_axis',(0.,0.,-1.));
#30095=DIRECTION('',(-1.,0.,0.));
#30096=DIRECTION('center_axis',(1.,0.,0.));
#30097=DIRECTION('ref_axis',(0.,0.,-1.));
#30098=DIRECTION('center_axis',(1.,0.,0.));
#30099=DIRECTION('ref_axis',(0.,0.,-1.));
#30100=DIRECTION('center_axis',(1.,0.,0.));
#30101=DIRECTION('ref_axis',(0.,0.,-1.));
#30102=DIRECTION('axis',(0.,0.,1.));
#30103=DIRECTION('refdir',(1.,0.,0.));
#30104=DIRECTION('center_axis',(1.,0.,0.));
#30105=DIRECTION('ref_axis',(0.,0.,-1.));
#30106=DIRECTION('center_axis',(1.,0.,0.));
#30107=DIRECTION('ref_axis',(0.,0.,-1.));
#30108=DIRECTION('',(1.,0.,0.));
#30109=DIRECTION('center_axis',(-1.,0.,0.));
#30110=DIRECTION('ref_axis',(0.,0.,-1.));
#30111=DIRECTION('center_axis',(1.,0.,0.));
#30112=DIRECTION('ref_axis',(0.,0.,-1.));
#30113=DIRECTION('center_axis',(1.,0.,0.));
#30114=DIRECTION('ref_axis',(0.,0.,-1.));
#30115=DIRECTION('',(1.,0.,0.));
#30116=DIRECTION('center_axis',(-1.,0.,0.));
#30117=DIRECTION('ref_axis',(0.,0.,-1.));
#30118=DIRECTION('center_axis',(1.,0.,0.));
#30119=DIRECTION('ref_axis',(0.,0.,-1.));
#30120=DIRECTION('center_axis',(1.,0.,0.));
#30121=DIRECTION('ref_axis',(0.,0.,-1.));
#30122=DIRECTION('',(1.,0.,0.));
#30123=DIRECTION('center_axis',(-1.,0.,0.));
#30124=DIRECTION('ref_axis',(0.,0.,-1.));
#30125=DIRECTION('center_axis',(1.,0.,0.));
#30126=DIRECTION('ref_axis',(0.,0.,-1.));
#30127=DIRECTION('center_axis',(1.,0.,0.));
#30128=DIRECTION('ref_axis',(0.,0.,-1.));
#30129=DIRECTION('',(1.,0.,0.));
#30130=DIRECTION('center_axis',(-1.,0.,0.));
#30131=DIRECTION('ref_axis',(0.,0.,-1.));
#30132=DIRECTION('center_axis',(1.,0.,0.));
#30133=DIRECTION('ref_axis',(0.,0.,-1.));
#30134=DIRECTION('center_axis',(1.,0.,0.));
#30135=DIRECTION('ref_axis',(0.,0.,-1.));
#30136=DIRECTION('center_axis',(1.,0.,0.));
#30137=DIRECTION('ref_axis',(0.,0.,-1.));
#30138=DIRECTION('center_axis',(1.,0.,0.));
#30139=DIRECTION('ref_axis',(0.,0.,-1.));
#30140=DIRECTION('',(1.,0.,0.));
#30141=DIRECTION('center_axis',(0.,0.,1.));
#30142=DIRECTION('ref_axis',(1.,0.,0.));
#30143=DIRECTION('center_axis',(0.,0.,1.));
#30144=DIRECTION('ref_axis',(1.,0.,0.));
#30145=DIRECTION('',(0.,0.,1.));
#30146=DIRECTION('center_axis',(0.,0.,1.));
#30147=DIRECTION('ref_axis',(1.,0.,0.));
#30148=DIRECTION('center_axis',(0.,0.,1.));
#30149=DIRECTION('ref_axis',(1.,0.,0.));
#30150=DIRECTION('center_axis',(0.,0.,1.));
#30151=DIRECTION('ref_axis',(1.,0.,0.));
#30152=DIRECTION('center_axis',(0.,0.,1.));
#30153=DIRECTION('ref_axis',(1.,0.,0.));
#30154=DIRECTION('',(0.,0.,1.));
#30155=DIRECTION('center_axis',(0.,0.,1.));
#30156=DIRECTION('ref_axis',(1.,0.,0.));
#30157=DIRECTION('center_axis',(0.,0.,1.));
#30158=DIRECTION('ref_axis',(1.,0.,0.));
#30159=DIRECTION('center_axis',(0.,1.,0.));
#30160=DIRECTION('ref_axis',(-1.,0.,0.));
#30161=DIRECTION('',(-1.,0.,0.));
#30162=DIRECTION('',(0.,0.,1.));
#30163=DIRECTION('',(-1.,0.,0.));
#30164=DIRECTION('',(0.,0.,1.));
#30165=DIRECTION('center_axis',(1.,0.,0.));
#30166=DIRECTION('ref_axis',(0.,1.,0.));
#30167=DIRECTION('',(0.,1.,0.));
#30168=DIRECTION('',(0.,1.,0.));
#30169=DIRECTION('',(0.,0.,1.));
#30170=DIRECTION('center_axis',(0.,-1.,0.));
#30171=DIRECTION('ref_axis',(1.,0.,0.));
#30172=DIRECTION('',(1.,0.,0.));
#30173=DIRECTION('',(1.,0.,0.));
#30174=DIRECTION('',(0.,0.,1.));
#30175=DIRECTION('center_axis',(-1.,0.,0.));
#30176=DIRECTION('ref_axis',(0.,-1.,0.));
#30177=DIRECTION('',(0.,-1.,0.));
#30178=DIRECTION('',(0.,-1.,0.));
#30179=DIRECTION('center_axis',(0.,0.,1.));
#30180=DIRECTION('ref_axis',(1.,0.,0.));
#30181=DIRECTION('center_axis',(0.,0.,1.));
#30182=DIRECTION('ref_axis',(1.,0.,0.));
#30183=DIRECTION('axis',(0.,0.,1.));
#30184=DIRECTION('refdir',(1.,0.,0.));
#30185=DIRECTION('center_axis',(1.,0.,0.));
#30186=DIRECTION('ref_axis',(0.,0.,-1.));
#30187=DIRECTION('center_axis',(1.,0.,0.));
#30188=DIRECTION('ref_axis',(0.,0.,-1.));
#30189=DIRECTION('',(1.,0.,0.));
#30190=DIRECTION('center_axis',(-1.,0.,0.));
#30191=DIRECTION('ref_axis',(0.,0.,-1.));
#30192=DIRECTION('center_axis',(1.,0.,0.));
#30193=DIRECTION('ref_axis',(0.,0.,-1.));
#30194=DIRECTION('center_axis',(1.,0.,0.));
#30195=DIRECTION('ref_axis',(0.,0.,-1.));
#30196=DIRECTION('',(1.,0.,0.));
#30197=DIRECTION('center_axis',(-1.,0.,0.));
#30198=DIRECTION('ref_axis',(0.,0.,-1.));
#30199=DIRECTION('center_axis',(1.,0.,0.));
#30200=DIRECTION('ref_axis',(0.,0.,-1.));
#30201=DIRECTION('center_axis',(1.,0.,0.));
#30202=DIRECTION('ref_axis',(0.,0.,-1.));
#30203=DIRECTION('',(1.,0.,0.));
#30204=DIRECTION('center_axis',(-1.,0.,0.));
#30205=DIRECTION('ref_axis',(0.,0.,-1.));
#30206=DIRECTION('center_axis',(0.,0.,1.));
#30207=DIRECTION('ref_axis',(0.,-1.,0.));
#30208=DIRECTION('',(1.,0.,0.));
#30209=DIRECTION('',(0.,-1.,0.));
#30210=DIRECTION('',(-1.,0.,0.));
#30211=DIRECTION('',(0.,1.,0.));
#30212=DIRECTION('center_axis',(1.,0.,0.));
#30213=DIRECTION('ref_axis',(0.,0.,-1.));
#30214=DIRECTION('center_axis',(1.,0.,0.));
#30215=DIRECTION('ref_axis',(0.,0.,-1.));
#30216=DIRECTION('center_axis',(1.,0.,0.));
#30217=DIRECTION('ref_axis',(0.,0.,-1.));
#30218=DIRECTION('center_axis',(1.,0.,0.));
#30219=DIRECTION('ref_axis',(0.,1.22464679914735E-16,1.));
#30220=DIRECTION('center_axis',(1.,0.,0.));
#30221=DIRECTION('ref_axis',(0.,0.,-1.));
#30222=DIRECTION('center_axis',(1.,0.,0.));
#30223=DIRECTION('ref_axis',(0.,0.,-1.));
#30224=DIRECTION('',(-1.,0.,0.));
#30225=DIRECTION('center_axis',(1.,0.,0.));
#30226=DIRECTION('ref_axis',(0.,0.,-1.));
#30227=DIRECTION('center_axis',(1.,0.,0.));
#30228=DIRECTION('ref_axis',(0.,0.,-1.));
#30229=DIRECTION('center_axis',(-1.,0.,0.));
#30230=DIRECTION('ref_axis',(0.,0.,-1.));
#30231=DIRECTION('center_axis',(1.,0.,0.));
#30232=DIRECTION('ref_axis',(0.,0.,-1.));
#30233=DIRECTION('center_axis',(-1.,0.,0.));
#30234=DIRECTION('ref_axis',(0.,0.,-1.));
#30235=DIRECTION('',(-1.,0.,0.));
#30236=DIRECTION('center_axis',(1.,0.,0.));
#30237=DIRECTION('ref_axis',(0.,0.,-1.));
#30238=DIRECTION('axis',(0.,0.,1.));
#30239=DIRECTION('refdir',(1.,0.,0.));
#30240=DIRECTION('center_axis',(0.,0.,1.));
#30241=DIRECTION('ref_axis',(1.,0.,0.));
#30242=DIRECTION('center_axis',(0.,0.,1.));
#30243=DIRECTION('ref_axis',(1.,0.,0.));
#30244=DIRECTION('',(0.,0.,1.));
#30245=DIRECTION('center_axis',(0.,0.,-1.));
#30246=DIRECTION('ref_axis',(1.,0.,0.));
#30247=DIRECTION('center_axis',(0.,0.,1.));
#30248=DIRECTION('ref_axis',(1.,0.,0.));
#30249=DIRECTION('center_axis',(0.,0.,1.));
#30250=DIRECTION('ref_axis',(1.,0.,0.));
#30251=DIRECTION('center_axis',(0.,0.,1.));
#30252=DIRECTION('ref_axis',(1.,0.,0.));
#30253=DIRECTION('center_axis',(0.,0.,1.));
#30254=DIRECTION('ref_axis',(1.,0.,0.));
#30255=DIRECTION('',(0.,0.,1.));
#30256=DIRECTION('center_axis',(0.,1.,0.));
#30257=DIRECTION('ref_axis',(-1.,0.,0.));
#30258=DIRECTION('',(-1.,0.,0.));
#30259=DIRECTION('',(0.,0.,1.));
#30260=DIRECTION('',(-1.,0.,0.));
#30261=DIRECTION('',(0.,0.,1.));
#30262=DIRECTION('center_axis',(1.,0.,0.));
#30263=DIRECTION('ref_axis',(0.,1.,0.));
#30264=DIRECTION('',(0.,1.,0.));
#30265=DIRECTION('',(0.,1.,0.));
#30266=DIRECTION('',(0.,0.,1.));
#30267=DIRECTION('center_axis',(0.,-1.,0.));
#30268=DIRECTION('ref_axis',(1.,0.,0.));
#30269=DIRECTION('',(1.,0.,0.));
#30270=DIRECTION('',(1.,0.,0.));
#30271=DIRECTION('',(0.,0.,1.));
#30272=DIRECTION('center_axis',(-1.,0.,0.));
#30273=DIRECTION('ref_axis',(0.,-1.,0.));
#30274=DIRECTION('',(0.,-1.,0.));
#30275=DIRECTION('',(0.,-1.,0.));
#30276=DIRECTION('center_axis',(0.,0.,1.));
#30277=DIRECTION('ref_axis',(1.,0.,0.));
#30278=DIRECTION('center_axis',(0.,0.,1.));
#30279=DIRECTION('ref_axis',(1.,0.,0.));
#30280=DIRECTION('axis',(0.,0.,1.));
#30281=DIRECTION('refdir',(1.,0.,0.));
#30282=DIRECTION('center_axis',(0.,0.,1.));
#30283=DIRECTION('ref_axis',(1.,0.,0.));
#30284=DIRECTION('center_axis',(0.,0.,1.));
#30285=DIRECTION('ref_axis',(1.,0.,0.));
#30286=DIRECTION('',(0.,0.,1.));
#30287=DIRECTION('center_axis',(0.,0.,-1.));
#30288=DIRECTION('ref_axis',(1.,0.,0.));
#30289=DIRECTION('center_axis',(0.,0.,1.));
#30290=DIRECTION('ref_axis',(1.,0.,0.));
#30291=DIRECTION('center_axis',(0.,0.,1.));
#30292=DIRECTION('ref_axis',(1.,0.,0.));
#30293=DIRECTION('center_axis',(0.,0.,1.));
#30294=DIRECTION('ref_axis',(1.,0.,0.));
#30295=DIRECTION('center_axis',(0.,0.,1.));
#30296=DIRECTION('ref_axis',(1.,0.,0.));
#30297=DIRECTION('',(0.,0.,1.));
#30298=DIRECTION('center_axis',(0.,1.,0.));
#30299=DIRECTION('ref_axis',(-1.,0.,0.));
#30300=DIRECTION('',(-1.,0.,0.));
#30301=DIRECTION('',(0.,0.,1.));
#30302=DIRECTION('',(-1.,0.,0.));
#30303=DIRECTION('',(0.,0.,1.));
#30304=DIRECTION('center_axis',(1.,0.,0.));
#30305=DIRECTION('ref_axis',(0.,1.,0.));
#30306=DIRECTION('',(0.,1.,0.));
#30307=DIRECTION('',(0.,1.,0.));
#30308=DIRECTION('',(0.,0.,1.));
#30309=DIRECTION('center_axis',(0.,-1.,0.));
#30310=DIRECTION('ref_axis',(1.,0.,0.));
#30311=DIRECTION('',(1.,0.,0.));
#30312=DIRECTION('',(1.,0.,0.));
#30313=DIRECTION('',(0.,0.,1.));
#30314=DIRECTION('center_axis',(-1.,0.,0.));
#30315=DIRECTION('ref_axis',(0.,-1.,0.));
#30316=DIRECTION('',(0.,-1.,0.));
#30317=DIRECTION('',(0.,-1.,0.));
#30318=DIRECTION('center_axis',(0.,0.,1.));
#30319=DIRECTION('ref_axis',(1.,0.,0.));
#30320=DIRECTION('center_axis',(0.,0.,1.));
#30321=DIRECTION('ref_axis',(1.,0.,0.));
#30322=DIRECTION('axis',(0.,0.,1.));
#30323=DIRECTION('refdir',(1.,0.,0.));
#30324=DIRECTION('center_axis',(0.,0.,1.));
#30325=DIRECTION('ref_axis',(1.,0.,0.));
#30326=DIRECTION('center_axis',(0.,0.,1.));
#30327=DIRECTION('ref_axis',(1.,0.,0.));
#30328=DIRECTION('',(0.,0.,1.));
#30329=DIRECTION('center_axis',(0.,0.,-1.));
#30330=DIRECTION('ref_axis',(1.,0.,0.));
#30331=DIRECTION('center_axis',(0.,0.,1.));
#30332=DIRECTION('ref_axis',(1.,0.,0.));
#30333=DIRECTION('center_axis',(0.,0.,1.));
#30334=DIRECTION('ref_axis',(1.,0.,0.));
#30335=DIRECTION('center_axis',(0.,0.,1.));
#30336=DIRECTION('ref_axis',(1.,0.,0.));
#30337=DIRECTION('center_axis',(0.,0.,1.));
#30338=DIRECTION('ref_axis',(1.,0.,0.));
#30339=DIRECTION('',(0.,0.,1.));
#30340=DIRECTION('center_axis',(0.,0.,-1.));
#30341=DIRECTION('ref_axis',(1.,0.,0.));
#30342=DIRECTION('center_axis',(0.,0.,1.));
#30343=DIRECTION('ref_axis',(1.,0.,0.));
#30344=DIRECTION('center_axis',(0.,0.,1.));
#30345=DIRECTION('ref_axis',(1.,0.,0.));
#30346=DIRECTION('center_axis',(0.,0.,1.));
#30347=DIRECTION('ref_axis',(1.,0.,0.));
#30348=DIRECTION('center_axis',(0.,0.,1.));
#30349=DIRECTION('ref_axis',(1.,0.,0.));
#30350=DIRECTION('',(0.,0.,1.));
#30351=DIRECTION('center_axis',(0.,0.,-1.));
#30352=DIRECTION('ref_axis',(1.,0.,0.));
#30353=DIRECTION('center_axis',(0.,0.,1.));
#30354=DIRECTION('ref_axis',(1.,0.,0.));
#30355=DIRECTION('center_axis',(0.,0.,1.));
#30356=DIRECTION('ref_axis',(1.,0.,0.));
#30357=DIRECTION('center_axis',(0.,0.,1.));
#30358=DIRECTION('ref_axis',(1.,0.,0.));
#30359=DIRECTION('center_axis',(0.,0.,1.));
#30360=DIRECTION('ref_axis',(1.,0.,0.));
#30361=DIRECTION('',(0.,0.,1.));
#30362=DIRECTION('center_axis',(0.,0.,-1.));
#30363=DIRECTION('ref_axis',(1.,0.,0.));
#30364=DIRECTION('center_axis',(0.,0.,1.));
#30365=DIRECTION('ref_axis',(1.,0.,0.));
#30366=DIRECTION('center_axis',(0.,0.,1.));
#30367=DIRECTION('ref_axis',(1.,0.,0.));
#30368=DIRECTION('center_axis',(0.,0.,1.));
#30369=DIRECTION('ref_axis',(1.,0.,0.));
#30370=DIRECTION('center_axis',(0.,0.,1.));
#30371=DIRECTION('ref_axis',(1.,0.,0.));
#30372=DIRECTION('',(0.,0.,1.));
#30373=DIRECTION('center_axis',(0.,0.,1.));
#30374=DIRECTION('ref_axis',(1.,0.,0.));
#30375=DIRECTION('center_axis',(0.,0.,1.));
#30376=DIRECTION('ref_axis',(1.,0.,0.));
#30377=DIRECTION('',(0.,0.,1.));
#30378=DIRECTION('center_axis',(0.,0.,1.));
#30379=DIRECTION('ref_axis',(1.,0.,0.));
#30380=DIRECTION('center_axis',(0.,0.,1.));
#30381=DIRECTION('ref_axis',(1.,0.,0.));
#30382=DIRECTION('',(0.,0.,1.));
#30383=DIRECTION('center_axis',(0.,0.,1.));
#30384=DIRECTION('ref_axis',(1.,0.,0.));
#30385=DIRECTION('center_axis',(0.,0.,1.));
#30386=DIRECTION('ref_axis',(1.,0.,0.));
#30387=DIRECTION('',(0.,0.,1.));
#30388=DIRECTION('center_axis',(0.,-0.56333682464151,0.826227342807548));
#30389=DIRECTION('ref_axis',(0.,-0.826227342807548,-0.56333682464151));
#30390=DIRECTION('',(0.,-0.826227342807548,-0.56333682464151));
#30391=DIRECTION('',(1.,0.,0.));
#30392=DIRECTION('',(0.,-0.826227342807548,-0.56333682464151));
#30393=DIRECTION('',(1.,0.,0.));
#30394=DIRECTION('center_axis',(0.,-1.,0.));
#30395=DIRECTION('ref_axis',(0.,0.,-1.));
#30396=DIRECTION('',(0.,0.,-1.));
#30397=DIRECTION('',(0.,0.,-1.));
#30398=DIRECTION('',(1.,0.,0.));
#30399=DIRECTION('center_axis',(0.,-0.56333682464151,-0.826227342807548));
#30400=DIRECTION('ref_axis',(0.,0.826227342807548,-0.56333682464151));
#30401=DIRECTION('',(0.,0.826227342807548,-0.56333682464151));
#30402=DIRECTION('',(0.,0.826227342807548,-0.56333682464151));
#30403=DIRECTION('',(1.,0.,0.));
#30404=DIRECTION('center_axis',(0.,-1.,0.));
#30405=DIRECTION('ref_axis',(0.,0.,-1.));
#30406=DIRECTION('',(0.,0.,-1.));
#30407=DIRECTION('',(0.,0.,-1.));
#30408=DIRECTION('',(1.,0.,0.));
#30409=DIRECTION('center_axis',(0.,0.,1.));
#30410=DIRECTION('ref_axis',(0.,-1.,0.));
#30411=DIRECTION('',(0.,-1.,0.));
#30412=DIRECTION('',(0.,-1.,0.));
#30413=DIRECTION('',(1.,0.,0.));
#30414=DIRECTION('center_axis',(0.,1.,0.));
#30415=DIRECTION('ref_axis',(0.,0.,1.));
#30416=DIRECTION('',(0.,0.,1.));
#30417=DIRECTION('',(0.,0.,1.));
#30418=DIRECTION('',(1.,0.,0.));
#30419=DIRECTION('center_axis',(0.,0.56333682464151,-0.826227342807548));
#30420=DIRECTION('ref_axis',(0.,0.826227342807548,0.56333682464151));
#30421=DIRECTION('',(0.,0.826227342807548,0.56333682464151));
#30422=DIRECTION('',(0.,0.826227342807548,0.56333682464151));
#30423=DIRECTION('',(1.,0.,0.));
#30424=DIRECTION('center_axis',(0.,1.,0.));
#30425=DIRECTION('ref_axis',(0.,0.,1.));
#30426=DIRECTION('',(0.,0.,1.));
#30427=DIRECTION('',(0.,0.,1.));
#30428=DIRECTION('',(1.,0.,0.));
#30429=DIRECTION('center_axis',(0.,0.56333682464151,0.826227342807548));
#30430=DIRECTION('ref_axis',(0.,-0.826227342807548,0.56333682464151));
#30431=DIRECTION('',(0.,-0.826227342807548,0.56333682464151));
#30432=DIRECTION('',(0.,-0.826227342807548,0.56333682464151));
#30433=DIRECTION('',(1.,0.,0.));
#30434=DIRECTION('center_axis',(0.,1.,0.));
#30435=DIRECTION('ref_axis',(0.,0.,1.));
#30436=DIRECTION('',(0.,0.,1.));
#30437=DIRECTION('',(0.,0.,1.));
#30438=DIRECTION('',(1.,0.,0.));
#30439=DIRECTION('center_axis',(0.,0.,-1.));
#30440=DIRECTION('ref_axis',(0.,1.,0.));
#30441=DIRECTION('',(0.,1.,0.));
#30442=DIRECTION('',(0.,1.,0.));
#30443=DIRECTION('',(1.,0.,0.));
#30444=DIRECTION('center_axis',(0.,-1.,0.));
#30445=DIRECTION('ref_axis',(0.,0.,-1.));
#30446=DIRECTION('',(0.,0.,-1.));
#30447=DIRECTION('',(0.,0.,-1.));
#30448=DIRECTION('center_axis',(1.,0.,0.));
#30449=DIRECTION('ref_axis',(0.,0.,-1.));
#30450=DIRECTION('center_axis',(1.,0.,0.));
#30451=DIRECTION('ref_axis',(0.,0.,-1.));
#30452=DIRECTION('axis',(0.,0.,1.));
#30453=DIRECTION('refdir',(1.,0.,0.));
#30454=DIRECTION('axis',(0.,0.,1.));
#30455=DIRECTION('refdir',(1.,0.,0.));
#30456=DIRECTION('center_axis',(0.,-1.,0.));
#30457=DIRECTION('ref_axis',(0.,0.,-1.));
#30458=DIRECTION('center_axis',(0.,-1.,0.));
#30459=DIRECTION('ref_axis',(1.,0.,0.));
#30460=DIRECTION('center_axis',(0.,-1.,0.));
#30461=DIRECTION('ref_axis',(1.,0.,0.));
#30462=DIRECTION('center_axis',(1.,0.,1.22464679914735E-16));
#30463=DIRECTION('ref_axis',(-1.22464679914735E-16,0.,1.));
#30464=DIRECTION('center_axis',(0.,1.,0.));
#30465=DIRECTION('ref_axis',(1.,0.,0.));
#30466=DIRECTION('center_axis',(0.,1.,0.));
#30467=DIRECTION('ref_axis',(1.,0.,0.));
#30468=DIRECTION('center_axis',(0.,-1.,0.));
#30469=DIRECTION('ref_axis',(1.,0.,0.));
#30470=DIRECTION('',(0.,1.,0.));
#30471=DIRECTION('center_axis',(0.,-1.,0.));
#30472=DIRECTION('ref_axis',(1.,0.,0.));
#30473=DIRECTION('center_axis',(0.,-1.,0.));
#30474=DIRECTION('ref_axis',(1.,0.,0.));
#30475=DIRECTION('center_axis',(0.,-1.,0.));
#30476=DIRECTION('ref_axis',(1.,0.,0.));
#30477=DIRECTION('',(0.,1.,0.));
#30478=DIRECTION('center_axis',(0.,-1.,0.));
#30479=DIRECTION('ref_axis',(1.,0.,0.));
#30480=DIRECTION('center_axis',(0.,1.,0.));
#30481=DIRECTION('ref_axis',(1.,0.,0.));
#30482=DIRECTION('',(-0.707106781186548,0.707106781186547,-8.65956056235493E-17));
#30483=DIRECTION('center_axis',(0.,-1.,0.));
#30484=DIRECTION('ref_axis',(1.,0.,0.));
#30485=DIRECTION('center_axis',(0.,1.,0.));
#30486=DIRECTION('ref_axis',(0.,0.,1.));
#30487=DIRECTION('center_axis',(0.,-1.,0.));
#30488=DIRECTION('ref_axis',(1.,0.,0.));
#30489=DIRECTION('center_axis',(0.,-1.,0.));
#30490=DIRECTION('ref_axis',(1.,0.,0.));
#30491=DIRECTION('',(0.,1.,0.));
#30492=DIRECTION('center_axis',(0.,-1.,0.));
#30493=DIRECTION('ref_axis',(0.,0.,-1.));
#30494=DIRECTION('center_axis',(0.,-1.,0.));
#30495=DIRECTION('ref_axis',(1.,0.,0.));
#30496=DIRECTION('center_axis',(0.,-1.,0.));
#30497=DIRECTION('ref_axis',(1.,0.,0.));
#30498=DIRECTION('',(0.707106781186548,0.707106781186547,8.65956056235493E-17));
#30499=DIRECTION('axis',(0.,0.,1.));
#30500=DIRECTION('refdir',(1.,0.,0.));
#30501=DIRECTION('center_axis',(0.,-1.,0.));
#30502=DIRECTION('ref_axis',(0.,0.,-1.));
#30503=DIRECTION('center_axis',(0.,-1.,0.));
#30504=DIRECTION('ref_axis',(1.,0.,0.));
#30505=DIRECTION('center_axis',(0.,-1.,0.));
#30506=DIRECTION('ref_axis',(1.,0.,0.));
#30507=DIRECTION('center_axis',(1.,0.,1.22464679914735E-16));
#30508=DIRECTION('ref_axis',(-1.22464679914735E-16,0.,1.));
#30509=DIRECTION('center_axis',(0.,1.,0.));
#30510=DIRECTION('ref_axis',(1.,0.,0.));
#30511=DIRECTION('center_axis',(0.,1.,0.));
#30512=DIRECTION('ref_axis',(1.,0.,0.));
#30513=DIRECTION('center_axis',(0.,-1.,0.));
#30514=DIRECTION('ref_axis',(1.,0.,0.));
#30515=DIRECTION('center_axis',(0.,-1.,0.));
#30516=DIRECTION('ref_axis',(1.,0.,0.));
#30517=DIRECTION('',(0.,1.,0.));
#30518=DIRECTION('center_axis',(0.,1.,0.));
#30519=DIRECTION('ref_axis',(0.,0.,1.));
#30520=DIRECTION('center_axis',(0.,-1.,0.));
#30521=DIRECTION('ref_axis',(1.,0.,0.));
#30522=DIRECTION('center_axis',(0.,-1.,0.));
#30523=DIRECTION('ref_axis',(1.,0.,0.));
#30524=DIRECTION('center_axis',(0.,-1.,0.));
#30525=DIRECTION('ref_axis',(1.,0.,0.));
#30526=DIRECTION('center_axis',(0.,-1.,0.));
#30527=DIRECTION('ref_axis',(1.,0.,0.));
#30528=DIRECTION('',(0.707106781186548,0.707106781186547,8.65956056235494E-17));
#30529=DIRECTION('center_axis',(0.,-1.,0.));
#30530=DIRECTION('ref_axis',(1.,0.,0.));
#30531=DIRECTION('center_axis',(0.,-1.,0.));
#30532=DIRECTION('ref_axis',(1.,0.,0.));
#30533=DIRECTION('',(0.,1.,0.));
#30534=DIRECTION('center_axis',(0.,1.,0.));
#30535=DIRECTION('ref_axis',(1.,0.,0.));
#30536=DIRECTION('center_axis',(0.,-1.,0.));
#30537=DIRECTION('ref_axis',(1.,0.,0.));
#30538=DIRECTION('',(-0.707106781186548,0.707106781186547,-8.65956056235494E-17));
#30539=DIRECTION('center_axis',(0.,-1.,0.));
#30540=DIRECTION('ref_axis',(0.,0.,-1.));
#30541=DIRECTION('center_axis',(0.,-1.,0.));
#30542=DIRECTION('ref_axis',(1.,0.,0.));
#30543=DIRECTION('',(0.,1.,0.));
#30544=DIRECTION('axis',(0.,0.,1.));
#30545=DIRECTION('refdir',(1.,0.,0.));
#30546=DIRECTION('center_axis',(0.,0.,1.));
#30547=DIRECTION('ref_axis',(1.,0.,0.));
#30548=DIRECTION('center_axis',(1.22464679914735E-16,-1.,0.));
#30549=DIRECTION('ref_axis',(-1.,-1.22464679914735E-16,0.));
#30550=DIRECTION('center_axis',(0.78183148246803,0.,0.623489801858733));
#30551=DIRECTION('ref_axis',(0.623489801858734,0.,-0.78183148246803));
#30552=DIRECTION('center_axis',(7.63554790147315E-17,-1.,-9.57467422477103E-17));
#30553=DIRECTION('ref_axis',(-0.623489801858734,-1.22464679914735E-16,0.78183148246803));
#30554=DIRECTION('center_axis',(0.974927912181824,0.,-0.222520933956314));
#30555=DIRECTION('ref_axis',(-0.222520933956314,0.,-0.974927912181824));
#30556=DIRECTION('center_axis',(-2.7250954951288E-17,-1.,-1.19394234705288E-16));
#30557=DIRECTION('ref_axis',(0.222520933956314,-1.22464679914735E-16,0.974927912181824));
#30558=DIRECTION('center_axis',(0.433883739117558,0.,-0.900968867902419));
#30559=DIRECTION('ref_axis',(-0.900968867902419,0.,-0.433883739117558));
#30560=DIRECTION('center_axis',(-1.10336864020811E-16,-1.,-5.31354332312403E-17));
#30561=DIRECTION('ref_axis',(0.900968867902419,-1.22464679914735E-16,0.433883739117558));
#30562=DIRECTION('center_axis',(-0.433883739117558,0.,-0.900968867902419));
#30563=DIRECTION('ref_axis',(-0.900968867902419,0.,0.433883739117558));
#30564=DIRECTION('center_axis',(-1.10336864020811E-16,-1.,5.31354332312403E-17));
#30565=DIRECTION('ref_axis',(0.900968867902419,-1.22464679914735E-16,-0.433883739117558));
#30566=DIRECTION('center_axis',(-0.974927912181824,0.,-0.222520933956314));
#30567=DIRECTION('ref_axis',(-0.222520933956315,0.,0.974927912181824));
#30568=DIRECTION('center_axis',(-2.7250954951288E-17,-1.,1.19394234705288E-16));
#30569=DIRECTION('ref_axis',(0.222520933956315,-1.22464679914735E-16,-0.974927912181824));
#30570=DIRECTION('center_axis',(-0.78183148246803,0.,0.623489801858734));
#30571=DIRECTION('ref_axis',(0.623489801858733,0.,0.78183148246803));
#30572=DIRECTION('center_axis',(7.63554790147315E-17,-1.,9.57467422477103E-17));
#30573=DIRECTION('ref_axis',(-0.623489801858733,-1.22464679914735E-16,-0.78183148246803));
#30574=DIRECTION('axis',(0.,0.,1.));
#30575=DIRECTION('refdir',(1.,0.,0.));
#30576=DIRECTION('center_axis',(0.,0.,1.));
#30577=DIRECTION('ref_axis',(1.,0.,0.));
#30578=DIRECTION('center_axis',(0.,-1.,0.));
#30579=DIRECTION('ref_axis',(0.,0.,-1.));
#30580=DIRECTION('center_axis',(0.,-1.,0.));
#30581=DIRECTION('ref_axis',(0.,0.,-1.));
#30582=DIRECTION('center_axis',(0.,1.,0.));
#30583=DIRECTION('ref_axis',(1.,0.,0.));
#30584=DIRECTION('center_axis',(0.,1.,0.));
#30585=DIRECTION('ref_axis',(1.,0.,0.));
#30586=DIRECTION('center_axis',(0.,1.,0.));
#30587=DIRECTION('ref_axis',(1.,0.,0.));
#30588=DIRECTION('center_axis',(0.,1.,0.));
#30589=DIRECTION('ref_axis',(1.,0.,0.));
#30590=DIRECTION('',(0.,-1.,0.));
#30591=DIRECTION('center_axis',(0.,-1.,0.));
#30592=DIRECTION('ref_axis',(1.,0.,0.));
#30593=DIRECTION('center_axis',(0.,1.,0.));
#30594=DIRECTION('ref_axis',(1.,0.,0.));
#30595=DIRECTION('center_axis',(0.,1.,0.));
#30596=DIRECTION('ref_axis',(1.,0.,0.));
#30597=DIRECTION('center_axis',(0.,1.,0.));
#30598=DIRECTION('ref_axis',(1.,0.,0.));
#30599=DIRECTION('center_axis',(0.,1.,0.));
#30600=DIRECTION('ref_axis',(1.,0.,0.));
#30601=DIRECTION('center_axis',(0.,1.,0.));
#30602=DIRECTION('ref_axis',(1.,0.,0.));
#30603=DIRECTION('center_axis',(0.,1.,0.));
#30604=DIRECTION('ref_axis',(1.,0.,0.));
#30605=DIRECTION('center_axis',(0.,-1.,0.));
#30606=DIRECTION('ref_axis',(1.,0.,0.));
#30607=DIRECTION('center_axis',(0.,-1.,0.));
#30608=DIRECTION('ref_axis',(0.,0.,-1.));
#30609=DIRECTION('center_axis',(8.96625347776458E-17,0.,1.));
#30610=DIRECTION('ref_axis',(1.,0.,0.));
#30611=DIRECTION('center_axis',(0.,-1.,0.));
#30612=DIRECTION('ref_axis',(0.,0.,-1.));
#30613=DIRECTION('center_axis',(0.,1.,0.));
#30614=DIRECTION('ref_axis',(1.,0.,0.));
#30615=DIRECTION('center_axis',(0.,-1.,0.));
#30616=DIRECTION('ref_axis',(1.,0.,0.));
#30617=DIRECTION('center_axis',(0.,-1.,0.));
#30618=DIRECTION('ref_axis',(0.,0.,-1.));
#30619=DIRECTION('center_axis',(0.,0.,1.));
#30620=DIRECTION('ref_axis',(1.,0.,0.));
#30621=DIRECTION('center_axis',(0.,-1.,0.));
#30622=DIRECTION('ref_axis',(0.,0.,-1.));
#30623=DIRECTION('center_axis',(0.,1.,0.));
#30624=DIRECTION('ref_axis',(1.,0.,0.));
#30625=DIRECTION('center_axis',(0.,-1.,0.));
#30626=DIRECTION('ref_axis',(1.,0.,0.));
#30627=DIRECTION('center_axis',(0.,-1.,0.));
#30628=DIRECTION('ref_axis',(1.,0.,0.));
#30629=DIRECTION('center_axis',(0.,-1.,0.));
#30630=DIRECTION('ref_axis',(0.,0.,-1.));
#30631=DIRECTION('center_axis',(0.,0.,1.));
#30632=DIRECTION('ref_axis',(1.,0.,0.));
#30633=DIRECTION('center_axis',(0.,-1.,0.));
#30634=DIRECTION('ref_axis',(0.,0.,-1.));
#30635=DIRECTION('center_axis',(0.,1.,0.));
#30636=DIRECTION('ref_axis',(1.,0.,0.));
#30637=DIRECTION('center_axis',(0.,-1.,0.));
#30638=DIRECTION('ref_axis',(1.,0.,0.));
#30639=DIRECTION('center_axis',(0.,-1.,0.));
#30640=DIRECTION('ref_axis',(0.,0.,-1.));
#30641=DIRECTION('center_axis',(8.96625347776458E-17,0.,1.));
#30642=DIRECTION('ref_axis',(1.,0.,0.));
#30643=DIRECTION('center_axis',(0.,-1.,0.));
#30644=DIRECTION('ref_axis',(0.,0.,-1.));
#30645=DIRECTION('center_axis',(0.,1.,0.));
#30646=DIRECTION('ref_axis',(1.,0.,0.));
#30647=DIRECTION('center_axis',(0.,-1.,0.));
#30648=DIRECTION('ref_axis',(1.,0.,0.));
#30649=DIRECTION('center_axis',(0.,-1.,0.));
#30650=DIRECTION('ref_axis',(0.,0.,-1.));
#30651=DIRECTION('center_axis',(0.,0.,1.));
#30652=DIRECTION('ref_axis',(1.,0.,0.));
#30653=DIRECTION('center_axis',(0.,-1.,0.));
#30654=DIRECTION('ref_axis',(0.,0.,-1.));
#30655=DIRECTION('center_axis',(0.,1.,0.));
#30656=DIRECTION('ref_axis',(1.,0.,0.));
#30657=DIRECTION('center_axis',(0.,1.,0.));
#30658=DIRECTION('ref_axis',(1.,0.,0.));
#30659=DIRECTION('',(0.,1.,0.));
#30660=DIRECTION('center_axis',(0.,-1.,0.));
#30661=DIRECTION('ref_axis',(1.,0.,0.));
#30662=DIRECTION('center_axis',(0.,-1.,0.));
#30663=DIRECTION('ref_axis',(1.,0.,0.));
#30664=DIRECTION('center_axis',(0.,1.,0.));
#30665=DIRECTION('ref_axis',(1.,0.,0.));
#30666=DIRECTION('center_axis',(0.,-1.,0.));
#30667=DIRECTION('ref_axis',(0.,0.,-1.));
#30668=DIRECTION('center_axis',(0.,0.,1.));
#30669=DIRECTION('ref_axis',(1.,0.,0.));
#30670=DIRECTION('center_axis',(0.,-1.,0.));
#30671=DIRECTION('ref_axis',(0.,0.,-1.));
#30672=DIRECTION('center_axis',(0.,-1.,0.));
#30673=DIRECTION('ref_axis',(-1.,0.,0.));
#30674=DIRECTION('center_axis',(0.,1.,0.));
#30675=DIRECTION('ref_axis',(1.,0.,0.));
#30676=DIRECTION('axis',(0.,0.,1.));
#30677=DIRECTION('refdir',(1.,0.,0.));
#30678=DIRECTION('center_axis',(0.,1.,0.));
#30679=DIRECTION('ref_axis',(0.,0.,1.));
#30680=DIRECTION('center_axis',(0.,-1.,0.));
#30681=DIRECTION('ref_axis',(1.,0.,0.));
#30682=DIRECTION('center_axis',(0.,-1.,0.));
#30683=DIRECTION('ref_axis',(1.,0.,0.));
#30684=DIRECTION('center_axis',(0.,-1.,0.));
#30685=DIRECTION('ref_axis',(1.,0.,0.));
#30686=DIRECTION('center_axis',(0.,-1.,0.));
#30687=DIRECTION('ref_axis',(1.,0.,0.));
#30688=DIRECTION('',(0.,1.,0.));
#30689=DIRECTION('center_axis',(0.,-1.,0.));
#30690=DIRECTION('ref_axis',(0.,0.,-1.));
#30691=DIRECTION('center_axis',(0.,-1.,0.));
#30692=DIRECTION('ref_axis',(1.,0.,0.));
#30693=DIRECTION('center_axis',(0.,-1.,0.));
#30694=DIRECTION('ref_axis',(1.,0.,0.));
#30695=DIRECTION('',(0.,1.,0.));
#30696=DIRECTION('center_axis',(0.,1.,0.));
#30697=DIRECTION('ref_axis',(0.,0.,1.));
#30698=DIRECTION('center_axis',(0.,-1.,0.));
#30699=DIRECTION('ref_axis',(1.,0.,0.));
#30700=DIRECTION('center_axis',(0.,-1.,0.));
#30701=DIRECTION('ref_axis',(1.,0.,0.));
#30702=DIRECTION('center_axis',(0.,-1.,0.));
#30703=DIRECTION('ref_axis',(1.,0.,0.));
#30704=DIRECTION('center_axis',(0.,-1.,0.));
#30705=DIRECTION('ref_axis',(1.,0.,0.));
#30706=DIRECTION('',(0.,1.,0.));
#30707=DIRECTION('center_axis',(0.,-1.,0.));
#30708=DIRECTION('ref_axis',(0.,0.,-1.));
#30709=DIRECTION('center_axis',(0.,-1.,0.));
#30710=DIRECTION('ref_axis',(1.,0.,0.));
#30711=DIRECTION('center_axis',(0.,-1.,0.));
#30712=DIRECTION('ref_axis',(1.,0.,0.));
#30713=DIRECTION('',(0.,1.,0.));
#30714=DIRECTION('',(0.,0.,1.));
#30715=DIRECTION('',(1.,0.,0.));
#30716=DIRECTION('',(0.,0.,1.));
#30717=DIRECTION('',(1.,0.,0.));
#30718=DIRECTION('',(0.,0.,1.));
#30719=DIRECTION('',(1.,0.,0.));
#30720=DIRECTION('',(0.,0.,1.));
#30721=DIRECTION('',(1.,0.,0.));
#30722=DIRECTION('',(0.,0.,1.));
#30723=DIRECTION('',(1.,0.,0.));
#30724=DIRECTION('axis',(0.,0.,1.));
#30725=DIRECTION('refdir',(1.,0.,0.));
#30726=DIRECTION('axis',(0.,0.,1.));
#30727=DIRECTION('refdir',(1.,0.,0.));
#30728=DIRECTION('center_axis',(0.,-1.,0.));
#30729=DIRECTION('ref_axis',(0.,0.,-1.));
#30730=DIRECTION('center_axis',(0.,-1.,0.));
#30731=DIRECTION('ref_axis',(1.,0.,0.));
#30732=DIRECTION('center_axis',(0.,-1.,0.));
#30733=DIRECTION('ref_axis',(1.,0.,0.));
#30734=DIRECTION('center_axis',(1.,0.,1.22464679914735E-16));
#30735=DIRECTION('ref_axis',(-1.22464679914735E-16,0.,1.));
#30736=DIRECTION('center_axis',(0.,1.,0.));
#30737=DIRECTION('ref_axis',(1.,0.,0.));
#30738=DIRECTION('center_axis',(0.,1.,0.));
#30739=DIRECTION('ref_axis',(1.,0.,0.));
#30740=DIRECTION('center_axis',(0.,-1.,0.));
#30741=DIRECTION('ref_axis',(1.,0.,0.));
#30742=DIRECTION('',(0.,1.,0.));
#30743=DIRECTION('center_axis',(0.,-1.,0.));
#30744=DIRECTION('ref_axis',(1.,0.,0.));
#30745=DIRECTION('center_axis',(0.,-1.,0.));
#30746=DIRECTION('ref_axis',(1.,0.,0.));
#30747=DIRECTION('center_axis',(0.,-1.,0.));
#30748=DIRECTION('ref_axis',(1.,0.,0.));
#30749=DIRECTION('',(0.,1.,0.));
#30750=DIRECTION('center_axis',(0.,-1.,0.));
#30751=DIRECTION('ref_axis',(1.,0.,0.));
#30752=DIRECTION('center_axis',(0.,1.,0.));
#30753=DIRECTION('ref_axis',(1.,0.,0.));
#30754=DIRECTION('',(-0.707106781186548,0.707106781186547,-8.65956056235494E-17));
#30755=DIRECTION('center_axis',(0.,-1.,0.));
#30756=DIRECTION('ref_axis',(1.,0.,0.));
#30757=DIRECTION('center_axis',(0.,1.,0.));
#30758=DIRECTION('ref_axis',(0.,0.,1.));
#30759=DIRECTION('center_axis',(0.,-1.,0.));
#30760=DIRECTION('ref_axis',(1.,0.,0.));
#30761=DIRECTION('center_axis',(0.,-1.,0.));
#30762=DIRECTION('ref_axis',(1.,0.,0.));
#30763=DIRECTION('',(0.,1.,0.));
#30764=DIRECTION('center_axis',(0.,-1.,0.));
#30765=DIRECTION('ref_axis',(0.,0.,-1.));
#30766=DIRECTION('center_axis',(0.,-1.,0.));
#30767=DIRECTION('ref_axis',(1.,0.,0.));
#30768=DIRECTION('center_axis',(0.,-1.,0.));
#30769=DIRECTION('ref_axis',(1.,0.,0.));
#30770=DIRECTION('',(0.707106781186548,0.707106781186547,8.65956056235494E-17));
#30771=DIRECTION('axis',(0.,0.,1.));
#30772=DIRECTION('refdir',(1.,0.,0.));
#30773=DIRECTION('center_axis',(0.,-1.,0.));
#30774=DIRECTION('ref_axis',(0.,0.,-1.));
#30775=DIRECTION('center_axis',(0.,-1.,0.));
#30776=DIRECTION('ref_axis',(1.,0.,0.));
#30777=DIRECTION('center_axis',(0.,-1.,0.));
#30778=DIRECTION('ref_axis',(1.,0.,0.));
#30779=DIRECTION('center_axis',(1.,0.,1.22464679914735E-16));
#30780=DIRECTION('ref_axis',(-1.22464679914735E-16,0.,1.));
#30781=DIRECTION('center_axis',(0.,1.,0.));
#30782=DIRECTION('ref_axis',(1.,0.,0.));
#30783=DIRECTION('center_axis',(0.,1.,0.));
#30784=DIRECTION('ref_axis',(1.,0.,0.));
#30785=DIRECTION('center_axis',(0.,-1.,0.));
#30786=DIRECTION('ref_axis',(1.,0.,0.));
#30787=DIRECTION('center_axis',(0.,-1.,0.));
#30788=DIRECTION('ref_axis',(1.,0.,0.));
#30789=DIRECTION('',(0.,1.,0.));
#30790=DIRECTION('center_axis',(0.,1.,0.));
#30791=DIRECTION('ref_axis',(0.,0.,1.));
#30792=DIRECTION('center_axis',(0.,-1.,0.));
#30793=DIRECTION('ref_axis',(1.,0.,0.));
#30794=DIRECTION('center_axis',(0.,-1.,0.));
#30795=DIRECTION('ref_axis',(1.,0.,0.));
#30796=DIRECTION('center_axis',(0.,-1.,0.));
#30797=DIRECTION('ref_axis',(1.,0.,0.));
#30798=DIRECTION('center_axis',(0.,-1.,0.));
#30799=DIRECTION('ref_axis',(1.,0.,0.));
#30800=DIRECTION('',(0.707106781186548,0.707106781186547,8.65956056235494E-17));
#30801=DIRECTION('center_axis',(0.,-1.,0.));
#30802=DIRECTION('ref_axis',(1.,0.,0.));
#30803=DIRECTION('center_axis',(0.,-1.,0.));
#30804=DIRECTION('ref_axis',(1.,0.,0.));
#30805=DIRECTION('',(0.,1.,0.));
#30806=DIRECTION('center_axis',(0.,1.,0.));
#30807=DIRECTION('ref_axis',(1.,0.,0.));
#30808=DIRECTION('center_axis',(0.,-1.,0.));
#30809=DIRECTION('ref_axis',(1.,0.,0.));
#30810=DIRECTION('',(-0.707106781186548,0.707106781186547,-8.65956056235494E-17));
#30811=DIRECTION('center_axis',(0.,-1.,0.));
#30812=DIRECTION('ref_axis',(0.,0.,-1.));
#30813=DIRECTION('center_axis',(0.,-1.,0.));
#30814=DIRECTION('ref_axis',(1.,0.,0.));
#30815=DIRECTION('',(0.,1.,0.));
#30816=DIRECTION('axis',(0.,0.,1.));
#30817=DIRECTION('refdir',(1.,0.,0.));
#30818=DIRECTION('center_axis',(0.,0.,1.));
#30819=DIRECTION('ref_axis',(1.,0.,0.));
#30820=DIRECTION('center_axis',(1.22464679914735E-16,-1.,0.));
#30821=DIRECTION('ref_axis',(-1.,-1.22464679914735E-16,0.));
#30822=DIRECTION('center_axis',(0.707106781186548,0.,0.707106781186548));
#30823=DIRECTION('ref_axis',(0.707106781186548,0.,-0.707106781186548));
#30824=DIRECTION('center_axis',(8.65956056235493E-17,-1.,-8.65956056235493E-17));
#30825=DIRECTION('ref_axis',(-0.707106781186548,-1.22464679914735E-16,0.707106781186548));
#30826=DIRECTION('center_axis',(1.,0.,0.));
#30827=DIRECTION('ref_axis',(6.12323399573677E-17,0.,-1.));
#30828=DIRECTION('center_axis',(7.49879891330929E-33,-1.,-1.22464679914735E-16));
#30829=DIRECTION('ref_axis',(-6.12323399573677E-17,-1.22464679914735E-16,
1.));
#30830=DIRECTION('center_axis',(0.707106781186548,0.,-0.707106781186548));
#30831=DIRECTION('ref_axis',(-0.707106781186548,0.,-0.707106781186548));
#30832=DIRECTION('center_axis',(-8.65956056235493E-17,-1.,-8.65956056235493E-17));
#30833=DIRECTION('ref_axis',(0.707106781186548,-1.22464679914735E-16,0.707106781186548));
#30834=DIRECTION('center_axis',(0.,0.,-1.));
#30835=DIRECTION('ref_axis',(-1.,0.,-1.22464679914735E-16));
#30836=DIRECTION('center_axis',(-1.22464679914735E-16,-1.,-1.49975978266186E-32));
#30837=DIRECTION('ref_axis',(1.,-1.22464679914735E-16,1.22464679914735E-16));
#30838=DIRECTION('center_axis',(-0.707106781186548,0.,-0.707106781186548));
#30839=DIRECTION('ref_axis',(-0.707106781186548,0.,0.707106781186548));
#30840=DIRECTION('center_axis',(-8.65956056235493E-17,-1.,8.65956056235493E-17));
#30841=DIRECTION('ref_axis',(0.707106781186548,-1.22464679914735E-16,-0.707106781186548));
#30842=DIRECTION('center_axis',(-1.,0.,0.));
#30843=DIRECTION('ref_axis',(-1.83697019872103E-16,0.,1.));
#30844=DIRECTION('center_axis',(-2.24963967399279E-32,-1.,1.22464679914735E-16));
#30845=DIRECTION('ref_axis',(1.83697019872103E-16,-1.22464679914735E-16,
-1.));
#30846=DIRECTION('center_axis',(-0.707106781186548,0.,0.707106781186548));
#30847=DIRECTION('ref_axis',(0.707106781186548,0.,0.707106781186548));
#30848=DIRECTION('center_axis',(8.65956056235493E-17,-1.,8.65956056235494E-17));
#30849=DIRECTION('ref_axis',(-0.707106781186548,-1.22464679914735E-16,-0.707106781186548));
#30850=DIRECTION('axis',(0.,0.,1.));
#30851=DIRECTION('refdir',(1.,0.,0.));
#30852=DIRECTION('center_axis',(0.,0.,1.));
#30853=DIRECTION('ref_axis',(1.,0.,0.));
#30854=DIRECTION('center_axis',(0.,-1.,0.));
#30855=DIRECTION('ref_axis',(0.,0.,-1.));
#30856=DIRECTION('center_axis',(0.,-1.,0.));
#30857=DIRECTION('ref_axis',(0.,0.,-1.));
#30858=DIRECTION('center_axis',(0.,1.,0.));
#30859=DIRECTION('ref_axis',(1.,0.,0.));
#30860=DIRECTION('center_axis',(0.,1.,0.));
#30861=DIRECTION('ref_axis',(1.,0.,0.));
#30862=DIRECTION('center_axis',(0.,1.,0.));
#30863=DIRECTION('ref_axis',(1.,0.,0.));
#30864=DIRECTION('center_axis',(0.,1.,0.));
#30865=DIRECTION('ref_axis',(1.,0.,0.));
#30866=DIRECTION('',(0.,-1.,0.));
#30867=DIRECTION('center_axis',(0.,-1.,0.));
#30868=DIRECTION('ref_axis',(1.,0.,0.));
#30869=DIRECTION('center_axis',(0.,1.,0.));
#30870=DIRECTION('ref_axis',(1.,0.,0.));
#30871=DIRECTION('center_axis',(0.,1.,0.));
#30872=DIRECTION('ref_axis',(1.,0.,0.));
#30873=DIRECTION('center_axis',(0.,1.,0.));
#30874=DIRECTION('ref_axis',(1.,0.,0.));
#30875=DIRECTION('center_axis',(0.,1.,0.));
#30876=DIRECTION('ref_axis',(1.,0.,0.));
#30877=DIRECTION('center_axis',(0.,1.,0.));
#30878=DIRECTION('ref_axis',(1.,0.,0.));
#30879=DIRECTION('center_axis',(0.,1.,0.));
#30880=DIRECTION('ref_axis',(1.,0.,0.));
#30881=DIRECTION('center_axis',(0.,-1.,0.));
#30882=DIRECTION('ref_axis',(1.,0.,0.));
#30883=DIRECTION('center_axis',(0.,-1.,0.));
#30884=DIRECTION('ref_axis',(0.,0.,-1.));
#30885=DIRECTION('center_axis',(6.12323399573677E-17,0.,1.));
#30886=DIRECTION('ref_axis',(1.,0.,0.));
#30887=DIRECTION('center_axis',(0.,-1.,0.));
#30888=DIRECTION('ref_axis',(0.,0.,-1.));
#30889=DIRECTION('center_axis',(0.,1.,0.));
#30890=DIRECTION('ref_axis',(1.,0.,0.));
#30891=DIRECTION('center_axis',(0.,-1.,0.));
#30892=DIRECTION('ref_axis',(1.,0.,0.));
#30893=DIRECTION('center_axis',(0.,-1.,0.));
#30894=DIRECTION('ref_axis',(0.,0.,-1.));
#30895=DIRECTION('center_axis',(0.,0.,1.));
#30896=DIRECTION('ref_axis',(1.,0.,0.));
#30897=DIRECTION('center_axis',(0.,-1.,0.));
#30898=DIRECTION('ref_axis',(0.,0.,-1.));
#30899=DIRECTION('center_axis',(0.,1.,0.));
#30900=DIRECTION('ref_axis',(1.,0.,0.));
#30901=DIRECTION('center_axis',(0.,-1.,0.));
#30902=DIRECTION('ref_axis',(1.,0.,0.));
#30903=DIRECTION('center_axis',(0.,-1.,0.));
#30904=DIRECTION('ref_axis',(0.,0.,-1.));
#30905=DIRECTION('center_axis',(0.,0.,1.));
#30906=DIRECTION('ref_axis',(1.,0.,0.));
#30907=DIRECTION('center_axis',(0.,-1.,0.));
#30908=DIRECTION('ref_axis',(0.,0.,-1.));
#30909=DIRECTION('center_axis',(0.,1.,0.));
#30910=DIRECTION('ref_axis',(1.,0.,0.));
#30911=DIRECTION('center_axis',(0.,-1.,0.));
#30912=DIRECTION('ref_axis',(1.,0.,0.));
#30913=DIRECTION('center_axis',(0.,-1.,0.));
#30914=DIRECTION('ref_axis',(0.,0.,-1.));
#30915=DIRECTION('center_axis',(0.,0.,1.));
#30916=DIRECTION('ref_axis',(1.,0.,0.));
#30917=DIRECTION('center_axis',(0.,-1.,0.));
#30918=DIRECTION('ref_axis',(0.,0.,-1.));
#30919=DIRECTION('center_axis',(0.,1.,0.));
#30920=DIRECTION('ref_axis',(1.,0.,0.));
#30921=DIRECTION('center_axis',(0.,-1.,0.));
#30922=DIRECTION('ref_axis',(1.,0.,0.));
#30923=DIRECTION('center_axis',(0.,-1.,0.));
#30924=DIRECTION('ref_axis',(0.,0.,-1.));
#30925=DIRECTION('center_axis',(6.12323399573676E-17,0.,1.));
#30926=DIRECTION('ref_axis',(1.,0.,0.));
#30927=DIRECTION('center_axis',(0.,-1.,0.));
#30928=DIRECTION('ref_axis',(0.,0.,-1.));
#30929=DIRECTION('center_axis',(0.,1.,0.));
#30930=DIRECTION('ref_axis',(1.,0.,0.));
#30931=DIRECTION('center_axis',(0.,-1.,0.));
#30932=DIRECTION('ref_axis',(1.,0.,0.));
#30933=DIRECTION('center_axis',(0.,-1.,0.));
#30934=DIRECTION('ref_axis',(0.,0.,-1.));
#30935=DIRECTION('center_axis',(0.,0.,1.));
#30936=DIRECTION('ref_axis',(1.,0.,0.));
#30937=DIRECTION('center_axis',(0.,-1.,0.));
#30938=DIRECTION('ref_axis',(0.,0.,-1.));
#30939=DIRECTION('center_axis',(0.,1.,0.));
#30940=DIRECTION('ref_axis',(1.,0.,0.));
#30941=DIRECTION('center_axis',(0.,1.,0.));
#30942=DIRECTION('ref_axis',(1.,0.,0.));
#30943=DIRECTION('',(0.,1.,0.));
#30944=DIRECTION('center_axis',(0.,-1.,0.));
#30945=DIRECTION('ref_axis',(1.,0.,0.));
#30946=DIRECTION('center_axis',(0.,-1.,0.));
#30947=DIRECTION('ref_axis',(1.,0.,0.));
#30948=DIRECTION('center_axis',(0.,1.,0.));
#30949=DIRECTION('ref_axis',(1.,0.,0.));
#30950=DIRECTION('center_axis',(0.,-1.,0.));
#30951=DIRECTION('ref_axis',(0.,0.,-1.));
#30952=DIRECTION('center_axis',(0.,0.,1.));
#30953=DIRECTION('ref_axis',(1.,0.,0.));
#30954=DIRECTION('center_axis',(0.,-1.,0.));
#30955=DIRECTION('ref_axis',(0.,0.,-1.));
#30956=DIRECTION('center_axis',(0.,-1.,0.));
#30957=DIRECTION('ref_axis',(-1.,0.,0.));
#30958=DIRECTION('center_axis',(0.,1.,0.));
#30959=DIRECTION('ref_axis',(1.,0.,0.));
#30960=DIRECTION('axis',(0.,0.,1.));
#30961=DIRECTION('refdir',(1.,0.,0.));
#30962=DIRECTION('center_axis',(0.,1.,0.));
#30963=DIRECTION('ref_axis',(0.,0.,1.));
#30964=DIRECTION('center_axis',(0.,-1.,0.));
#30965=DIRECTION('ref_axis',(1.,0.,0.));
#30966=DIRECTION('center_axis',(0.,-1.,0.));
#30967=DIRECTION('ref_axis',(1.,0.,0.));
#30968=DIRECTION('center_axis',(0.,-1.,0.));
#30969=DIRECTION('ref_axis',(1.,0.,0.));
#30970=DIRECTION('center_axis',(0.,-1.,0.));
#30971=DIRECTION('ref_axis',(1.,0.,0.));
#30972=DIRECTION('',(0.,1.,0.));
#30973=DIRECTION('center_axis',(0.,-1.,0.));
#30974=DIRECTION('ref_axis',(0.,0.,-1.));
#30975=DIRECTION('center_axis',(0.,-1.,0.));
#30976=DIRECTION('ref_axis',(1.,0.,0.));
#30977=DIRECTION('center_axis',(0.,-1.,0.));
#30978=DIRECTION('ref_axis',(1.,0.,0.));
#30979=DIRECTION('',(0.,1.,0.));
#30980=DIRECTION('center_axis',(0.,1.,0.));
#30981=DIRECTION('ref_axis',(0.,0.,1.));
#30982=DIRECTION('center_axis',(0.,-1.,0.));
#30983=DIRECTION('ref_axis',(1.,0.,0.));
#30984=DIRECTION('center_axis',(0.,-1.,0.));
#30985=DIRECTION('ref_axis',(1.,0.,0.));
#30986=DIRECTION('center_axis',(0.,-1.,0.));
#30987=DIRECTION('ref_axis',(1.,0.,0.));
#30988=DIRECTION('center_axis',(0.,-1.,0.));
#30989=DIRECTION('ref_axis',(1.,0.,0.));
#30990=DIRECTION('',(0.,1.,0.));
#30991=DIRECTION('center_axis',(0.,-1.,0.));
#30992=DIRECTION('ref_axis',(0.,0.,-1.));
#30993=DIRECTION('center_axis',(0.,-1.,0.));
#30994=DIRECTION('ref_axis',(1.,0.,0.));
#30995=DIRECTION('center_axis',(0.,-1.,0.));
#30996=DIRECTION('ref_axis',(1.,0.,0.));
#30997=DIRECTION('',(0.,1.,0.));
#30998=DIRECTION('',(0.,0.,1.));
#30999=DIRECTION('',(1.,0.,0.));
#31000=DIRECTION('',(0.,0.,1.));
#31001=DIRECTION('',(1.,0.,0.));
#31002=DIRECTION('',(0.,0.,1.));
#31003=DIRECTION('',(1.,0.,0.));
#31004=DIRECTION('',(0.,0.,1.));
#31005=DIRECTION('',(1.,0.,0.));
#31006=DIRECTION('',(0.,0.,1.));
#31007=DIRECTION('',(1.,0.,0.));
#31008=DIRECTION('axis',(0.,0.,1.));
#31009=DIRECTION('refdir',(1.,0.,0.));
#31010=DIRECTION('center_axis',(0.866025403784439,0.,-0.5));
#31011=DIRECTION('ref_axis',(0.5,0.,0.866025403784439));
#31012=DIRECTION('',(-0.5,0.,-0.866025403784439));
#31013=DIRECTION('',(0.,-1.,0.));
#31014=DIRECTION('',(0.5,0.,0.866025403784439));
#31015=DIRECTION('',(0.,-1.,0.));
#31016=DIRECTION('center_axis',(1.20185167898973E-16,0.,-1.));
#31017=DIRECTION('ref_axis',(1.,0.,1.20185167898973E-16));
#31018=DIRECTION('',(-1.,0.,-1.20185167898973E-16));
#31019=DIRECTION('',(0.,-1.,0.));
#31020=DIRECTION('',(1.,0.,1.20185167898973E-16));
#31021=DIRECTION('center_axis',(-0.866025403784439,0.,-0.5));
#31022=DIRECTION('ref_axis',(0.5,0.,-0.866025403784439));
#31023=DIRECTION('',(-0.5,0.,0.866025403784439));
#31024=DIRECTION('',(0.,-1.,0.));
#31025=DIRECTION('',(0.5,0.,-0.866025403784439));
#31026=DIRECTION('center_axis',(-0.866025403784439,0.,0.5));
#31027=DIRECTION('ref_axis',(-0.5,0.,-0.866025403784439));
#31028=DIRECTION('',(0.5,0.,0.866025403784439));
#31029=DIRECTION('',(0.,-1.,0.));
#31030=DIRECTION('',(-0.5,0.,-0.866025403784439));
#31031=DIRECTION('center_axis',(-2.40370335797945E-16,0.,1.));
#31032=DIRECTION('ref_axis',(-1.,0.,-2.40370335797945E-16));
#31033=DIRECTION('',(1.,0.,2.40370335797945E-16));
#31034=DIRECTION('',(0.,-1.,0.));
#31035=DIRECTION('',(-1.,0.,-2.40370335797945E-16));
#31036=DIRECTION('center_axis',(0.866025403784439,0.,0.5));
#31037=DIRECTION('ref_axis',(-0.5,0.,0.866025403784439));
#31038=DIRECTION('',(0.5,0.,-0.866025403784439));
#31039=DIRECTION('',(-0.5,0.,0.866025403784439));
#31040=DIRECTION('center_axis',(0.,1.,0.));
#31041=DIRECTION('ref_axis',(1.,0.,0.));
#31042=DIRECTION('center_axis',(0.,-1.,0.));
#31043=DIRECTION('ref_axis',(0.,0.,-1.));
#31044=DIRECTION('center_axis',(0.,1.,0.));
#31045=DIRECTION('ref_axis',(1.,0.,0.));
#31046=DIRECTION('center_axis',(0.,1.,0.));
#31047=DIRECTION('ref_axis',(1.,0.,0.));
#31048=DIRECTION('center_axis',(0.,1.,0.));
#31049=DIRECTION('ref_axis',(0.,0.,1.));
#31050=DIRECTION('center_axis',(0.,-1.,0.));
#31051=DIRECTION('ref_axis',(1.,0.,0.));
#31052=DIRECTION('center_axis',(0.,-1.,0.));
#31053=DIRECTION('ref_axis',(1.,0.,0.));
#31054=DIRECTION('center_axis',(0.,-1.,0.));
#31055=DIRECTION('ref_axis',(1.,0.,0.));
#31056=DIRECTION('',(0.707106781186548,0.707106781186547,8.65956056235493E-17));
#31057=DIRECTION('center_axis',(0.,-1.,0.));
#31058=DIRECTION('ref_axis',(1.,0.,0.));
#31059=DIRECTION('center_axis',(0.,-1.,0.));
#31060=DIRECTION('ref_axis',(1.,0.,0.));
#31061=DIRECTION('',(0.,1.,0.));
#31062=DIRECTION('center_axis',(0.,1.,0.));
#31063=DIRECTION('ref_axis',(1.,0.,0.));
#31064=DIRECTION('center_axis',(0.,-1.,0.));
#31065=DIRECTION('ref_axis',(1.,0.,0.));
#31066=DIRECTION('',(-0.707106781186547,0.707106781186548,-8.65956056235493E-17));
#31067=DIRECTION('center_axis',(0.,-1.,0.));
#31068=DIRECTION('ref_axis',(0.,0.,-1.));
#31069=DIRECTION('center_axis',(0.,-1.,0.));
#31070=DIRECTION('ref_axis',(1.,0.,0.));
#31071=DIRECTION('center_axis',(0.,1.,0.));
#31072=DIRECTION('ref_axis',(1.,0.,0.));
#31073=DIRECTION('center_axis',(0.,1.,0.));
#31074=DIRECTION('ref_axis',(1.,0.,0.));
#31075=DIRECTION('',(-0.447213595499958,0.894427190999916,-5.47678698264203E-17));
#31076=DIRECTION('center_axis',(0.,-1.,0.));
#31077=DIRECTION('ref_axis',(1.,0.,0.));
#31078=DIRECTION('',(0.,1.,0.));
#31079=DIRECTION('axis',(0.,0.,1.));
#31080=DIRECTION('refdir',(1.,0.,0.));
#31081=DIRECTION('axis',(0.,0.,1.));
#31082=DIRECTION('refdir',(1.,0.,0.));
#31083=DIRECTION('center_axis',(0.,0.,1.));
#31084=DIRECTION('ref_axis',(1.,0.,0.));
#31085=DIRECTION('center_axis',(0.,0.,1.));
#31086=DIRECTION('ref_axis',(1.,0.,0.));
#31087=DIRECTION('',(0.,0.,1.));
#31088=DIRECTION('center_axis',(0.,0.,-1.));
#31089=DIRECTION('ref_axis',(1.,0.,0.));
#31090=DIRECTION('center_axis',(0.,0.,1.));
#31091=DIRECTION('ref_axis',(1.,0.,0.));
#31092=DIRECTION('center_axis',(0.,0.,1.));
#31093=DIRECTION('ref_axis',(1.,0.,0.));
#31094=DIRECTION('',(0.,0.,1.));
#31095=DIRECTION('center_axis',(0.,0.,-1.));
#31096=DIRECTION('ref_axis',(1.,0.,0.));
#31097=DIRECTION('center_axis',(0.,0.,1.));
#31098=DIRECTION('ref_axis',(1.,0.,0.));
#31099=DIRECTION('center_axis',(0.,0.,1.));
#31100=DIRECTION('ref_axis',(1.,0.,0.));
#31101=DIRECTION('',(0.,0.,1.));
#31102=DIRECTION('center_axis',(0.,0.,-1.));
#31103=DIRECTION('ref_axis',(1.,0.,0.));
#31104=DIRECTION('center_axis',(0.,0.,1.));
#31105=DIRECTION('ref_axis',(1.,0.,0.));
#31106=DIRECTION('center_axis',(0.,0.,1.));
#31107=DIRECTION('ref_axis',(1.,0.,0.));
#31108=DIRECTION('',(0.,0.,1.));
#31109=DIRECTION('center_axis',(0.,0.,-1.));
#31110=DIRECTION('ref_axis',(1.,0.,0.));
#31111=DIRECTION('center_axis',(0.,1.,0.));
#31112=DIRECTION('ref_axis',(-1.,0.,0.));
#31113=DIRECTION('',(-1.,0.,0.));
#31114=DIRECTION('',(0.,0.,1.));
#31115=DIRECTION('',(-1.,0.,0.));
#31116=DIRECTION('',(0.,0.,1.));
#31117=DIRECTION('center_axis',(1.,0.,0.));
#31118=DIRECTION('ref_axis',(0.,1.,0.));
#31119=DIRECTION('',(0.,1.,0.));
#31120=DIRECTION('',(0.,1.,0.));
#31121=DIRECTION('',(0.,0.,1.));
#31122=DIRECTION('center_axis',(0.,-1.,0.));
#31123=DIRECTION('ref_axis',(1.,0.,0.));
#31124=DIRECTION('',(1.,0.,0.));
#31125=DIRECTION('',(1.,0.,0.));
#31126=DIRECTION('',(0.,0.,1.));
#31127=DIRECTION('center_axis',(-1.,0.,0.));
#31128=DIRECTION('ref_axis',(0.,-1.,0.));
#31129=DIRECTION('',(0.,-1.,0.));
#31130=DIRECTION('',(0.,-1.,0.));
#31131=DIRECTION('center_axis',(0.,0.,1.));
#31132=DIRECTION('ref_axis',(1.,0.,0.));
#31133=DIRECTION('center_axis',(0.,0.,1.));
#31134=DIRECTION('ref_axis',(1.,0.,0.));
#31135=DIRECTION('axis',(0.,0.,1.));
#31136=DIRECTION('refdir',(1.,0.,0.));
#31137=DIRECTION('center_axis',(0.,0.,1.));
#31138=DIRECTION('ref_axis',(1.,0.,0.));
#31139=DIRECTION('center_axis',(0.,0.,1.));
#31140=DIRECTION('ref_axis',(1.,0.,0.));
#31141=DIRECTION('',(0.,0.,1.));
#31142=DIRECTION('center_axis',(0.,0.,-1.));
#31143=DIRECTION('ref_axis',(1.,0.,0.));
#31144=DIRECTION('center_axis',(0.,0.,1.));
#31145=DIRECTION('ref_axis',(1.,0.,0.));
#31146=DIRECTION('center_axis',(0.,0.,1.));
#31147=DIRECTION('ref_axis',(1.,0.,0.));
#31148=DIRECTION('',(0.,0.,1.));
#31149=DIRECTION('center_axis',(0.,0.,-1.));
#31150=DIRECTION('ref_axis',(1.,0.,0.));
#31151=DIRECTION('center_axis',(0.,0.,1.));
#31152=DIRECTION('ref_axis',(1.,0.,0.));
#31153=DIRECTION('center_axis',(0.,0.,1.));
#31154=DIRECTION('ref_axis',(1.,0.,0.));
#31155=DIRECTION('',(0.,0.,1.));
#31156=DIRECTION('center_axis',(0.,0.,-1.));
#31157=DIRECTION('ref_axis',(1.,0.,0.));
#31158=DIRECTION('center_axis',(0.,0.,1.));
#31159=DIRECTION('ref_axis',(1.,0.,0.));
#31160=DIRECTION('center_axis',(0.,0.,1.));
#31161=DIRECTION('ref_axis',(1.,0.,0.));
#31162=DIRECTION('',(0.,0.,1.));
#31163=DIRECTION('center_axis',(0.,0.,-1.));
#31164=DIRECTION('ref_axis',(1.,0.,0.));
#31165=DIRECTION('center_axis',(0.,0.,1.));
#31166=DIRECTION('ref_axis',(1.,0.,0.));
#31167=DIRECTION('center_axis',(0.,0.,1.));
#31168=DIRECTION('ref_axis',(1.,0.,0.));
#31169=DIRECTION('',(0.,0.,1.));
#31170=DIRECTION('center_axis',(0.,0.,-1.));
#31171=DIRECTION('ref_axis',(1.,0.,0.));
#31172=DIRECTION('center_axis',(0.,0.,1.));
#31173=DIRECTION('ref_axis',(1.,0.,0.));
#31174=DIRECTION('center_axis',(0.,0.,1.));
#31175=DIRECTION('ref_axis',(1.,0.,0.));
#31176=DIRECTION('',(0.,0.,1.));
#31177=DIRECTION('center_axis',(0.,0.,-1.));
#31178=DIRECTION('ref_axis',(1.,0.,0.));
#31179=DIRECTION('center_axis',(0.,0.,1.));
#31180=DIRECTION('ref_axis',(1.,0.,0.));
#31181=DIRECTION('center_axis',(0.,0.,1.));
#31182=DIRECTION('ref_axis',(1.,0.,0.));
#31183=DIRECTION('',(0.,0.,1.));
#31184=DIRECTION('center_axis',(0.,0.,-1.));
#31185=DIRECTION('ref_axis',(1.,0.,0.));
#31186=DIRECTION('center_axis',(0.,0.,1.));
#31187=DIRECTION('ref_axis',(1.,0.,0.));
#31188=DIRECTION('center_axis',(0.,0.,1.));
#31189=DIRECTION('ref_axis',(1.,0.,0.));
#31190=DIRECTION('',(0.,0.,1.));
#31191=DIRECTION('center_axis',(0.,0.,-1.));
#31192=DIRECTION('ref_axis',(1.,0.,0.));
#31193=DIRECTION('center_axis',(0.,1.,0.));
#31194=DIRECTION('ref_axis',(-1.,0.,0.));
#31195=DIRECTION('',(-1.,0.,0.));
#31196=DIRECTION('',(0.,0.,1.));
#31197=DIRECTION('',(-1.,0.,0.));
#31198=DIRECTION('',(0.,0.,1.));
#31199=DIRECTION('center_axis',(1.,0.,0.));
#31200=DIRECTION('ref_axis',(0.,1.,0.));
#31201=DIRECTION('',(0.,1.,0.));
#31202=DIRECTION('',(0.,1.,0.));
#31203=DIRECTION('',(0.,0.,1.));
#31204=DIRECTION('center_axis',(0.,-1.,0.));
#31205=DIRECTION('ref_axis',(1.,0.,0.));
#31206=DIRECTION('',(1.,0.,0.));
#31207=DIRECTION('',(1.,0.,0.));
#31208=DIRECTION('',(0.,0.,1.));
#31209=DIRECTION('center_axis',(-1.,0.,0.));
#31210=DIRECTION('ref_axis',(0.,-1.,0.));
#31211=DIRECTION('',(0.,-1.,0.));
#31212=DIRECTION('',(0.,-1.,0.));
#31213=DIRECTION('center_axis',(0.,0.,1.));
#31214=DIRECTION('ref_axis',(1.,0.,0.));
#31215=DIRECTION('center_axis',(0.,0.,1.));
#31216=DIRECTION('ref_axis',(1.,0.,0.));
#31217=DIRECTION('axis',(0.,0.,1.));
#31218=DIRECTION('refdir',(1.,0.,0.));
#31219=DIRECTION('center_axis',(0.,0.,1.));
#31220=DIRECTION('ref_axis',(1.,0.,0.));
#31221=DIRECTION('center_axis',(0.,0.,1.));
#31222=DIRECTION('ref_axis',(1.,0.,0.));
#31223=DIRECTION('',(0.,0.,1.));
#31224=DIRECTION('center_axis',(0.,0.,-1.));
#31225=DIRECTION('ref_axis',(1.,0.,0.));
#31226=DIRECTION('center_axis',(0.,0.,1.));
#31227=DIRECTION('ref_axis',(1.,0.,0.));
#31228=DIRECTION('center_axis',(0.,0.,1.));
#31229=DIRECTION('ref_axis',(1.,0.,0.));
#31230=DIRECTION('center_axis',(0.,0.,1.));
#31231=DIRECTION('ref_axis',(1.,0.,0.));
#31232=DIRECTION('',(0.,0.,1.));
#31233=DIRECTION('center_axis',(0.,0.,-1.));
#31234=DIRECTION('ref_axis',(1.,0.,0.));
#31235=DIRECTION('center_axis',(0.,0.,1.));
#31236=DIRECTION('ref_axis',(1.,0.,0.));
#31237=DIRECTION('center_axis',(0.,0.,1.));
#31238=DIRECTION('ref_axis',(1.,0.,0.));
#31239=DIRECTION('center_axis',(0.,0.,1.));
#31240=DIRECTION('ref_axis',(1.,0.,0.));
#31241=DIRECTION('',(0.,0.,1.));
#31242=DIRECTION('center_axis',(0.,0.,-1.));
#31243=DIRECTION('ref_axis',(1.,0.,0.));
#31244=DIRECTION('center_axis',(0.,0.,1.));
#31245=DIRECTION('ref_axis',(1.,0.,0.));
#31246=DIRECTION('center_axis',(0.,0.,1.));
#31247=DIRECTION('ref_axis',(1.,0.,0.));
#31248=DIRECTION('center_axis',(0.,0.,1.));
#31249=DIRECTION('ref_axis',(1.,0.,0.));
#31250=DIRECTION('',(0.,0.,1.));
#31251=DIRECTION('center_axis',(0.,0.,-1.));
#31252=DIRECTION('ref_axis',(1.,0.,0.));
#31253=DIRECTION('center_axis',(0.,0.,1.));
#31254=DIRECTION('ref_axis',(1.,0.,0.));
#31255=DIRECTION('center_axis',(1.,0.,0.));
#31256=DIRECTION('ref_axis',(0.,0.,-1.));
#31257=DIRECTION('center_axis',(1.,0.,0.));
#31258=DIRECTION('ref_axis',(0.,0.,-1.));
#31259=DIRECTION('',(1.,0.,0.));
#31260=DIRECTION('center_axis',(-1.,0.,0.));
#31261=DIRECTION('ref_axis',(0.,0.,-1.));
#31262=DIRECTION('center_axis',(1.,0.,0.));
#31263=DIRECTION('ref_axis',(0.,0.,-1.));
#31264=DIRECTION('center_axis',(1.,0.,0.));
#31265=DIRECTION('ref_axis',(0.,0.,-1.));
#31266=DIRECTION('center_axis',(1.,0.,0.));
#31267=DIRECTION('ref_axis',(0.,0.,-1.));
#31268=DIRECTION('',(1.,0.,0.));
#31269=DIRECTION('center_axis',(-1.,0.,0.));
#31270=DIRECTION('ref_axis',(0.,0.,-1.));
#31271=DIRECTION('center_axis',(1.,0.,0.));
#31272=DIRECTION('ref_axis',(0.,0.,-1.));
#31273=DIRECTION('center_axis',(1.,0.,0.));
#31274=DIRECTION('ref_axis',(0.,0.,-1.));
#31275=DIRECTION('center_axis',(1.,0.,0.));
#31276=DIRECTION('ref_axis',(0.,0.,-1.));
#31277=DIRECTION('',(1.,0.,0.));
#31278=DIRECTION('center_axis',(-1.,0.,0.));
#31279=DIRECTION('ref_axis',(0.,0.,-1.));
#31280=DIRECTION('center_axis',(1.,0.,0.));
#31281=DIRECTION('ref_axis',(0.,0.,-1.));
#31282=DIRECTION('center_axis',(1.,0.,0.));
#31283=DIRECTION('ref_axis',(0.,0.,-1.));
#31284=DIRECTION('center_axis',(1.,0.,0.));
#31285=DIRECTION('ref_axis',(0.,0.,-1.));
#31286=DIRECTION('',(1.,0.,0.));
#31287=DIRECTION('center_axis',(-1.,0.,0.));
#31288=DIRECTION('ref_axis',(0.,0.,-1.));
#31289=DIRECTION('center_axis',(0.,1.,0.));
#31290=DIRECTION('ref_axis',(-1.,0.,0.));
#31291=DIRECTION('',(-1.,0.,0.));
#31292=DIRECTION('',(0.,0.,1.));
#31293=DIRECTION('',(-1.,0.,0.));
#31294=DIRECTION('',(0.,0.,1.));
#31295=DIRECTION('center_axis',(1.,0.,0.));
#31296=DIRECTION('ref_axis',(0.,1.,0.));
#31297=DIRECTION('',(0.,1.,0.));
#31298=DIRECTION('',(0.,1.,0.));
#31299=DIRECTION('',(0.,0.,1.));
#31300=DIRECTION('center_axis',(0.,-1.,0.));
#31301=DIRECTION('ref_axis',(1.,0.,0.));
#31302=DIRECTION('',(1.,0.,0.));
#31303=DIRECTION('',(1.,0.,0.));
#31304=DIRECTION('',(0.,0.,1.));
#31305=DIRECTION('center_axis',(-1.,0.,0.));
#31306=DIRECTION('ref_axis',(0.,-1.,0.));
#31307=DIRECTION('',(0.,-1.,0.));
#31308=DIRECTION('',(0.,-1.,0.));
#31309=DIRECTION('center_axis',(0.,0.,1.));
#31310=DIRECTION('ref_axis',(1.,0.,0.));
#31311=DIRECTION('center_axis',(0.,0.,1.));
#31312=DIRECTION('ref_axis',(1.,0.,0.));
#31313=DIRECTION('axis',(0.,0.,1.));
#31314=DIRECTION('refdir',(1.,0.,0.));
#31315=DIRECTION('axis',(0.,0.,1.));
#31316=DIRECTION('refdir',(1.,0.,0.));
#31317=DIRECTION('center_axis',(0.,0.,1.));
#31318=DIRECTION('ref_axis',(1.,0.,0.));
#31319=DIRECTION('',(-1.,0.,0.));
#31320=DIRECTION('center_axis',(0.,0.,1.));
#31321=DIRECTION('ref_axis',(1.,0.,0.));
#31322=DIRECTION('center_axis',(0.,0.,1.));
#31323=DIRECTION('ref_axis',(1.,0.,0.));
#31324=DIRECTION('',(0.,0.,-1.));
#31325=DIRECTION('center_axis',(0.,0.,1.));
#31326=DIRECTION('ref_axis',(1.,0.,0.));
#31327=DIRECTION('',(0.,0.,1.));
#31328=DIRECTION('center_axis',(0.,0.,-1.));
#31329=DIRECTION('ref_axis',(1.,0.,0.));
#31330=DIRECTION('center_axis',(0.,0.,1.));
#31331=DIRECTION('ref_axis',(1.,0.,0.));
#31332=DIRECTION('',(0.,0.,1.));
#31333=DIRECTION('center_axis',(0.,0.,1.));
#31334=DIRECTION('ref_axis',(1.,0.,0.));
#31335=DIRECTION('',(1.,0.,0.));
#31336=DIRECTION('center_axis',(0.,0.,1.));
#31337=DIRECTION('ref_axis',(1.,0.,0.));
#31338=DIRECTION('center_axis',(0.,0.,1.));
#31339=DIRECTION('ref_axis',(1.,0.,0.));
#31340=DIRECTION('',(0.,0.,-1.));
#31341=DIRECTION('center_axis',(0.,0.,1.));
#31342=DIRECTION('ref_axis',(1.,0.,0.));
#31343=DIRECTION('',(0.,0.,1.));
#31344=DIRECTION('center_axis',(0.,0.,-1.));
#31345=DIRECTION('ref_axis',(1.,0.,0.));
#31346=DIRECTION('center_axis',(0.,0.,1.));
#31347=DIRECTION('ref_axis',(1.,0.,0.));
#31348=DIRECTION('',(0.,0.,1.));
#31349=DIRECTION('center_axis',(0.,0.,1.));
#31350=DIRECTION('ref_axis',(1.,0.,0.));
#31351=DIRECTION('',(-1.,0.,0.));
#31352=DIRECTION('center_axis',(0.,0.,1.));
#31353=DIRECTION('ref_axis',(1.,0.,0.));
#31354=DIRECTION('center_axis',(0.,0.,1.));
#31355=DIRECTION('ref_axis',(1.,0.,0.));
#31356=DIRECTION('',(0.,0.,-1.));
#31357=DIRECTION('center_axis',(0.,0.,1.));
#31358=DIRECTION('ref_axis',(1.,0.,0.));
#31359=DIRECTION('',(0.,0.,1.));
#31360=DIRECTION('center_axis',(0.,0.,-1.));
#31361=DIRECTION('ref_axis',(1.,0.,0.));
#31362=DIRECTION('center_axis',(0.,0.,1.));
#31363=DIRECTION('ref_axis',(1.,0.,0.));
#31364=DIRECTION('',(0.,0.,1.));
#31365=DIRECTION('center_axis',(0.,0.,1.));
#31366=DIRECTION('ref_axis',(1.,0.,0.));
#31367=DIRECTION('',(1.,0.,0.));
#31368=DIRECTION('center_axis',(0.,0.,1.));
#31369=DIRECTION('ref_axis',(1.,0.,0.));
#31370=DIRECTION('center_axis',(0.,0.,1.));
#31371=DIRECTION('ref_axis',(1.,0.,0.));
#31372=DIRECTION('',(0.,0.,-1.));
#31373=DIRECTION('center_axis',(0.,0.,1.));
#31374=DIRECTION('ref_axis',(1.,0.,0.));
#31375=DIRECTION('',(0.,0.,1.));
#31376=DIRECTION('center_axis',(0.,0.,-1.));
#31377=DIRECTION('ref_axis',(1.,0.,0.));
#31378=DIRECTION('center_axis',(0.,0.,1.));
#31379=DIRECTION('ref_axis',(1.,0.,0.));
#31380=DIRECTION('',(0.,0.,1.));
#31381=DIRECTION('center_axis',(0.,-1.,0.));
#31382=DIRECTION('ref_axis',(0.,0.,-1.));
#31383=DIRECTION('',(-1.,0.,0.));
#31384=DIRECTION('',(-1.,0.,0.));
#31385=DIRECTION('',(0.,0.,1.));
#31386=DIRECTION('',(1.,0.,0.));
#31387=DIRECTION('',(0.,0.,-1.));
#31388=DIRECTION('',(-1.,0.,0.));
#31389=DIRECTION('center_axis',(0.,1.,0.));
#31390=DIRECTION('ref_axis',(0.,0.,1.));
#31391=DIRECTION('',(1.,0.,0.));
#31392=DIRECTION('',(1.,0.,0.));
#31393=DIRECTION('',(0.,0.,1.));
#31394=DIRECTION('',(1.,0.,0.));
#31395=DIRECTION('',(0.,0.,-1.));
#31396=DIRECTION('',(1.,0.,0.));
#31397=DIRECTION('center_axis',(-1.,0.,0.));
#31398=DIRECTION('ref_axis',(0.,0.,1.));
#31399=DIRECTION('',(0.,-1.,0.));
#31400=DIRECTION('',(0.,0.,1.));
#31401=DIRECTION('',(0.,1.,0.));
#31402=DIRECTION('',(0.,0.,-1.));
#31403=DIRECTION('',(0.,-1.,0.));
#31404=DIRECTION('',(0.,-1.,0.));
#31405=DIRECTION('',(0.,0.,1.));
#31406=DIRECTION('',(0.,-1.,0.));
#31407=DIRECTION('',(0.,0.,-1.));
#31408=DIRECTION('',(0.,-1.,0.));
#31409=DIRECTION('center_axis',(0.,0.,-1.));
#31410=DIRECTION('ref_axis',(0.,1.,0.));
#31411=DIRECTION('',(0.,1.,0.));
#31412=DIRECTION('',(1.,0.,0.));
#31413=DIRECTION('center_axis',(0.,-1.,0.));
#31414=DIRECTION('ref_axis',(0.,0.,-1.));
#31415=DIRECTION('',(0.,0.,-1.));
#31416=DIRECTION('',(1.,0.,0.));
#31417=DIRECTION('center_axis',(0.,0.,1.));
#31418=DIRECTION('ref_axis',(0.,-1.,0.));
#31419=DIRECTION('',(0.,-1.,0.));
#31420=DIRECTION('',(1.,0.,0.));
#31421=DIRECTION('center_axis',(0.,1.,0.));
#31422=DIRECTION('ref_axis',(0.,0.,1.));
#31423=DIRECTION('',(0.,0.,1.));
#31424=DIRECTION('',(1.,0.,0.));
#31425=DIRECTION('center_axis',(0.,0.,-1.));
#31426=DIRECTION('ref_axis',(0.,1.,0.));
#31427=DIRECTION('',(0.,1.,0.));
#31428=DIRECTION('center_axis',(0.,0.,-1.));
#31429=DIRECTION('ref_axis',(0.,1.,0.));
#31430=DIRECTION('',(0.,1.,0.));
#31431=DIRECTION('',(1.,0.,0.));
#31432=DIRECTION('center_axis',(0.,-1.,0.));
#31433=DIRECTION('ref_axis',(0.,0.,-1.));
#31434=DIRECTION('',(0.,0.,-1.));
#31435=DIRECTION('',(1.,0.,0.));
#31436=DIRECTION('center_axis',(0.,0.,-1.));
#31437=DIRECTION('ref_axis',(0.,1.,0.));
#31438=DIRECTION('',(0.,1.,0.));
#31439=DIRECTION('',(1.,0.,0.));
#31440=DIRECTION('center_axis',(0.,1.,0.));
#31441=DIRECTION('ref_axis',(0.,0.,1.));
#31442=DIRECTION('',(0.,0.,1.));
#31443=DIRECTION('',(1.,0.,0.));
#31444=DIRECTION('center_axis',(0.,0.,-1.));
#31445=DIRECTION('ref_axis',(0.,1.,0.));
#31446=DIRECTION('',(0.,1.,0.));
#31447=DIRECTION('center_axis',(1.,0.,0.));
#31448=DIRECTION('ref_axis',(0.,0.,-1.));
#31449=DIRECTION('axis',(0.,0.,1.));
#31450=DIRECTION('refdir',(1.,0.,0.));
#31451=DIRECTION('center_axis',(0.,0.,1.));
#31452=DIRECTION('ref_axis',(0.,-1.,0.));
#31453=DIRECTION('',(0.,-1.,0.));
#31454=DIRECTION('',(1.,0.,0.));
#31455=DIRECTION('',(0.,-1.,0.));
#31456=DIRECTION('',(1.,0.,0.));
#31457=DIRECTION('center_axis',(0.,1.,0.));
#31458=DIRECTION('ref_axis',(0.,0.,1.));
#31459=DIRECTION('',(0.,0.,1.));
#31460=DIRECTION('',(0.,0.,1.));
#31461=DIRECTION('',(1.,0.,0.));
#31462=DIRECTION('center_axis',(0.,0.,-1.));
#31463=DIRECTION('ref_axis',(0.,1.,0.));
#31464=DIRECTION('',(0.,1.,0.));
#31465=DIRECTION('',(0.,1.,0.));
#31466=DIRECTION('',(1.,0.,0.));
#31467=DIRECTION('center_axis',(0.,-1.,0.));
#31468=DIRECTION('ref_axis',(0.,0.,-1.));
#31469=DIRECTION('',(0.,0.,-1.));
#31470=DIRECTION('',(0.,0.,-1.));
#31471=DIRECTION('',(1.,0.,0.));
#31472=DIRECTION('center_axis',(0.,0.,-1.));
#31473=DIRECTION('ref_axis',(0.,1.,0.));
#31474=DIRECTION('',(0.,1.,0.));
#31475=DIRECTION('',(0.,1.,0.));
#31476=DIRECTION('',(1.,0.,0.));
#31477=DIRECTION('center_axis',(0.,1.,0.));
#31478=DIRECTION('ref_axis',(0.,0.,1.));
#31479=DIRECTION('',(0.,0.,1.));
#31480=DIRECTION('',(0.,0.,1.));
#31481=DIRECTION('',(1.,0.,0.));
#31482=DIRECTION('center_axis',(0.,0.,-1.));
#31483=DIRECTION('ref_axis',(0.,1.,0.));
#31484=DIRECTION('',(0.,1.,0.));
#31485=DIRECTION('',(0.,1.,0.));
#31486=DIRECTION('',(1.,0.,0.));
#31487=DIRECTION('center_axis',(0.,-1.,0.));
#31488=DIRECTION('ref_axis',(0.,0.,-1.));
#31489=DIRECTION('',(0.,0.,-1.));
#31490=DIRECTION('',(0.,0.,-1.));
#31491=DIRECTION('center_axis',(1.,0.,0.));
#31492=DIRECTION('ref_axis',(0.,0.,-1.));
#31493=DIRECTION('center_axis',(1.,0.,0.));
#31494=DIRECTION('ref_axis',(0.,0.,-1.));
#31495=DIRECTION('axis',(0.,0.,1.));
#31496=DIRECTION('refdir',(1.,0.,0.));
#31497=DIRECTION('center_axis',(0.,0.,-1.));
#31498=DIRECTION('ref_axis',(0.,-1.,0.));
#31499=DIRECTION('',(0.,1.,0.));
#31500=DIRECTION('',(-1.,0.,0.));
#31501=DIRECTION('',(0.,-1.,0.));
#31502=DIRECTION('',(-1.,0.,0.));
#31503=DIRECTION('center_axis',(0.,1.,0.));
#31504=DIRECTION('ref_axis',(0.,0.,-1.));
#31505=DIRECTION('',(0.,0.,1.));
#31506=DIRECTION('',(0.,0.,-1.));
#31507=DIRECTION('',(-1.,0.,0.));
#31508=DIRECTION('center_axis',(0.,0.,-1.));
#31509=DIRECTION('ref_axis',(0.,-1.,0.));
#31510=DIRECTION('',(0.,1.,0.));
#31511=DIRECTION('',(0.,-1.,0.));
#31512=DIRECTION('',(-1.,0.,0.));
#31513=DIRECTION('center_axis',(0.,-1.,0.));
#31514=DIRECTION('ref_axis',(0.,0.,1.));
#31515=DIRECTION('',(0.,0.,-1.));
#31516=DIRECTION('',(0.,0.,1.));
#31517=DIRECTION('',(-1.,0.,0.));
#31518=DIRECTION('center_axis',(0.,0.,-1.));
#31519=DIRECTION('ref_axis',(0.,-1.,0.));
#31520=DIRECTION('',(0.,1.,0.));
#31521=DIRECTION('',(0.,-1.,0.));
#31522=DIRECTION('',(-1.,0.,0.));
#31523=DIRECTION('center_axis',(0.,1.,0.));
#31524=DIRECTION('ref_axis',(0.,0.,-1.));
#31525=DIRECTION('',(0.,0.,1.));
#31526=DIRECTION('',(0.,0.,-1.));
#31527=DIRECTION('',(-1.,0.,0.));
#31528=DIRECTION('center_axis',(0.,0.,1.));
#31529=DIRECTION('ref_axis',(0.,1.,0.));
#31530=DIRECTION('',(0.,-1.,0.));
#31531=DIRECTION('',(0.,1.,0.));
#31532=DIRECTION('',(-1.,0.,0.));
#31533=DIRECTION('center_axis',(0.,-1.,0.));
#31534=DIRECTION('ref_axis',(0.,0.,1.));
#31535=DIRECTION('',(0.,0.,-1.));
#31536=DIRECTION('',(0.,0.,1.));
#31537=DIRECTION('center_axis',(1.,0.,0.));
#31538=DIRECTION('ref_axis',(0.,0.,-1.));
#31539=DIRECTION('center_axis',(-1.,0.,0.));
#31540=DIRECTION('ref_axis',(0.,0.,1.));
#31541=DIRECTION('',(0.,0.,1.));
#31542=DIRECTION('',(1.,0.,0.));
#31543=DIRECTION('',(0.,0.,1.));
#31544=DIRECTION('',(1.,0.,0.));
#31545=DIRECTION('',(0.,0.,1.));
#31546=DIRECTION('',(1.,0.,0.));
#31547=DIRECTION('axis',(0.,0.,1.));
#31548=DIRECTION('refdir',(1.,0.,0.));
#31549=DIRECTION('center_axis',(0.,1.,0.));
#31550=DIRECTION('ref_axis',(1.,0.,0.));
#31551=DIRECTION('center_axis',(0.,1.,0.));
#31552=DIRECTION('ref_axis',(1.,0.,0.));
#31553=DIRECTION('',(0.707106781186548,-0.707106781186547,-8.65956056235494E-17));
#31554=DIRECTION('center_axis',(0.,-1.,0.));
#31555=DIRECTION('ref_axis',(1.,0.,0.));
#31556=DIRECTION('center_axis',(0.,1.,0.));
#31557=DIRECTION('ref_axis',(1.,0.,0.));
#31558=DIRECTION('',(0.,-1.,0.));
#31559=DIRECTION('center_axis',(0.,-1.,0.));
#31560=DIRECTION('ref_axis',(1.,0.,0.));
#31561=DIRECTION('center_axis',(0.,1.,0.));
#31562=DIRECTION('ref_axis',(1.,0.,0.));
#31563=DIRECTION('center_axis',(0.,1.,0.));
#31564=DIRECTION('ref_axis',(1.,0.,0.));
#31565=DIRECTION('center_axis',(0.,1.,0.));
#31566=DIRECTION('ref_axis',(1.,0.,0.));
#31567=DIRECTION('',(0.,-1.,0.));
#31568=DIRECTION('center_axis',(0.,1.,0.));
#31569=DIRECTION('ref_axis',(1.,0.,0.));
#31570=DIRECTION('center_axis',(0.,1.,0.));
#31571=DIRECTION('ref_axis',(1.,0.,0.));
#31572=DIRECTION('axis',(0.,0.,1.));
#31573=DIRECTION('refdir',(1.,0.,0.));
#31574=DIRECTION('center_axis',(0.866025403784439,0.,-0.5));
#31575=DIRECTION('ref_axis',(0.5,0.,0.866025403784439));
#31576=DIRECTION('',(-0.5,0.,-0.866025403784439));
#31577=DIRECTION('',(0.,-1.,0.));
#31578=DIRECTION('',(0.5,0.,0.866025403784439));
#31579=DIRECTION('',(0.,-1.,0.));
#31580=DIRECTION('center_axis',(1.20185167898973E-16,0.,-1.));
#31581=DIRECTION('ref_axis',(1.,0.,1.20185167898973E-16));
#31582=DIRECTION('',(-1.,0.,-1.20185167898973E-16));
#31583=DIRECTION('',(0.,-1.,0.));
#31584=DIRECTION('',(1.,0.,1.20185167898973E-16));
#31585=DIRECTION('center_axis',(-0.866025403784439,0.,-0.5));
#31586=DIRECTION('ref_axis',(0.5,0.,-0.866025403784439));
#31587=DIRECTION('',(-0.5,0.,0.866025403784439));
#31588=DIRECTION('',(0.,-1.,0.));
#31589=DIRECTION('',(0.5,0.,-0.866025403784439));
#31590=DIRECTION('center_axis',(-0.866025403784439,0.,0.5));
#31591=DIRECTION('ref_axis',(-0.5,0.,-0.866025403784439));
#31592=DIRECTION('',(0.5,0.,0.866025403784439));
#31593=DIRECTION('',(0.,-1.,0.));
#31594=DIRECTION('',(-0.5,0.,-0.866025403784439));
#31595=DIRECTION('center_axis',(-2.40370335797945E-16,0.,1.));
#31596=DIRECTION('ref_axis',(-1.,0.,-2.40370335797945E-16));
#31597=DIRECTION('',(1.,0.,2.40370335797945E-16));
#31598=DIRECTION('',(0.,-1.,0.));
#31599=DIRECTION('',(-1.,0.,-2.40370335797945E-16));
#31600=DIRECTION('center_axis',(0.866025403784439,0.,0.5));
#31601=DIRECTION('ref_axis',(-0.5,0.,0.866025403784439));
#31602=DIRECTION('',(0.5,0.,-0.866025403784439));
#31603=DIRECTION('',(-0.5,0.,0.866025403784439));
#31604=DIRECTION('center_axis',(0.,1.,0.));
#31605=DIRECTION('ref_axis',(1.,0.,0.));
#31606=DIRECTION('center_axis',(0.,-1.,0.));
#31607=DIRECTION('ref_axis',(0.,0.,-1.));
#31608=DIRECTION('center_axis',(0.,1.,0.));
#31609=DIRECTION('ref_axis',(1.,0.,0.));
#31610=DIRECTION('center_axis',(0.,1.,0.));
#31611=DIRECTION('ref_axis',(1.,0.,0.));
#31612=DIRECTION('center_axis',(0.,1.,0.));
#31613=DIRECTION('ref_axis',(1.,0.,0.));
#31614=DIRECTION('center_axis',(0.,1.,0.));
#31615=DIRECTION('ref_axis',(1.,0.,0.));
#31616=DIRECTION('',(0.,-1.,0.));
#31617=DIRECTION('center_axis',(0.,1.,0.));
#31618=DIRECTION('ref_axis',(1.,0.,0.));
#31619=DIRECTION('center_axis',(0.,1.,0.));
#31620=DIRECTION('ref_axis',(1.,0.,0.));
#31621=DIRECTION('center_axis',(0.,1.,0.));
#31622=DIRECTION('ref_axis',(0.,0.,1.));
#31623=DIRECTION('center_axis',(0.,-1.,0.));
#31624=DIRECTION('ref_axis',(1.,0.,0.));
#31625=DIRECTION('center_axis',(0.,-1.,0.));
#31626=DIRECTION('ref_axis',(1.,0.,0.));
#31627=DIRECTION('center_axis',(0.,-1.,0.));
#31628=DIRECTION('ref_axis',(1.,0.,0.));
#31629=DIRECTION('',(0.707106781186548,0.707106781186547,8.65956056235493E-17));
#31630=DIRECTION('center_axis',(0.,-1.,0.));
#31631=DIRECTION('ref_axis',(1.,0.,0.));
#31632=DIRECTION('center_axis',(0.,-1.,0.));
#31633=DIRECTION('ref_axis',(1.,0.,0.));
#31634=DIRECTION('',(0.,1.,0.));
#31635=DIRECTION('center_axis',(0.,1.,0.));
#31636=DIRECTION('ref_axis',(1.,0.,0.));
#31637=DIRECTION('center_axis',(0.,-1.,0.));
#31638=DIRECTION('ref_axis',(1.,0.,0.));
#31639=DIRECTION('',(-0.707106781186547,0.707106781186548,-8.65956056235493E-17));
#31640=DIRECTION('center_axis',(0.,-1.,0.));
#31641=DIRECTION('ref_axis',(0.,0.,-1.));
#31642=DIRECTION('center_axis',(0.,-1.,0.));
#31643=DIRECTION('ref_axis',(1.,0.,0.));
#31644=DIRECTION('center_axis',(0.,1.,0.));
#31645=DIRECTION('ref_axis',(1.,0.,0.));
#31646=DIRECTION('center_axis',(0.,1.,0.));
#31647=DIRECTION('ref_axis',(1.,0.,0.));
#31648=DIRECTION('',(-0.447213595499958,0.894427190999916,-5.47678698264203E-17));
#31649=DIRECTION('center_axis',(0.,-1.,0.));
#31650=DIRECTION('ref_axis',(1.,0.,0.));
#31651=DIRECTION('',(0.,1.,0.));
#31652=DIRECTION('axis',(0.,0.,1.));
#31653=DIRECTION('refdir',(1.,0.,0.));
#31654=DIRECTION('center_axis',(1.,0.,0.));
#31655=DIRECTION('ref_axis',(0.,0.207879895528894,-0.978154358490978));
#31656=DIRECTION('',(-1.,0.,0.));
#31657=DIRECTION('center_axis',(1.,0.,0.));
#31658=DIRECTION('ref_axis',(0.,0.,-1.));
#31659=DIRECTION('center_axis',(1.,0.,0.));
#31660=DIRECTION('ref_axis',(0.,0.,-1.));
#31661=DIRECTION('',(-1.,0.,0.));
#31662=DIRECTION('center_axis',(1.,0.,0.));
#31663=DIRECTION('ref_axis',(0.,0.,-1.));
#31664=DIRECTION('',(-1.,0.,0.));
#31665=DIRECTION('center_axis',(1.,0.,0.));
#31666=DIRECTION('ref_axis',(0.,0.,-1.));
#31667=DIRECTION('',(-1.,0.,0.));
#31668=DIRECTION('center_axis',(1.,0.,0.));
#31669=DIRECTION('ref_axis',(0.,0.,-1.));
#31670=DIRECTION('',(-1.,0.,0.));
#31671=DIRECTION('center_axis',(1.,0.,0.));
#31672=DIRECTION('ref_axis',(0.,0.,-1.));
#31673=DIRECTION('',(-1.,0.,0.));
#31674=DIRECTION('center_axis',(1.,0.,0.));
#31675=DIRECTION('ref_axis',(0.,0.,-1.));
#31676=DIRECTION('',(-1.,0.,0.));
#31677=DIRECTION('center_axis',(1.,0.,0.));
#31678=DIRECTION('ref_axis',(0.,0.,-1.));
#31679=DIRECTION('',(-1.,0.,0.));
#31680=DIRECTION('center_axis',(1.,0.,0.));
#31681=DIRECTION('ref_axis',(0.,0.,-1.));
#31682=DIRECTION('',(-1.,0.,0.));
#31683=DIRECTION('center_axis',(1.,0.,0.));
#31684=DIRECTION('ref_axis',(0.,0.,-1.));
#31685=DIRECTION('center_axis',(1.,0.,0.));
#31686=DIRECTION('ref_axis',(0.,2.68771689099506E-14,-1.));
#31687=DIRECTION('',(1.,3.30650148539799E-30,-1.22464679914735E-16));
#31688=DIRECTION('center_axis',(-1.,0.,0.));
#31689=DIRECTION('ref_axis',(0.,2.68771689099506E-14,-1.));
#31690=DIRECTION('center_axis',(1.,0.,0.));
#31691=DIRECTION('ref_axis',(0.,2.68771689099506E-14,-1.));
#31692=DIRECTION('',(1.,3.30650148539799E-30,-1.22464679914735E-16));
#31693=DIRECTION('center_axis',(1.,0.,0.));
#31694=DIRECTION('ref_axis',(0.,2.68771689099506E-14,-1.));
#31695=DIRECTION('',(1.,3.30650148539799E-30,-1.22464679914735E-16));
#31696=DIRECTION('center_axis',(1.,0.,0.));
#31697=DIRECTION('ref_axis',(0.,2.68771689099506E-14,-1.));
#31698=DIRECTION('',(1.,3.30650148539799E-30,-1.22464679914735E-16));
#31699=DIRECTION('center_axis',(1.,0.,0.));
#31700=DIRECTION('ref_axis',(0.,2.68771689099506E-14,-1.));
#31701=DIRECTION('',(1.,3.30650148539799E-30,-1.22464679914735E-16));
#31702=DIRECTION('center_axis',(1.,0.,0.));
#31703=DIRECTION('ref_axis',(0.,2.68771689099506E-14,-1.));
#31704=DIRECTION('',(1.,3.30650148539799E-30,-1.22464679914735E-16));
#31705=DIRECTION('center_axis',(1.,0.,0.));
#31706=DIRECTION('ref_axis',(0.,2.68771689099506E-14,-1.));
#31707=DIRECTION('',(1.,3.30650148539799E-30,-1.22464679914735E-16));
#31708=DIRECTION('center_axis',(1.,0.,0.));
#31709=DIRECTION('ref_axis',(0.,2.68771689099506E-14,-1.));
#31710=DIRECTION('',(1.,3.30650148539799E-30,-1.22464679914735E-16));
#31711=DIRECTION('center_axis',(1.,0.,0.));
#31712=DIRECTION('ref_axis',(0.,2.68771689099506E-14,-1.));
#31713=DIRECTION('',(1.,3.30650148539799E-30,-1.22464679914735E-16));
#31714=DIRECTION('center_axis',(1.,0.,0.));
#31715=DIRECTION('ref_axis',(0.,2.68771689099506E-14,-1.));
#31716=DIRECTION('center_axis',(1.,0.,0.));
#31717=DIRECTION('ref_axis',(0.,2.68771689099506E-14,-1.));
#31718=DIRECTION('center_axis',(1.,0.,0.));
#31719=DIRECTION('ref_axis',(0.,0.,-1.));
#31720=DIRECTION('',(0.,1.,0.));
#31721=DIRECTION('center_axis',(1.,0.,0.));
#31722=DIRECTION('ref_axis',(0.,0.,-1.));
#31723=DIRECTION('center_axis',(1.,0.,0.));
#31724=DIRECTION('ref_axis',(0.,0.,-1.));
#31725=DIRECTION('center_axis',(-1.,0.,0.));
#31726=DIRECTION('ref_axis',(0.,0.,-1.));
#31727=DIRECTION('center_axis',(-1.,0.,0.));
#31728=DIRECTION('ref_axis',(0.,0.,-1.));
#31729=DIRECTION('center_axis',(-1.,0.,0.));
#31730=DIRECTION('ref_axis',(0.,0.,-1.));
#31731=DIRECTION('center_axis',(1.,0.,0.));
#31732=DIRECTION('ref_axis',(0.,0.,-1.));
#31733=DIRECTION('center_axis',(1.,0.,0.));
#31734=DIRECTION('ref_axis',(0.,0.,-1.));
#31735=DIRECTION('',(1.,0.,0.));
#31736=DIRECTION('center_axis',(1.,0.,0.));
#31737=DIRECTION('ref_axis',(0.,0.,-1.));
#31738=DIRECTION('center_axis',(1.,0.,0.));
#31739=DIRECTION('ref_axis',(0.,0.,-1.));
#31740=DIRECTION('',(1.,0.,0.));
#31741=DIRECTION('center_axis',(1.,0.,0.));
#31742=DIRECTION('ref_axis',(0.,0.,-1.));
#31743=DIRECTION('center_axis',(1.,0.,0.));
#31744=DIRECTION('ref_axis',(0.,0.,-1.));
#31745=DIRECTION('',(1.,0.,0.));
#31746=DIRECTION('center_axis',(0.,0.,1.));
#31747=DIRECTION('ref_axis',(0.,-1.,0.));
#31748=DIRECTION('',(0.,-1.,0.));
#31749=DIRECTION('',(-1.,0.,0.));
#31750=DIRECTION('',(1.,0.,0.));
#31751=DIRECTION('center_axis',(1.,0.,0.));
#31752=DIRECTION('ref_axis',(0.,0.,-1.));
#31753=DIRECTION('center_axis',(1.,0.,0.));
#31754=DIRECTION('ref_axis',(0.,0.,-1.));
#31755=DIRECTION('center_axis',(1.,0.,0.));
#31756=DIRECTION('ref_axis',(0.,0.,-1.));
#31757=DIRECTION('center_axis',(1.,0.,0.));
#31758=DIRECTION('ref_axis',(0.,-1.22464679914735E-16,1.));
#31759=DIRECTION('center_axis',(1.,0.,0.));
#31760=DIRECTION('ref_axis',(0.,0.,-1.));
#31761=DIRECTION('center_axis',(1.,0.,0.));
#31762=DIRECTION('ref_axis',(0.,0.,-1.));
#31763=DIRECTION('',(-1.,0.,0.));
#31764=DIRECTION('center_axis',(1.,0.,0.));
#31765=DIRECTION('ref_axis',(0.,0.,-1.));
#31766=DIRECTION('center_axis',(1.,0.,0.));
#31767=DIRECTION('ref_axis',(0.,0.,-1.));
#31768=DIRECTION('axis',(0.,0.,1.));
#31769=DIRECTION('refdir',(1.,0.,0.));
#31770=DIRECTION('center_axis',(0.,1.,0.));
#31771=DIRECTION('ref_axis',(0.,0.,1.));
#31772=DIRECTION('center_axis',(0.,-1.,0.));
#31773=DIRECTION('ref_axis',(1.,0.,0.));
#31774=DIRECTION('center_axis',(0.,-1.,0.));
#31775=DIRECTION('ref_axis',(1.,0.,0.));
#31776=DIRECTION('center_axis',(0.,-1.,0.));
#31777=DIRECTION('ref_axis',(1.,0.,0.));
#31778=DIRECTION('',(0.707106781186547,0.707106781186548,8.65956056235493E-17));
#31779=DIRECTION('center_axis',(0.,-1.,0.));
#31780=DIRECTION('ref_axis',(1.,0.,0.));
#31781=DIRECTION('center_axis',(0.,-1.,0.));
#31782=DIRECTION('ref_axis',(1.,0.,0.));
#31783=DIRECTION('',(0.,1.,0.));
#31784=DIRECTION('center_axis',(0.,1.,0.));
#31785=DIRECTION('ref_axis',(1.,0.,0.));
#31786=DIRECTION('center_axis',(0.,-1.,0.));
#31787=DIRECTION('ref_axis',(1.,0.,0.));
#31788=DIRECTION('',(-0.707106781186547,0.707106781186548,-8.65956056235493E-17));
#31789=DIRECTION('center_axis',(0.,-1.,0.));
#31790=DIRECTION('ref_axis',(0.,0.,-1.));
#31791=DIRECTION('center_axis',(0.,-1.,0.));
#31792=DIRECTION('ref_axis',(1.,0.,0.));
#31793=DIRECTION('center_axis',(0.,1.,0.));
#31794=DIRECTION('ref_axis',(1.,0.,0.));
#31795=DIRECTION('center_axis',(0.,1.,0.));
#31796=DIRECTION('ref_axis',(1.,0.,0.));
#31797=DIRECTION('',(-0.447213595499958,0.894427190999916,-5.47678698264203E-17));
#31798=DIRECTION('center_axis',(0.,-1.,0.));
#31799=DIRECTION('ref_axis',(1.,0.,0.));
#31800=DIRECTION('center_axis',(0.,1.,0.));
#31801=DIRECTION('ref_axis',(1.,0.,0.));
#31802=DIRECTION('',(0.,1.,0.));
#31803=DIRECTION('center_axis',(0.,1.,0.));
#31804=DIRECTION('ref_axis',(1.,0.,0.));
#31805=DIRECTION('center_axis',(0.,-1.,0.));
#31806=DIRECTION('ref_axis',(1.,0.,0.));
#31807=DIRECTION('',(-0.707106781186547,0.707106781186548,-8.65956056235493E-17));
#31808=DIRECTION('center_axis',(0.,-1.,0.));
#31809=DIRECTION('ref_axis',(0.,0.,-1.));
#31810=DIRECTION('center_axis',(0.866025403784439,0.,-0.5));
#31811=DIRECTION('ref_axis',(0.5,0.,0.866025403784439));
#31812=DIRECTION('',(-0.5,0.,-0.866025403784439));
#31813=DIRECTION('',(0.,-1.,0.));
#31814=DIRECTION('',(0.5,0.,0.866025403784439));
#31815=DIRECTION('',(0.,-1.,0.));
#31816=DIRECTION('center_axis',(1.60246890531964E-16,0.,-1.));
#31817=DIRECTION('ref_axis',(1.,0.,1.60246890531964E-16));
#31818=DIRECTION('',(-1.,0.,-1.60246890531964E-16));
#31819=DIRECTION('',(0.,-1.,0.));
#31820=DIRECTION('',(1.,0.,1.60246890531964E-16));
#31821=DIRECTION('center_axis',(-0.866025403784439,0.,-0.5));
#31822=DIRECTION('ref_axis',(0.5,0.,-0.866025403784439));
#31823=DIRECTION('',(-0.5,0.,0.866025403784439));
#31824=DIRECTION('',(0.,-1.,0.));
#31825=DIRECTION('',(0.5,0.,-0.866025403784439));
#31826=DIRECTION('center_axis',(-0.866025403784439,0.,0.5));
#31827=DIRECTION('ref_axis',(-0.5,0.,-0.866025403784439));
#31828=DIRECTION('',(0.5,0.,0.866025403784439));
#31829=DIRECTION('',(0.,-1.,0.));
#31830=DIRECTION('',(-0.5,0.,-0.866025403784439));
#31831=DIRECTION('center_axis',(-1.60246890531964E-16,0.,1.));
#31832=DIRECTION('ref_axis',(-1.,0.,-1.60246890531964E-16));
#31833=DIRECTION('',(1.,0.,1.60246890531964E-16));
#31834=DIRECTION('',(0.,-1.,0.));
#31835=DIRECTION('',(-1.,0.,-1.60246890531964E-16));
#31836=DIRECTION('center_axis',(0.866025403784439,0.,0.5));
#31837=DIRECTION('ref_axis',(-0.5,0.,0.866025403784439));
#31838=DIRECTION('',(0.5,0.,-0.866025403784439));
#31839=DIRECTION('',(-0.5,0.,0.866025403784439));
#31840=DIRECTION('center_axis',(0.,1.,0.));
#31841=DIRECTION('ref_axis',(1.,0.,0.));
#31842=DIRECTION('center_axis',(0.,-1.,0.));
#31843=DIRECTION('ref_axis',(0.,0.,-1.));
#31844=DIRECTION('axis',(0.,0.,1.));
#31845=DIRECTION('refdir',(1.,0.,0.));
#31846=DIRECTION('center_axis',(0.,1.,0.));
#31847=DIRECTION('ref_axis',(0.,0.,1.));
#31848=DIRECTION('center_axis',(0.,-1.,0.));
#31849=DIRECTION('ref_axis',(1.,0.,0.));
#31850=DIRECTION('center_axis',(0.,-1.,0.));
#31851=DIRECTION('ref_axis',(1.,0.,0.));
#31852=DIRECTION('center_axis',(0.,-1.,0.));
#31853=DIRECTION('ref_axis',(1.,0.,0.));
#31854=DIRECTION('',(0.707106781186548,0.707106781186547,8.65956056235493E-17));
#31855=DIRECTION('center_axis',(0.,-1.,0.));
#31856=DIRECTION('ref_axis',(1.,0.,0.));
#31857=DIRECTION('center_axis',(0.,-1.,0.));
#31858=DIRECTION('ref_axis',(1.,0.,0.));
#31859=DIRECTION('',(0.,1.,0.));
#31860=DIRECTION('center_axis',(0.,1.,0.));
#31861=DIRECTION('ref_axis',(1.,0.,0.));
#31862=DIRECTION('center_axis',(0.,-1.,0.));
#31863=DIRECTION('ref_axis',(1.,0.,0.));
#31864=DIRECTION('',(-0.707106781186547,0.707106781186548,-8.65956056235493E-17));
#31865=DIRECTION('center_axis',(0.,-1.,0.));
#31866=DIRECTION('ref_axis',(0.,0.,-1.));
#31867=DIRECTION('center_axis',(0.,-1.,0.));
#31868=DIRECTION('ref_axis',(1.,0.,0.));
#31869=DIRECTION('center_axis',(0.,1.,0.));
#31870=DIRECTION('ref_axis',(1.,0.,0.));
#31871=DIRECTION('center_axis',(0.,1.,0.));
#31872=DIRECTION('ref_axis',(1.,0.,0.));
#31873=DIRECTION('',(-0.447213595499958,0.894427190999916,-5.47678698264203E-17));
#31874=DIRECTION('center_axis',(0.,-1.,0.));
#31875=DIRECTION('ref_axis',(1.,0.,0.));
#31876=DIRECTION('center_axis',(0.,1.,0.));
#31877=DIRECTION('ref_axis',(1.,0.,0.));
#31878=DIRECTION('',(0.,1.,0.));
#31879=DIRECTION('center_axis',(0.,1.,0.));
#31880=DIRECTION('ref_axis',(1.,0.,0.));
#31881=DIRECTION('center_axis',(0.,-1.,0.));
#31882=DIRECTION('ref_axis',(1.,0.,0.));
#31883=DIRECTION('',(-0.707106781186547,0.707106781186548,-8.65956056235493E-17));
#31884=DIRECTION('center_axis',(0.,-1.,0.));
#31885=DIRECTION('ref_axis',(0.,0.,-1.));
#31886=DIRECTION('center_axis',(0.866025403784439,0.,-0.5));
#31887=DIRECTION('ref_axis',(0.5,0.,0.866025403784439));
#31888=DIRECTION('',(-0.5,0.,-0.866025403784439));
#31889=DIRECTION('',(0.,-1.,0.));
#31890=DIRECTION('',(0.5,0.,0.866025403784439));
#31891=DIRECTION('',(0.,-1.,0.));
#31892=DIRECTION('center_axis',(1.20185167898973E-16,0.,-1.));
#31893=DIRECTION('ref_axis',(1.,0.,1.20185167898973E-16));
#31894=DIRECTION('',(-1.,0.,-1.20185167898973E-16));
#31895=DIRECTION('',(0.,-1.,0.));
#31896=DIRECTION('',(1.,0.,1.20185167898973E-16));
#31897=DIRECTION('center_axis',(-0.866025403784439,0.,-0.5));
#31898=DIRECTION('ref_axis',(0.5,0.,-0.866025403784439));
#31899=DIRECTION('',(-0.5,0.,0.866025403784439));
#31900=DIRECTION('',(0.,-1.,0.));
#31901=DIRECTION('',(0.5,0.,-0.866025403784439));
#31902=DIRECTION('center_axis',(-0.866025403784439,0.,0.5));
#31903=DIRECTION('ref_axis',(-0.5,0.,-0.866025403784439));
#31904=DIRECTION('',(0.5,0.,0.866025403784439));
#31905=DIRECTION('',(0.,-1.,0.));
#31906=DIRECTION('',(-0.5,0.,-0.866025403784439));
#31907=DIRECTION('center_axis',(-2.40370335797945E-16,0.,1.));
#31908=DIRECTION('ref_axis',(-1.,0.,-2.40370335797945E-16));
#31909=DIRECTION('',(1.,0.,2.40370335797945E-16));
#31910=DIRECTION('',(0.,-1.,0.));
#31911=DIRECTION('',(-1.,0.,-2.40370335797945E-16));
#31912=DIRECTION('center_axis',(0.866025403784439,0.,0.5));
#31913=DIRECTION('ref_axis',(-0.5,0.,0.866025403784439));
#31914=DIRECTION('',(0.5,0.,-0.866025403784439));
#31915=DIRECTION('',(-0.5,0.,0.866025403784439));
#31916=DIRECTION('center_axis',(0.,1.,0.));
#31917=DIRECTION('ref_axis',(1.,0.,0.));
#31918=DIRECTION('center_axis',(0.,-1.,0.));
#31919=DIRECTION('ref_axis',(0.,0.,-1.));
#31920=DIRECTION('',(0.,0.,1.));
#31921=DIRECTION('',(1.,0.,0.));
#31922=DIRECTION('',(0.,0.,1.));
#31923=DIRECTION('',(1.,0.,0.));
#31924=DIRECTION('',(0.,0.,1.));
#31925=DIRECTION('',(1.,0.,0.));
#31926=DIRECTION('',(0.,0.,1.));
#31927=DIRECTION('',(1.,0.,0.));
#31928=DIRECTION('',(0.,-1.,2.22044604925031E-16));
#31929=DIRECTION('',(1.,0.,0.));
#31930=DIRECTION('',(0.,-1.,2.22044604925031E-16));
#31931=DIRECTION('',(1.,0.,0.));
#31932=DIRECTION('',(0.,-1.,2.22044604925031E-16));
#31933=DIRECTION('',(1.,0.,0.));
#31934=DIRECTION('',(0.,-1.,2.22044604925031E-16));
#31935=DIRECTION('',(1.,0.,0.));
#31936=DIRECTION('',(0.,-1.,2.22044604925031E-16));
#31937=DIRECTION('',(1.,0.,0.));
#31938=DIRECTION('',(0.,-1.,2.22044604925031E-16));
#31939=DIRECTION('',(1.,0.,0.));
#31940=DIRECTION('',(0.,-1.,2.22044604925031E-16));
#31941=DIRECTION('',(1.,0.,0.));
#31942=DIRECTION('',(0.,-1.,2.22044604925031E-16));
#31943=DIRECTION('',(1.,0.,0.));
#31944=DIRECTION('',(0.,0.,1.));
#31945=DIRECTION('',(1.,0.,0.));
#31946=DIRECTION('',(0.,0.,1.));
#31947=DIRECTION('',(2.22044604925031E-16,-1.,0.));
#31948=DIRECTION('',(0.,0.,1.));
#31949=DIRECTION('',(2.22044604925031E-16,-1.,0.));
#31950=DIRECTION('',(0.,0.,1.));
#31951=DIRECTION('',(2.22044604925031E-16,-1.,0.));
#31952=DIRECTION('',(0.,-1.,2.22044604925031E-16));
#31953=DIRECTION('',(1.,0.,0.));
#31954=DIRECTION('',(0.,-1.,2.22044604925031E-16));
#31955=DIRECTION('',(1.,0.,0.));
#31956=DIRECTION('',(0.,-1.,2.22044604925031E-16));
#31957=DIRECTION('',(1.,0.,0.));
#31958=DIRECTION('',(0.,-1.,2.22044604925031E-16));
#31959=DIRECTION('',(1.,0.,0.));
#31960=DIRECTION('axis',(0.,0.,1.));
#31961=DIRECTION('refdir',(1.,0.,0.));
#31962=DIRECTION('axis',(0.,0.,1.));
#31963=DIRECTION('refdir',(1.,0.,0.));
#31964=DIRECTION('center_axis',(1.,0.,0.));
#31965=DIRECTION('ref_axis',(0.,0.975560628713931,0.219730425074181));
#31966=DIRECTION('',(-1.,0.,0.));
#31967=DIRECTION('center_axis',(-1.,0.,0.));
#31968=DIRECTION('ref_axis',(0.,0.,-1.));
#31969=DIRECTION('center_axis',(1.,0.,0.));
#31970=DIRECTION('ref_axis',(0.,0.,-1.));
#31971=DIRECTION('',(-1.,0.,0.));
#31972=DIRECTION('center_axis',(1.,0.,0.));
#31973=DIRECTION('ref_axis',(0.,0.,-1.));
#31974=DIRECTION('',(-1.,0.,0.));
#31975=DIRECTION('center_axis',(1.,0.,0.));
#31976=DIRECTION('ref_axis',(0.,0.,-1.));
#31977=DIRECTION('',(-1.,0.,0.));
#31978=DIRECTION('center_axis',(1.,0.,0.));
#31979=DIRECTION('ref_axis',(0.,0.,-1.));
#31980=DIRECTION('',(-1.,0.,0.));
#31981=DIRECTION('center_axis',(1.,0.,0.));
#31982=DIRECTION('ref_axis',(0.,0.,-1.));
#31983=DIRECTION('',(-1.,0.,0.));
#31984=DIRECTION('center_axis',(1.,0.,0.));
#31985=DIRECTION('ref_axis',(0.,0.,-1.));
#31986=DIRECTION('',(-1.,0.,0.));
#31987=DIRECTION('center_axis',(1.,0.,0.));
#31988=DIRECTION('ref_axis',(0.,0.,-1.));
#31989=DIRECTION('',(-1.,0.,0.));
#31990=DIRECTION('center_axis',(1.,0.,0.));
#31991=DIRECTION('ref_axis',(0.,0.,-1.));
#31992=DIRECTION('',(-1.,0.,0.));
#31993=DIRECTION('center_axis',(1.,0.,0.));
#31994=DIRECTION('ref_axis',(0.,0.,-1.));
#31995=DIRECTION('',(-1.,0.,0.));
#31996=DIRECTION('center_axis',(1.,0.,0.));
#31997=DIRECTION('ref_axis',(0.,0.,-1.));
#31998=DIRECTION('',(-1.,0.,0.));
#31999=DIRECTION('center_axis',(1.,0.,0.));
#32000=DIRECTION('ref_axis',(0.,0.,-1.));
#32001=DIRECTION('',(-1.,0.,0.));
#32002=DIRECTION('center_axis',(1.,0.,0.));
#32003=DIRECTION('ref_axis',(0.,0.,-1.));
#32004=DIRECTION('',(-1.,0.,0.));
#32005=DIRECTION('center_axis',(1.,0.,0.));
#32006=DIRECTION('ref_axis',(0.,0.,-1.));
#32007=DIRECTION('',(-1.,0.,0.));
#32008=DIRECTION('center_axis',(1.,0.,0.));
#32009=DIRECTION('ref_axis',(0.,0.,-1.));
#32010=DIRECTION('',(-1.,0.,0.));
#32011=DIRECTION('center_axis',(1.,0.,0.));
#32012=DIRECTION('ref_axis',(0.,0.,-1.));
#32013=DIRECTION('',(-1.,0.,0.));
#32014=DIRECTION('center_axis',(1.,0.,0.));
#32015=DIRECTION('ref_axis',(0.,0.,-1.));
#32016=DIRECTION('',(-1.,0.,0.));
#32017=DIRECTION('center_axis',(1.,0.,0.));
#32018=DIRECTION('ref_axis',(0.,0.,-1.));
#32019=DIRECTION('',(-1.,0.,0.));
#32020=DIRECTION('center_axis',(1.,0.,0.));
#32021=DIRECTION('ref_axis',(0.,0.,-1.));
#32022=DIRECTION('',(-1.,0.,0.));
#32023=DIRECTION('center_axis',(1.,0.,0.));
#32024=DIRECTION('ref_axis',(0.,0.,-1.));
#32025=DIRECTION('',(-1.,0.,0.));
#32026=DIRECTION('center_axis',(1.,0.,0.));
#32027=DIRECTION('ref_axis',(0.,0.,-1.));
#32028=DIRECTION('',(-1.,0.,0.));
#32029=DIRECTION('center_axis',(1.,0.,0.));
#32030=DIRECTION('ref_axis',(0.,0.,-1.));
#32031=DIRECTION('',(-1.,0.,0.));
#32032=DIRECTION('center_axis',(1.,0.,0.));
#32033=DIRECTION('ref_axis',(0.,0.,-1.));
#32034=DIRECTION('',(-1.,0.,0.));
#32035=DIRECTION('center_axis',(1.,0.,0.));
#32036=DIRECTION('ref_axis',(0.,0.,-1.));
#32037=DIRECTION('',(-1.,0.,0.));
#32038=DIRECTION('center_axis',(1.,0.,0.));
#32039=DIRECTION('ref_axis',(0.,0.,-1.));
#32040=DIRECTION('',(-1.,0.,0.));
#32041=DIRECTION('center_axis',(1.,0.,0.));
#32042=DIRECTION('ref_axis',(0.,0.,-1.));
#32043=DIRECTION('',(-1.,0.,0.));
#32044=DIRECTION('center_axis',(1.,0.,0.));
#32045=DIRECTION('ref_axis',(0.,0.,-1.));
#32046=DIRECTION('',(-1.,0.,0.));
#32047=DIRECTION('center_axis',(1.,0.,0.));
#32048=DIRECTION('ref_axis',(0.,0.,-1.));
#32049=DIRECTION('',(-1.,0.,0.));
#32050=DIRECTION('center_axis',(1.,0.,0.));
#32051=DIRECTION('ref_axis',(0.,0.,-1.));
#32052=DIRECTION('',(-1.,0.,0.));
#32053=DIRECTION('center_axis',(1.,0.,0.));
#32054=DIRECTION('ref_axis',(0.,0.,-1.));
#32055=DIRECTION('',(-1.,0.,0.));
#32056=DIRECTION('center_axis',(1.,0.,0.));
#32057=DIRECTION('ref_axis',(0.,0.,-1.));
#32058=DIRECTION('',(-1.,0.,0.));
#32059=DIRECTION('center_axis',(1.,0.,0.));
#32060=DIRECTION('ref_axis',(0.,0.,-1.));
#32061=DIRECTION('',(-1.,0.,0.));
#32062=DIRECTION('center_axis',(1.,0.,0.));
#32063=DIRECTION('ref_axis',(0.,0.,-1.));
#32064=DIRECTION('',(-1.,0.,0.));
#32065=DIRECTION('center_axis',(1.,0.,0.));
#32066=DIRECTION('ref_axis',(0.,0.,-1.));
#32067=DIRECTION('',(-1.,0.,0.));
#32068=DIRECTION('center_axis',(1.,0.,0.));
#32069=DIRECTION('ref_axis',(0.,0.,-1.));
#32070=DIRECTION('',(-1.,0.,0.));
#32071=DIRECTION('center_axis',(1.,0.,0.));
#32072=DIRECTION('ref_axis',(0.,0.,-1.));
#32073=DIRECTION('',(-1.,0.,0.));
#32074=DIRECTION('center_axis',(1.,0.,0.));
#32075=DIRECTION('ref_axis',(0.,0.,-1.));
#32076=DIRECTION('',(-1.,0.,0.));
#32077=DIRECTION('center_axis',(1.,0.,0.));
#32078=DIRECTION('ref_axis',(0.,0.,-1.));
#32079=DIRECTION('',(-1.,0.,0.));
#32080=DIRECTION('center_axis',(1.,0.,0.));
#32081=DIRECTION('ref_axis',(0.,0.,-1.));
#32082=DIRECTION('',(-1.,0.,0.));
#32083=DIRECTION('center_axis',(1.,0.,0.));
#32084=DIRECTION('ref_axis',(0.,0.,-1.));
#32085=DIRECTION('',(-1.,0.,0.));
#32086=DIRECTION('center_axis',(1.,0.,0.));
#32087=DIRECTION('ref_axis',(0.,0.,-1.));
#32088=DIRECTION('',(-1.,0.,0.));
#32089=DIRECTION('center_axis',(1.,0.,0.));
#32090=DIRECTION('ref_axis',(0.,0.,-1.));
#32091=DIRECTION('',(-1.,0.,0.));
#32092=DIRECTION('center_axis',(1.,0.,0.));
#32093=DIRECTION('ref_axis',(0.,0.,-1.));
#32094=DIRECTION('',(-1.,0.,0.));
#32095=DIRECTION('center_axis',(1.,0.,0.));
#32096=DIRECTION('ref_axis',(0.,0.,-1.));
#32097=DIRECTION('',(-1.,0.,0.));
#32098=DIRECTION('center_axis',(1.,0.,0.));
#32099=DIRECTION('ref_axis',(0.,0.,-1.));
#32100=DIRECTION('',(-1.,0.,0.));
#32101=DIRECTION('center_axis',(1.,0.,0.));
#32102=DIRECTION('ref_axis',(0.,0.,-1.));
#32103=DIRECTION('',(-1.,0.,0.));
#32104=DIRECTION('center_axis',(1.,0.,0.));
#32105=DIRECTION('ref_axis',(0.,0.,-1.));
#32106=DIRECTION('',(-1.,0.,0.));
#32107=DIRECTION('center_axis',(1.,0.,0.));
#32108=DIRECTION('ref_axis',(0.,0.,-1.));
#32109=DIRECTION('',(-1.,0.,0.));
#32110=DIRECTION('center_axis',(1.,0.,0.));
#32111=DIRECTION('ref_axis',(0.,0.,-1.));
#32112=DIRECTION('',(-1.,0.,0.));
#32113=DIRECTION('center_axis',(1.,0.,0.));
#32114=DIRECTION('ref_axis',(0.,0.,-1.));
#32115=DIRECTION('',(-1.,0.,0.));
#32116=DIRECTION('center_axis',(1.,0.,0.));
#32117=DIRECTION('ref_axis',(0.,0.,-1.));
#32118=DIRECTION('',(-1.,0.,0.));
#32119=DIRECTION('center_axis',(1.,0.,0.));
#32120=DIRECTION('ref_axis',(0.,0.,-1.));
#32121=DIRECTION('',(-1.,0.,0.));
#32122=DIRECTION('center_axis',(1.,0.,0.));
#32123=DIRECTION('ref_axis',(0.,0.,-1.));
#32124=DIRECTION('',(-1.,0.,0.));
#32125=DIRECTION('center_axis',(1.,0.,0.));
#32126=DIRECTION('ref_axis',(0.,0.,-1.));
#32127=DIRECTION('',(-1.,0.,0.));
#32128=DIRECTION('center_axis',(1.,0.,0.));
#32129=DIRECTION('ref_axis',(0.,0.,-1.));
#32130=DIRECTION('',(-1.,0.,0.));
#32131=DIRECTION('center_axis',(1.,0.,0.));
#32132=DIRECTION('ref_axis',(0.,0.,-1.));
#32133=DIRECTION('',(-1.,0.,0.));
#32134=DIRECTION('center_axis',(1.,0.,0.));
#32135=DIRECTION('ref_axis',(0.,0.,-1.));
#32136=DIRECTION('',(-1.,0.,0.));
#32137=DIRECTION('center_axis',(1.,0.,0.));
#32138=DIRECTION('ref_axis',(0.,0.,-1.));
#32139=DIRECTION('',(-1.,0.,0.));
#32140=DIRECTION('center_axis',(1.,0.,0.));
#32141=DIRECTION('ref_axis',(0.,0.,-1.));
#32142=DIRECTION('',(-1.,0.,0.));
#32143=DIRECTION('center_axis',(1.,0.,0.));
#32144=DIRECTION('ref_axis',(0.,0.,-1.));
#32145=DIRECTION('',(-1.,0.,0.));
#32146=DIRECTION('center_axis',(1.,0.,0.));
#32147=DIRECTION('ref_axis',(0.,0.,-1.));
#32148=DIRECTION('',(-1.,0.,0.));
#32149=DIRECTION('center_axis',(1.,0.,0.));
#32150=DIRECTION('ref_axis',(0.,0.,-1.));
#32151=DIRECTION('',(-1.,0.,0.));
#32152=DIRECTION('center_axis',(1.,0.,0.));
#32153=DIRECTION('ref_axis',(0.,0.,-1.));
#32154=DIRECTION('',(-1.,0.,0.));
#32155=DIRECTION('center_axis',(1.,0.,0.));
#32156=DIRECTION('ref_axis',(0.,-1.17203152359781E-12,-1.));
#32157=DIRECTION('',(1.,0.,0.));
#32158=DIRECTION('center_axis',(1.,0.,0.));
#32159=DIRECTION('ref_axis',(0.,-1.17203152359781E-12,-1.));
#32160=DIRECTION('center_axis',(1.,0.,0.));
#32161=DIRECTION('ref_axis',(0.,-1.17203152359781E-12,-1.));
#32162=DIRECTION('',(1.,0.,0.));
#32163=DIRECTION('center_axis',(1.,0.,0.));
#32164=DIRECTION('ref_axis',(0.,-1.17203152359781E-12,-1.));
#32165=DIRECTION('center_axis',(1.,0.,0.));
#32166=DIRECTION('ref_axis',(0.,-1.17203152359781E-12,-1.));
#32167=DIRECTION('',(1.,0.,0.));
#32168=DIRECTION('center_axis',(1.,0.,0.));
#32169=DIRECTION('ref_axis',(0.,-1.17203152359781E-12,-1.));
#32170=DIRECTION('',(1.,0.,0.));
#32171=DIRECTION('center_axis',(1.,0.,0.));
#32172=DIRECTION('ref_axis',(0.,-1.17203152359781E-12,-1.));
#32173=DIRECTION('',(1.,0.,0.));
#32174=DIRECTION('center_axis',(1.,0.,0.));
#32175=DIRECTION('ref_axis',(0.,-1.17203152359781E-12,-1.));
#32176=DIRECTION('',(1.,0.,0.));
#32177=DIRECTION('center_axis',(1.,0.,0.));
#32178=DIRECTION('ref_axis',(0.,-1.17203152359781E-12,-1.));
#32179=DIRECTION('',(1.,0.,0.));
#32180=DIRECTION('center_axis',(1.,0.,0.));
#32181=DIRECTION('ref_axis',(0.,-1.17203152359781E-12,-1.));
#32182=DIRECTION('',(1.,0.,0.));
#32183=DIRECTION('center_axis',(1.,0.,0.));
#32184=DIRECTION('ref_axis',(0.,-1.17203152359781E-12,-1.));
#32185=DIRECTION('',(1.,0.,0.));
#32186=DIRECTION('center_axis',(1.,0.,0.));
#32187=DIRECTION('ref_axis',(0.,-1.17203152359781E-12,-1.));
#32188=DIRECTION('',(1.,0.,0.));
#32189=DIRECTION('center_axis',(1.,0.,0.));
#32190=DIRECTION('ref_axis',(0.,-1.17203152359781E-12,-1.));
#32191=DIRECTION('',(1.,0.,0.));
#32192=DIRECTION('center_axis',(1.,0.,0.));
#32193=DIRECTION('ref_axis',(0.,-1.17203152359781E-12,-1.));
#32194=DIRECTION('',(1.,0.,0.));
#32195=DIRECTION('center_axis',(1.,0.,0.));
#32196=DIRECTION('ref_axis',(0.,-1.17203152359781E-12,-1.));
#32197=DIRECTION('',(1.,0.,0.));
#32198=DIRECTION('center_axis',(1.,0.,0.));
#32199=DIRECTION('ref_axis',(0.,-1.17203152359781E-12,-1.));
#32200=DIRECTION('',(1.,0.,0.));
#32201=DIRECTION('center_axis',(1.,0.,0.));
#32202=DIRECTION('ref_axis',(0.,-1.17203152359781E-12,-1.));
#32203=DIRECTION('',(1.,0.,0.));
#32204=DIRECTION('center_axis',(1.,0.,0.));
#32205=DIRECTION('ref_axis',(0.,-1.17203152359781E-12,-1.));
#32206=DIRECTION('',(1.,0.,0.));
#32207=DIRECTION('center_axis',(1.,0.,0.));
#32208=DIRECTION('ref_axis',(0.,-1.17203152359781E-12,-1.));
#32209=DIRECTION('',(1.,0.,0.));
#32210=DIRECTION('center_axis',(1.,0.,0.));
#32211=DIRECTION('ref_axis',(0.,-1.17203152359781E-12,-1.));
#32212=DIRECTION('',(1.,0.,0.));
#32213=DIRECTION('center_axis',(1.,0.,0.));
#32214=DIRECTION('ref_axis',(0.,-1.17203152359781E-12,-1.));
#32215=DIRECTION('',(1.,0.,0.));
#32216=DIRECTION('center_axis',(1.,0.,0.));
#32217=DIRECTION('ref_axis',(0.,-1.17203152359781E-12,-1.));
#32218=DIRECTION('',(1.,0.,0.));
#32219=DIRECTION('center_axis',(1.,0.,0.));
#32220=DIRECTION('ref_axis',(0.,-1.17203152359781E-12,-1.));
#32221=DIRECTION('',(1.,0.,0.));
#32222=DIRECTION('center_axis',(1.,0.,0.));
#32223=DIRECTION('ref_axis',(0.,-1.17203152359781E-12,-1.));
#32224=DIRECTION('',(1.,0.,0.));
#32225=DIRECTION('center_axis',(1.,0.,0.));
#32226=DIRECTION('ref_axis',(0.,-1.17203152359781E-12,-1.));
#32227=DIRECTION('',(1.,0.,0.));
#32228=DIRECTION('center_axis',(1.,0.,0.));
#32229=DIRECTION('ref_axis',(0.,-1.17203152359781E-12,-1.));
#32230=DIRECTION('',(1.,0.,0.));
#32231=DIRECTION('center_axis',(1.,0.,0.));
#32232=DIRECTION('ref_axis',(0.,-1.17203152359781E-12,-1.));
#32233=DIRECTION('',(1.,0.,0.));
#32234=DIRECTION('center_axis',(1.,0.,0.));
#32235=DIRECTION('ref_axis',(0.,-1.17203152359781E-12,-1.));
#32236=DIRECTION('',(1.,0.,0.));
#32237=DIRECTION('center_axis',(1.,0.,0.));
#32238=DIRECTION('ref_axis',(0.,-1.17203152359781E-12,-1.));
#32239=DIRECTION('',(1.,0.,0.));
#32240=DIRECTION('center_axis',(1.,0.,0.));
#32241=DIRECTION('ref_axis',(0.,-1.17203152359781E-12,-1.));
#32242=DIRECTION('',(1.,0.,0.));
#32243=DIRECTION('center_axis',(1.,0.,0.));
#32244=DIRECTION('ref_axis',(0.,-1.17203152359781E-12,-1.));
#32245=DIRECTION('',(1.,0.,0.));
#32246=DIRECTION('center_axis',(1.,0.,0.));
#32247=DIRECTION('ref_axis',(0.,-1.17203152359781E-12,-1.));
#32248=DIRECTION('',(1.,0.,0.));
#32249=DIRECTION('center_axis',(1.,0.,0.));
#32250=DIRECTION('ref_axis',(0.,-1.17203152359781E-12,-1.));
#32251=DIRECTION('',(1.,0.,0.));
#32252=DIRECTION('center_axis',(1.,0.,0.));
#32253=DIRECTION('ref_axis',(0.,-1.17203152359781E-12,-1.));
#32254=DIRECTION('',(1.,0.,0.));
#32255=DIRECTION('center_axis',(1.,0.,0.));
#32256=DIRECTION('ref_axis',(0.,-1.17203152359781E-12,-1.));
#32257=DIRECTION('',(1.,0.,0.));
#32258=DIRECTION('center_axis',(1.,0.,0.));
#32259=DIRECTION('ref_axis',(0.,-1.17203152359781E-12,-1.));
#32260=DIRECTION('',(1.,0.,0.));
#32261=DIRECTION('center_axis',(1.,0.,0.));
#32262=DIRECTION('ref_axis',(0.,-1.17203152359781E-12,-1.));
#32263=DIRECTION('',(1.,0.,0.));
#32264=DIRECTION('center_axis',(1.,0.,0.));
#32265=DIRECTION('ref_axis',(0.,-1.17203152359781E-12,-1.));
#32266=DIRECTION('',(1.,0.,0.));
#32267=DIRECTION('center_axis',(1.,0.,0.));
#32268=DIRECTION('ref_axis',(0.,-1.17203152359781E-12,-1.));
#32269=DIRECTION('',(1.,0.,0.));
#32270=DIRECTION('center_axis',(1.,0.,0.));
#32271=DIRECTION('ref_axis',(0.,-1.17203152359781E-12,-1.));
#32272=DIRECTION('',(1.,0.,0.));
#32273=DIRECTION('center_axis',(1.,0.,0.));
#32274=DIRECTION('ref_axis',(0.,-1.17203152359781E-12,-1.));
#32275=DIRECTION('',(1.,0.,0.));
#32276=DIRECTION('center_axis',(1.,0.,0.));
#32277=DIRECTION('ref_axis',(0.,-1.17203152359781E-12,-1.));
#32278=DIRECTION('',(1.,0.,0.));
#32279=DIRECTION('center_axis',(1.,0.,0.));
#32280=DIRECTION('ref_axis',(0.,-1.17203152359781E-12,-1.));
#32281=DIRECTION('',(1.,0.,0.));
#32282=DIRECTION('center_axis',(1.,0.,0.));
#32283=DIRECTION('ref_axis',(0.,-1.17203152359781E-12,-1.));
#32284=DIRECTION('',(1.,0.,0.));
#32285=DIRECTION('center_axis',(1.,0.,0.));
#32286=DIRECTION('ref_axis',(0.,-1.17203152359781E-12,-1.));
#32287=DIRECTION('',(1.,0.,0.));
#32288=DIRECTION('center_axis',(1.,0.,0.));
#32289=DIRECTION('ref_axis',(0.,-1.17203152359781E-12,-1.));
#32290=DIRECTION('',(1.,0.,0.));
#32291=DIRECTION('center_axis',(1.,0.,0.));
#32292=DIRECTION('ref_axis',(0.,-1.17203152359781E-12,-1.));
#32293=DIRECTION('',(1.,0.,0.));
#32294=DIRECTION('center_axis',(1.,0.,0.));
#32295=DIRECTION('ref_axis',(0.,-1.17203152359781E-12,-1.));
#32296=DIRECTION('',(1.,0.,0.));
#32297=DIRECTION('center_axis',(1.,0.,0.));
#32298=DIRECTION('ref_axis',(0.,-1.17203152359781E-12,-1.));
#32299=DIRECTION('',(1.,0.,0.));
#32300=DIRECTION('center_axis',(1.,0.,0.));
#32301=DIRECTION('ref_axis',(0.,-1.17203152359781E-12,-1.));
#32302=DIRECTION('',(1.,0.,0.));
#32303=DIRECTION('center_axis',(1.,0.,0.));
#32304=DIRECTION('ref_axis',(0.,-1.17203152359781E-12,-1.));
#32305=DIRECTION('',(1.,0.,0.));
#32306=DIRECTION('center_axis',(1.,0.,0.));
#32307=DIRECTION('ref_axis',(0.,-1.17203152359781E-12,-1.));
#32308=DIRECTION('',(1.,0.,0.));
#32309=DIRECTION('center_axis',(1.,0.,0.));
#32310=DIRECTION('ref_axis',(0.,-1.17203152359781E-12,-1.));
#32311=DIRECTION('',(1.,0.,0.));
#32312=DIRECTION('center_axis',(1.,0.,0.));
#32313=DIRECTION('ref_axis',(0.,-1.17203152359781E-12,-1.));
#32314=DIRECTION('',(1.,0.,0.));
#32315=DIRECTION('center_axis',(1.,0.,0.));
#32316=DIRECTION('ref_axis',(0.,-1.17203152359781E-12,-1.));
#32317=DIRECTION('',(1.,0.,0.));
#32318=DIRECTION('center_axis',(1.,0.,0.));
#32319=DIRECTION('ref_axis',(0.,-1.17203152359781E-12,-1.));
#32320=DIRECTION('',(1.,0.,0.));
#32321=DIRECTION('center_axis',(1.,0.,0.));
#32322=DIRECTION('ref_axis',(0.,-1.17203152359781E-12,-1.));
#32323=DIRECTION('',(1.,0.,0.));
#32324=DIRECTION('center_axis',(1.,0.,0.));
#32325=DIRECTION('ref_axis',(0.,-1.17203152359781E-12,-1.));
#32326=DIRECTION('',(1.,0.,0.));
#32327=DIRECTION('center_axis',(1.,0.,0.));
#32328=DIRECTION('ref_axis',(0.,-1.17203152359781E-12,-1.));
#32329=DIRECTION('',(1.,0.,0.));
#32330=DIRECTION('center_axis',(1.,0.,0.));
#32331=DIRECTION('ref_axis',(0.,-1.17203152359781E-12,-1.));
#32332=DIRECTION('',(1.,0.,0.));
#32333=DIRECTION('center_axis',(1.,0.,0.));
#32334=DIRECTION('ref_axis',(0.,-1.17203152359781E-12,-1.));
#32335=DIRECTION('',(1.,0.,0.));
#32336=DIRECTION('center_axis',(1.,0.,0.));
#32337=DIRECTION('ref_axis',(0.,-1.17203152359781E-12,-1.));
#32338=DIRECTION('',(1.,0.,0.));
#32339=DIRECTION('center_axis',(1.,0.,0.));
#32340=DIRECTION('ref_axis',(0.,-1.17203152359781E-12,-1.));
#32341=DIRECTION('',(1.,0.,0.));
#32342=DIRECTION('center_axis',(1.,0.,0.));
#32343=DIRECTION('ref_axis',(0.,-1.17203152359781E-12,-1.));
#32344=DIRECTION('',(1.,0.,0.));
#32345=DIRECTION('center_axis',(1.,0.,0.));
#32346=DIRECTION('ref_axis',(0.,-1.17203152359781E-12,-1.));
#32347=DIRECTION('',(1.,0.,0.));
#32348=DIRECTION('center_axis',(1.,0.,0.));
#32349=DIRECTION('ref_axis',(0.,0.,-1.));
#32350=DIRECTION('center_axis',(1.,0.,0.));
#32351=DIRECTION('ref_axis',(0.,0.,-1.));
#32352=DIRECTION('center_axis',(-1.,0.,0.));
#32353=DIRECTION('ref_axis',(0.,-1.17203152359781E-12,-1.));
#32354=DIRECTION('center_axis',(1.,0.,0.));
#32355=DIRECTION('ref_axis',(0.,0.,-1.));
#32356=DIRECTION('',(-1.,0.,0.));
#32357=DIRECTION('center_axis',(1.,0.,0.));
#32358=DIRECTION('ref_axis',(0.,0.,-1.));
#32359=DIRECTION('center_axis',(1.,0.,0.));
#32360=DIRECTION('ref_axis',(0.,0.,-1.));
#32361=DIRECTION('center_axis',(1.,0.,0.));
#32362=DIRECTION('ref_axis',(0.,-1.17203152359781E-12,-1.));
#32363=DIRECTION('center_axis',(0.,1.,0.));
#32364=DIRECTION('ref_axis',(0.,0.,1.));
#32365=DIRECTION('',(-1.,0.,0.));
#32366=DIRECTION('',(0.,0.,1.));
#32367=DIRECTION('',(1.,0.,0.));
#32368=DIRECTION('',(0.,0.,1.));
#32369=DIRECTION('center_axis',(1.,0.,0.));
#32370=DIRECTION('ref_axis',(0.,0.,-1.));
#32371=DIRECTION('center_axis',(-1.,0.,0.));
#32372=DIRECTION('ref_axis',(0.,0.,-1.));
#32373=DIRECTION('',(0.,-1.,0.));
#32374=DIRECTION('',(0.,0.,-1.));
#32375=DIRECTION('center_axis',(0.,0.,1.));
#32376=DIRECTION('ref_axis',(0.,-1.,0.));
#32377=DIRECTION('',(0.,-1.,0.));
#32378=DIRECTION('',(1.,0.,0.));
#32379=DIRECTION('center_axis',(0.,-1.,0.));
#32380=DIRECTION('ref_axis',(0.,0.,-1.));
#32381=DIRECTION('',(1.,0.,0.));
#32382=DIRECTION('',(0.,0.,-1.));
#32383=DIRECTION('center_axis',(1.,0.,0.));
#32384=DIRECTION('ref_axis',(0.,0.,-1.));
#32385=DIRECTION('center_axis',(1.,0.,0.));
#32386=DIRECTION('ref_axis',(0.,0.,-1.));
#32387=DIRECTION('center_axis',(1.,0.,0.));
#32388=DIRECTION('ref_axis',(0.,0.,-1.));
#32389=DIRECTION('center_axis',(1.,0.,0.));
#32390=DIRECTION('ref_axis',(0.,0.,-1.));
#32391=DIRECTION('',(-1.,0.,0.));
#32392=DIRECTION('center_axis',(-1.,0.,0.));
#32393=DIRECTION('ref_axis',(0.,0.,-1.));
#32394=DIRECTION('center_axis',(1.,0.,0.));
#32395=DIRECTION('ref_axis',(0.,0.,-1.));
#32396=DIRECTION('center_axis',(1.,0.,0.));
#32397=DIRECTION('ref_axis',(0.,0.,-1.));
#32398=DIRECTION('center_axis',(1.,0.,0.));
#32399=DIRECTION('ref_axis',(0.,0.,-1.));
#32400=DIRECTION('center_axis',(-1.,0.,0.));
#32401=DIRECTION('ref_axis',(0.,0.,-1.));
#32402=DIRECTION('center_axis',(1.,0.,0.));
#32403=DIRECTION('ref_axis',(0.,0.,-1.));
#32404=DIRECTION('center_axis',(1.,0.,0.));
#32405=DIRECTION('ref_axis',(0.,0.,-1.));
#32406=DIRECTION('',(-1.,0.,0.));
#32407=DIRECTION('center_axis',(1.,0.,0.));
#32408=DIRECTION('ref_axis',(0.,0.,-1.));
#32409=DIRECTION('center_axis',(1.,0.,0.));
#32410=DIRECTION('ref_axis',(0.,0.,-1.));
#32411=DIRECTION('axis',(0.,0.,1.));
#32412=DIRECTION('refdir',(1.,0.,0.));
#32413=DIRECTION('center_axis',(1.,0.,0.));
#32414=DIRECTION('ref_axis',(0.,0.,-1.));
#32415=DIRECTION('center_axis',(-1.,0.,0.));
#32416=DIRECTION('ref_axis',(0.,0.,-1.));
#32417=DIRECTION('',(-1.,0.,0.));
#32418=DIRECTION('center_axis',(-1.,0.,0.));
#32419=DIRECTION('ref_axis',(0.,0.,-1.));
#32420=DIRECTION('center_axis',(1.,0.,0.));
#32421=DIRECTION('ref_axis',(0.,0.,-1.));
#32422=DIRECTION('center_axis',(1.,0.,0.));
#32423=DIRECTION('ref_axis',(0.,0.,-1.));
#32424=DIRECTION('',(-1.,0.,0.));
#32425=DIRECTION('center_axis',(1.,0.,0.));
#32426=DIRECTION('ref_axis',(0.,0.,-1.));
#32427=DIRECTION('center_axis',(1.,0.,0.));
#32428=DIRECTION('ref_axis',(0.,0.,-1.));
#32429=DIRECTION('center_axis',(1.,0.,0.));
#32430=DIRECTION('ref_axis',(0.,0.,-1.));
#32431=DIRECTION('axis',(0.,0.,1.));
#32432=DIRECTION('refdir',(1.,0.,0.));
#32433=DIRECTION('center_axis',(0.,1.,0.));
#32434=DIRECTION('ref_axis',(1.,0.,0.));
#32435=DIRECTION('',(1.,0.,0.));
#32436=DIRECTION('center_axis',(0.,1.,0.));
#32437=DIRECTION('ref_axis',(1.,0.,0.));
#32438=DIRECTION('center_axis',(0.,1.,0.));
#32439=DIRECTION('ref_axis',(1.,0.,0.));
#32440=DIRECTION('center_axis',(0.,1.,0.));
#32441=DIRECTION('ref_axis',(1.,0.,0.));
#32442=DIRECTION('',(0.,1.,0.));
#32443=DIRECTION('center_axis',(0.,1.,0.));
#32444=DIRECTION('ref_axis',(1.,0.,0.));
#32445=DIRECTION('',(-1.,0.,0.));
#32446=DIRECTION('center_axis',(1.,0.,0.));
#32447=DIRECTION('ref_axis',(0.,0.,-1.));
#32448=DIRECTION('center_axis',(-1.,0.,0.));
#32449=DIRECTION('ref_axis',(0.,0.,-1.));
#32450=DIRECTION('',(-1.,0.,0.));
#32451=DIRECTION('center_axis',(-1.,0.,0.));
#32452=DIRECTION('ref_axis',(0.,0.,-1.));
#32453=DIRECTION('center_axis',(1.,0.,0.));
#32454=DIRECTION('ref_axis',(0.,0.,-1.));
#32455=DIRECTION('center_axis',(1.,0.,0.));
#32456=DIRECTION('ref_axis',(0.,0.,-1.));
#32457=DIRECTION('',(-1.,0.,0.));
#32458=DIRECTION('center_axis',(1.,0.,0.));
#32459=DIRECTION('ref_axis',(0.,0.,-1.));
#32460=DIRECTION('center_axis',(1.,0.,0.));
#32461=DIRECTION('ref_axis',(0.,0.,-1.));
#32462=DIRECTION('center_axis',(1.,0.,0.));
#32463=DIRECTION('ref_axis',(0.,0.,-1.));
#32464=DIRECTION('axis',(0.,0.,1.));
#32465=DIRECTION('refdir',(1.,0.,0.));
#32466=DIRECTION('center_axis',(1.,0.,0.));
#32467=DIRECTION('ref_axis',(0.,0.,-1.));
#32468=DIRECTION('center_axis',(1.,0.,0.));
#32469=DIRECTION('ref_axis',(0.,0.,-1.));
#32470=DIRECTION('',(1.,0.,0.));
#32471=DIRECTION('center_axis',(-1.,0.,0.));
#32472=DIRECTION('ref_axis',(0.,0.,-1.));
#32473=DIRECTION('center_axis',(0.,1.,0.));
#32474=DIRECTION('ref_axis',(1.,0.,0.));
#32475=DIRECTION('',(1.,0.,0.));
#32476=DIRECTION('center_axis',(0.,1.,0.));
#32477=DIRECTION('ref_axis',(1.,0.,0.));
#32478=DIRECTION('center_axis',(0.,1.,0.));
#32479=DIRECTION('ref_axis',(1.,0.,0.));
#32480=DIRECTION('center_axis',(0.,1.,0.));
#32481=DIRECTION('ref_axis',(1.,0.,0.));
#32482=DIRECTION('',(0.,1.,0.));
#32483=DIRECTION('center_axis',(0.,1.,0.));
#32484=DIRECTION('ref_axis',(1.,0.,0.));
#32485=DIRECTION('',(-1.,0.,0.));
#32486=DIRECTION('center_axis',(0.,-1.,0.));
#32487=DIRECTION('ref_axis',(0.,0.,-1.));
#32488=DIRECTION('',(0.,0.,1.));
#32489=DIRECTION('',(1.,0.,0.));
#32490=DIRECTION('',(0.,0.,-1.));
#32491=DIRECTION('',(1.,0.,0.));
#32492=DIRECTION('',(0.,0.,-1.));
#32493=DIRECTION('',(-1.,0.,0.));
#32494=DIRECTION('center_axis',(0.,0.,-1.));
#32495=DIRECTION('ref_axis',(0.,1.,0.));
#32496=DIRECTION('',(0.,-1.,0.));
#32497=DIRECTION('',(1.,0.,0.));
#32498=DIRECTION('',(0.,1.,0.));
#32499=DIRECTION('center_axis',(0.,1.,0.));
#32500=DIRECTION('ref_axis',(0.,0.,1.));
#32501=DIRECTION('',(0.,0.,-1.));
#32502=DIRECTION('',(1.,0.,0.));
#32503=DIRECTION('',(0.,0.,1.));
#32504=DIRECTION('',(-1.,0.,0.));
#32505=DIRECTION('',(0.,0.,1.));
#32506=DIRECTION('center_axis',(1.,0.,0.));
#32507=DIRECTION('ref_axis',(0.,0.,-1.));
#32508=DIRECTION('center_axis',(1.,0.,0.));
#32509=DIRECTION('ref_axis',(0.,0.,-1.));
#32510=DIRECTION('center_axis',(-1.,0.,0.));
#32511=DIRECTION('ref_axis',(0.,0.,-1.));
#32512=DIRECTION('center_axis',(1.,0.,0.));
#32513=DIRECTION('ref_axis',(0.,0.,-1.));
#32514=DIRECTION('center_axis',(1.,0.,0.));
#32515=DIRECTION('ref_axis',(0.,0.,-1.));
#32516=DIRECTION('center_axis',(1.,0.,0.));
#32517=DIRECTION('ref_axis',(0.,0.,-1.));
#32518=DIRECTION('center_axis',(1.,0.,0.));
#32519=DIRECTION('ref_axis',(0.,0.,-1.));
#32520=DIRECTION('',(-1.,0.,0.));
#32521=DIRECTION('center_axis',(1.,0.,0.));
#32522=DIRECTION('ref_axis',(0.,1.22464679914735E-16,1.));
#32523=DIRECTION('center_axis',(-1.,0.,0.));
#32524=DIRECTION('ref_axis',(0.,0.,-1.));
#32525=DIRECTION('center_axis',(1.,0.,0.));
#32526=DIRECTION('ref_axis',(0.,1.22464679914735E-16,1.));
#32527=DIRECTION('center_axis',(1.,0.,0.));
#32528=DIRECTION('ref_axis',(0.,0.,-1.));
#32529=DIRECTION('center_axis',(1.,0.,0.));
#32530=DIRECTION('ref_axis',(0.,0.,-1.));
#32531=DIRECTION('axis',(0.,0.,1.));
#32532=DIRECTION('refdir',(1.,0.,0.));
#32533=DIRECTION('center_axis',(1.,0.,0.));
#32534=DIRECTION('ref_axis',(0.,0.,-1.));
#32535=DIRECTION('center_axis',(-1.,0.,0.));
#32536=DIRECTION('ref_axis',(0.,0.,-1.));
#32537=DIRECTION('',(-1.,0.,0.));
#32538=DIRECTION('center_axis',(-1.,0.,0.));
#32539=DIRECTION('ref_axis',(0.,0.,-1.));
#32540=DIRECTION('center_axis',(1.,0.,0.));
#32541=DIRECTION('ref_axis',(0.,0.,-1.));
#32542=DIRECTION('center_axis',(1.,0.,0.));
#32543=DIRECTION('ref_axis',(0.,0.,-1.));
#32544=DIRECTION('',(-1.,0.,0.));
#32545=DIRECTION('center_axis',(1.,0.,0.));
#32546=DIRECTION('ref_axis',(0.,0.,-1.));
#32547=DIRECTION('center_axis',(1.,0.,0.));
#32548=DIRECTION('ref_axis',(0.,0.,-1.));
#32549=DIRECTION('center_axis',(1.,0.,0.));
#32550=DIRECTION('ref_axis',(0.,0.,-1.));
#32551=DIRECTION('axis',(0.,0.,1.));
#32552=DIRECTION('refdir',(1.,0.,0.));
#32553=DIRECTION('center_axis',(1.,0.,0.));
#32554=DIRECTION('ref_axis',(0.,0.,-1.));
#32555=DIRECTION('center_axis',(-1.,0.,0.));
#32556=DIRECTION('ref_axis',(0.,0.,-1.));
#32557=DIRECTION('',(-1.,0.,0.));
#32558=DIRECTION('center_axis',(-1.,0.,0.));
#32559=DIRECTION('ref_axis',(0.,0.,-1.));
#32560=DIRECTION('center_axis',(1.,0.,0.));
#32561=DIRECTION('ref_axis',(0.,0.,-1.));
#32562=DIRECTION('center_axis',(1.,0.,0.));
#32563=DIRECTION('ref_axis',(0.,0.,-1.));
#32564=DIRECTION('',(-1.,0.,0.));
#32565=DIRECTION('center_axis',(1.,0.,0.));
#32566=DIRECTION('ref_axis',(0.,0.,-1.));
#32567=DIRECTION('center_axis',(1.,0.,0.));
#32568=DIRECTION('ref_axis',(0.,0.,-1.));
#32569=DIRECTION('center_axis',(1.,0.,0.));
#32570=DIRECTION('ref_axis',(0.,0.,-1.));
#32571=DIRECTION('axis',(0.,0.,1.));
#32572=DIRECTION('refdir',(1.,0.,0.));
#32573=DIRECTION('center_axis',(1.,0.,0.));
#32574=DIRECTION('ref_axis',(0.,0.,-1.));
#32575=DIRECTION('',(0.,-0.707106781186547,-0.707106781186548));
#32576=DIRECTION('',(0.,-1.,0.));
#32577=DIRECTION('',(0.,-0.707106781186547,0.707106781186548));
#32578=DIRECTION('',(0.,0.,1.));
#32579=DIRECTION('',(0.,0.707106781186547,0.707106781186548));
#32580=DIRECTION('',(0.,1.,0.));
#32581=DIRECTION('',(0.,0.707106781186547,-0.707106781186548));
#32582=DIRECTION('',(0.,0.,-1.));
#32583=DIRECTION('center_axis',(0.,0.707106781186548,-0.707106781186547));
#32584=DIRECTION('ref_axis',(-1.,0.,0.));
#32585=DIRECTION('',(1.,0.,0.));
#32586=DIRECTION('',(0.,-0.707106781186547,-0.707106781186548));
#32587=DIRECTION('',(-1.,0.,0.));
#32588=DIRECTION('center_axis',(0.,1.,0.));
#32589=DIRECTION('ref_axis',(-1.,0.,0.));
#32590=DIRECTION('',(-1.,0.,0.));
#32591=DIRECTION('',(0.,0.,-1.));
#32592=DIRECTION('center_axis',(0.,0.707106781186548,0.707106781186547));
#32593=DIRECTION('ref_axis',(1.,0.,0.));
#32594=DIRECTION('',(1.,0.,0.));
#32595=DIRECTION('',(0.,0.707106781186547,-0.707106781186548));
#32596=DIRECTION('center_axis',(0.,0.,1.));
#32597=DIRECTION('ref_axis',(1.,0.,0.));
#32598=DIRECTION('',(-1.,0.,0.));
#32599=DIRECTION('',(0.,1.,0.));
#32600=DIRECTION('center_axis',(1.,0.,0.));
#32601=DIRECTION('ref_axis',(0.,0.,-1.));
#32602=DIRECTION('',(0.,-0.707106781186547,0.707106781186548));
#32603=DIRECTION('',(0.,-1.,0.));
#32604=DIRECTION('',(0.,0.707106781186547,0.707106781186548));
#32605=DIRECTION('',(0.,0.,1.));
#32606=DIRECTION('center_axis',(0.,0.,1.));
#32607=DIRECTION('ref_axis',(1.,0.,0.));
#32608=DIRECTION('',(1.,0.,0.));
#32609=DIRECTION('center_axis',(0.,-0.707106781186548,0.707106781186547));
#32610=DIRECTION('ref_axis',(1.,0.,0.));
#32611=DIRECTION('',(1.,0.,0.));
#32612=DIRECTION('center_axis',(0.,-0.707106781186548,-0.707106781186547));
#32613=DIRECTION('ref_axis',(-1.,0.,0.));
#32614=DIRECTION('',(-1.,0.,0.));
#32615=DIRECTION('center_axis',(0.,-1.,0.));
#32616=DIRECTION('ref_axis',(1.,0.,0.));
#32617=DIRECTION('axis',(0.,0.,1.));
#32618=DIRECTION('refdir',(1.,0.,0.));
#32619=DIRECTION('center_axis',(0.866025403784439,0.,-0.5));
#32620=DIRECTION('ref_axis',(0.5,0.,0.866025403784439));
#32621=DIRECTION('',(0.5,0.,0.866025403784439));
#32622=DIRECTION('',(0.,-1.,0.));
#32623=DIRECTION('',(0.5,0.,0.866025403784439));
#32624=DIRECTION('',(0.,-1.,0.));
#32625=DIRECTION('center_axis',(1.92296268638356E-16,0.,-1.));
#32626=DIRECTION('ref_axis',(1.,0.,1.92296268638356E-16));
#32627=DIRECTION('',(1.,0.,1.92296268638356E-16));
#32628=DIRECTION('',(0.,-1.,0.));
#32629=DIRECTION('',(1.,0.,1.92296268638356E-16));
#32630=DIRECTION('center_axis',(-0.866025403784439,0.,-0.5));
#32631=DIRECTION('ref_axis',(0.5,0.,-0.866025403784439));
#32632=DIRECTION('',(0.5,0.,-0.866025403784439));
#32633=DIRECTION('',(0.,-1.,0.));
#32634=DIRECTION('',(0.5,0.,-0.866025403784438));
#32635=DIRECTION('center_axis',(-0.866025403784439,0.,0.5));
#32636=DIRECTION('ref_axis',(-0.5,0.,-0.866025403784439));
#32637=DIRECTION('',(-0.5,0.,-0.866025403784439));
#32638=DIRECTION('',(0.,-1.,0.));
#32639=DIRECTION('',(-0.5,0.,-0.866025403784439));
#32640=DIRECTION('center_axis',(-1.92296268638356E-16,0.,1.));
#32641=DIRECTION('ref_axis',(-1.,0.,-1.92296268638356E-16));
#32642=DIRECTION('',(-1.,0.,-1.92296268638356E-16));
#32643=DIRECTION('',(0.,-1.,0.));
#32644=DIRECTION('',(-1.,0.,-1.92296268638356E-16));
#32645=DIRECTION('center_axis',(0.866025403784439,0.,0.5));
#32646=DIRECTION('ref_axis',(-0.5,0.,0.866025403784439));
#32647=DIRECTION('',(-0.5,0.,0.866025403784439));
#32648=DIRECTION('',(-0.5,0.,0.866025403784439));
#32649=DIRECTION('center_axis',(0.,-1.,0.));
#32650=DIRECTION('ref_axis',(0.,0.,-1.));
#32651=DIRECTION('center_axis',(0.,1.,0.));
#32652=DIRECTION('ref_axis',(0.,0.,1.));
#32653=DIRECTION('center_axis',(0.,-1.,0.));
#32654=DIRECTION('ref_axis',(1.,0.,0.));
#32655=DIRECTION('center_axis',(0.,-1.,0.));
#32656=DIRECTION('ref_axis',(1.,0.,0.));
#32657=DIRECTION('center_axis',(0.,-1.,0.));
#32658=DIRECTION('ref_axis',(1.,0.,0.));
#32659=DIRECTION('',(0.707106781186547,0.707106781186548,8.65956056235493E-17));
#32660=DIRECTION('center_axis',(0.,-1.,0.));
#32661=DIRECTION('ref_axis',(1.,0.,0.));
#32662=DIRECTION('center_axis',(0.,1.,0.));
#32663=DIRECTION('ref_axis',(1.,0.,0.));
#32664=DIRECTION('',(0.,1.,0.));
#32665=DIRECTION('center_axis',(0.,1.,0.));
#32666=DIRECTION('ref_axis',(1.,0.,0.));
#32667=DIRECTION('center_axis',(0.,-1.,0.));
#32668=DIRECTION('ref_axis',(1.,0.,0.));
#32669=DIRECTION('',(-0.707106781186547,0.707106781186548,-8.65956056235493E-17));
#32670=DIRECTION('center_axis',(0.,-1.,0.));
#32671=DIRECTION('ref_axis',(0.,0.,-1.));
#32672=DIRECTION('axis',(0.,0.,1.));
#32673=DIRECTION('refdir',(1.,0.,0.));
#32674=DIRECTION('center_axis',(0.,1.,0.));
#32675=DIRECTION('ref_axis',(1.,0.,0.));
#32676=DIRECTION('center_axis',(0.,-1.,0.));
#32677=DIRECTION('ref_axis',(1.,0.,0.));
#32678=DIRECTION('',(0.,-1.,0.));
#32679=DIRECTION('center_axis',(0.,-1.,0.));
#32680=DIRECTION('ref_axis',(1.,0.,0.));
#32681=DIRECTION('center_axis',(0.,1.,0.));
#32682=DIRECTION('ref_axis',(1.,0.,0.));
#32683=DIRECTION('center_axis',(0.,1.,0.));
#32684=DIRECTION('ref_axis',(1.,0.,0.));
#32685=DIRECTION('',(0.,-1.,0.));
#32686=DIRECTION('center_axis',(0.,1.,0.));
#32687=DIRECTION('ref_axis',(1.,0.,0.));
#32688=DIRECTION('center_axis',(0.,1.,0.));
#32689=DIRECTION('ref_axis',(1.,0.,0.));
#32690=DIRECTION('center_axis',(0.,1.,0.));
#32691=DIRECTION('ref_axis',(1.,0.,0.));
#32692=DIRECTION('axis',(0.,0.,1.));
#32693=DIRECTION('refdir',(1.,0.,0.));
#32694=DIRECTION('center_axis',(0.,1.,0.));
#32695=DIRECTION('ref_axis',(0.,0.,1.));
#32696=DIRECTION('center_axis',(0.,-1.,0.));
#32697=DIRECTION('ref_axis',(1.,0.,0.));
#32698=DIRECTION('center_axis',(0.,-1.,0.));
#32699=DIRECTION('ref_axis',(1.,0.,0.));
#32700=DIRECTION('center_axis',(0.,-1.,0.));
#32701=DIRECTION('ref_axis',(1.,0.,0.));
#32702=DIRECTION('',(0.707106781186548,0.707106781186547,8.65956056235494E-17));
#32703=DIRECTION('center_axis',(0.,-1.,0.));
#32704=DIRECTION('ref_axis',(1.,0.,0.));
#32705=DIRECTION('center_axis',(0.,-1.,0.));
#32706=DIRECTION('ref_axis',(1.,0.,0.));
#32707=DIRECTION('',(0.,1.,0.));
#32708=DIRECTION('center_axis',(0.,1.,0.));
#32709=DIRECTION('ref_axis',(1.,0.,0.));
#32710=DIRECTION('center_axis',(0.,-1.,0.));
#32711=DIRECTION('ref_axis',(1.,0.,0.));
#32712=DIRECTION('',(-0.707106781186547,0.707106781186548,-8.65956056235493E-17));
#32713=DIRECTION('center_axis',(0.,-1.,0.));
#32714=DIRECTION('ref_axis',(0.,0.,-1.));
#32715=DIRECTION('center_axis',(0.,-1.,0.));
#32716=DIRECTION('ref_axis',(1.,0.,0.));
#32717=DIRECTION('center_axis',(0.,1.,0.));
#32718=DIRECTION('ref_axis',(1.,0.,0.));
#32719=DIRECTION('center_axis',(0.,1.,0.));
#32720=DIRECTION('ref_axis',(1.,0.,0.));
#32721=DIRECTION('',(-0.447213595499958,0.894427190999916,-5.47678698264203E-17));
#32722=DIRECTION('center_axis',(0.,-1.,0.));
#32723=DIRECTION('ref_axis',(1.,0.,0.));
#32724=DIRECTION('center_axis',(0.,1.,0.));
#32725=DIRECTION('ref_axis',(1.,0.,0.));
#32726=DIRECTION('',(0.,1.,0.));
#32727=DIRECTION('center_axis',(0.,1.,0.));
#32728=DIRECTION('ref_axis',(1.,0.,0.));
#32729=DIRECTION('center_axis',(0.,-1.,0.));
#32730=DIRECTION('ref_axis',(1.,0.,0.));
#32731=DIRECTION('',(-0.707106781186547,0.707106781186548,-8.65956056235493E-17));
#32732=DIRECTION('center_axis',(0.,-1.,0.));
#32733=DIRECTION('ref_axis',(0.,0.,-1.));
#32734=DIRECTION('center_axis',(0.866025403784439,0.,-0.5));
#32735=DIRECTION('ref_axis',(0.5,0.,0.866025403784439));
#32736=DIRECTION('',(-0.5,0.,-0.866025403784439));
#32737=DIRECTION('',(0.,-1.,0.));
#32738=DIRECTION('',(0.5,0.,0.866025403784439));
#32739=DIRECTION('',(0.,-1.,0.));
#32740=DIRECTION('center_axis',(1.92296268638356E-16,0.,-1.));
#32741=DIRECTION('ref_axis',(1.,0.,1.92296268638356E-16));
#32742=DIRECTION('',(-1.,0.,-1.92296268638356E-16));
#32743=DIRECTION('',(0.,-1.,0.));
#32744=DIRECTION('',(1.,0.,1.92296268638356E-16));
#32745=DIRECTION('center_axis',(-0.866025403784439,0.,-0.5));
#32746=DIRECTION('ref_axis',(0.5,0.,-0.866025403784439));
#32747=DIRECTION('',(-0.5,0.,0.866025403784438));
#32748=DIRECTION('',(0.,-1.,0.));
#32749=DIRECTION('',(0.5,0.,-0.866025403784438));
#32750=DIRECTION('center_axis',(-0.866025403784439,0.,0.5));
#32751=DIRECTION('ref_axis',(-0.5,0.,-0.866025403784439));
#32752=DIRECTION('',(0.5,0.,0.866025403784439));
#32753=DIRECTION('',(0.,-1.,0.));
#32754=DIRECTION('',(-0.5,0.,-0.866025403784439));
#32755=DIRECTION('center_axis',(-1.92296268638356E-16,0.,1.));
#32756=DIRECTION('ref_axis',(-1.,0.,-1.92296268638356E-16));
#32757=DIRECTION('',(1.,0.,1.92296268638356E-16));
#32758=DIRECTION('',(0.,-1.,0.));
#32759=DIRECTION('',(-1.,0.,-1.92296268638356E-16));
#32760=DIRECTION('center_axis',(0.866025403784439,0.,0.5));
#32761=DIRECTION('ref_axis',(-0.5,0.,0.866025403784439));
#32762=DIRECTION('',(0.5,0.,-0.866025403784439));
#32763=DIRECTION('',(-0.5,0.,0.866025403784439));
#32764=DIRECTION('center_axis',(0.,1.,0.));
#32765=DIRECTION('ref_axis',(1.,0.,0.));
#32766=DIRECTION('center_axis',(0.,-1.,0.));
#32767=DIRECTION('ref_axis',(0.,0.,-1.));
#32768=DIRECTION('',(0.,0.,1.));
#32769=DIRECTION('',(1.,0.,0.));
#32770=DIRECTION('',(0.,0.,1.));
#32771=DIRECTION('',(1.,0.,0.));
#32772=DIRECTION('',(0.,0.,1.));
#32773=DIRECTION('',(1.,0.,0.));
#32774=DIRECTION('',(0.,0.,1.));
#32775=DIRECTION('',(1.,0.,0.));
#32776=DIRECTION('',(0.,0.,1.));
#32777=DIRECTION('',(1.,0.,0.));
#32778=DIRECTION('',(0.,0.,1.));
#32779=DIRECTION('',(1.,0.,0.));
#32780=DIRECTION('',(0.,0.,1.));
#32781=DIRECTION('',(1.,0.,0.));
#32782=DIRECTION('',(0.,0.,1.));
#32783=DIRECTION('',(1.,0.,0.));
#32784=DIRECTION('',(0.,-1.,2.22044604925031E-16));
#32785=DIRECTION('',(1.,0.,0.));
#32786=DIRECTION('',(0.,-1.,2.22044604925031E-16));
#32787=DIRECTION('',(1.,0.,0.));
#32788=DIRECTION('',(0.,-1.,2.22044604925031E-16));
#32789=DIRECTION('',(1.,0.,0.));
#32790=DIRECTION('',(0.,-1.,2.22044604925031E-16));
#32791=DIRECTION('',(1.,0.,0.));
#32792=DIRECTION('',(0.,0.,1.));
#32793=DIRECTION('',(1.,0.,0.));
#32794=DIRECTION('',(0.,-1.,2.22044604925031E-16));
#32795=DIRECTION('',(1.,0.,0.));
#32796=DIRECTION('',(0.,-1.,2.22044604925031E-16));
#32797=DIRECTION('',(1.,0.,0.));
#32798=DIRECTION('',(0.,-1.,2.22044604925031E-16));
#32799=DIRECTION('',(1.,0.,0.));
#32800=DIRECTION('',(0.,-1.,2.22044604925031E-16));
#32801=DIRECTION('',(1.,0.,0.));
#32802=DIRECTION('',(0.,1.,2.22044604925031E-16));
#32803=DIRECTION('',(1.,0.,0.));
#32804=DIRECTION('',(0.,1.,2.22044604925031E-16));
#32805=DIRECTION('',(1.,0.,0.));
#32806=DIRECTION('',(0.,0.,1.));
#32807=DIRECTION('',(2.22044604925031E-16,-1.,0.));
#32808=DIRECTION('',(0.,0.,1.));
#32809=DIRECTION('',(2.22044604925031E-16,1.,0.));
#32810=DIRECTION('',(0.,0.,1.));
#32811=DIRECTION('',(2.22044604925031E-16,1.,0.));
#32812=DIRECTION('',(0.,0.,1.));
#32813=DIRECTION('',(2.22044604925031E-16,1.,0.));
#32814=DIRECTION('',(0.,1.,2.22044604925031E-16));
#32815=DIRECTION('',(1.,0.,0.));
#32816=DIRECTION('',(0.,1.,2.22044604925031E-16));
#32817=DIRECTION('',(1.,0.,0.));
#32818=DIRECTION('',(0.,0.,1.));
#32819=DIRECTION('',(2.22044604925031E-16,-1.,0.));
#32820=DIRECTION('',(0.,0.,1.));
#32821=DIRECTION('',(2.22044604925031E-16,-1.,0.));
#32822=DIRECTION('',(0.,0.,1.));
#32823=DIRECTION('',(2.22044604925031E-16,-1.,0.));
#32824=DIRECTION('',(0.,0.,1.));
#32825=DIRECTION('',(2.22044604925031E-16,-1.,0.));
#32826=DIRECTION('',(0.,-1.,2.22044604925031E-16));
#32827=DIRECTION('',(1.,0.,0.));
#32828=DIRECTION('',(0.,-1.,2.22044604925031E-16));
#32829=DIRECTION('',(1.,0.,0.));
#32830=DIRECTION('',(0.,-1.,2.22044604925031E-16));
#32831=DIRECTION('',(1.,0.,0.));
#32832=DIRECTION('',(0.,-1.,2.22044604925031E-16));
#32833=DIRECTION('',(1.,0.,0.));
#32834=DIRECTION('',(0.,-1.,2.22044604925031E-16));
#32835=DIRECTION('',(1.,0.,0.));
#32836=DIRECTION('',(0.,-1.,2.22044604925031E-16));
#32837=DIRECTION('',(1.,0.,0.));
#32838=DIRECTION('',(0.,0.,1.));
#32839=DIRECTION('',(1.,0.,0.));
#32840=DIRECTION('',(0.,0.,1.));
#32841=DIRECTION('',(1.,0.,0.));
#32842=DIRECTION('',(0.,0.,1.));
#32843=DIRECTION('',(1.,0.,0.));
#32844=DIRECTION('',(0.,0.,1.));
#32845=DIRECTION('',(1.,0.,0.));
#32846=DIRECTION('',(0.,0.,1.));
#32847=DIRECTION('',(1.,0.,0.));
#32848=DIRECTION('',(0.,0.,1.));
#32849=DIRECTION('',(1.,0.,0.));
#32850=DIRECTION('',(0.,-1.22464679914735E-16,-1.));
#32851=DIRECTION('',(1.,0.,0.));
#32852=DIRECTION('',(0.,0.,1.));
#32853=DIRECTION('',(1.,0.,0.));
#32854=DIRECTION('',(0.,0.,1.));
#32855=DIRECTION('',(1.,0.,0.));
#32856=DIRECTION('',(0.,0.,1.));
#32857=DIRECTION('',(2.22044604925031E-16,-1.,0.));
#32858=DIRECTION('',(0.,0.,1.));
#32859=DIRECTION('',(2.22044604925031E-16,-1.,0.));
#32860=DIRECTION('',(0.,0.,1.));
#32861=DIRECTION('',(1.,0.,0.));
#32862=DIRECTION('',(0.,0.,1.));
#32863=DIRECTION('',(1.,0.,0.));
#32864=DIRECTION('',(0.,0.866025403784439,-0.5));
#32865=DIRECTION('',(1.,0.,0.));
#32866=DIRECTION('',(0.,0.,1.));
#32867=DIRECTION('',(1.,0.,0.));
#32868=DIRECTION('',(0.,0.,1.));
#32869=DIRECTION('',(2.22044604925031E-16,1.,0.));
#32870=CARTESIAN_POINT('',(0.,0.,0.));
#32871=CARTESIAN_POINT('',(0.,0.,0.));
#32872=CARTESIAN_POINT('',(0.,0.,0.));
#32873=CARTESIAN_POINT('',(0.,0.,0.));
#32874=CARTESIAN_POINT('Origin',(23.5,-9.25,-0.1));
#32875=CARTESIAN_POINT('',(23.29,-9.25,0.));
#32876=CARTESIAN_POINT('Origin',(23.5,-9.25,0.));
#32877=CARTESIAN_POINT('',(23.29,-9.25,1.2));
#32878=CARTESIAN_POINT('',(23.29,-9.25,-0.1));
#32879=CARTESIAN_POINT('Origin',(23.5,-9.25,1.2));
#32880=CARTESIAN_POINT('Origin',(3.5,-9.25,-0.1));
#32881=CARTESIAN_POINT('',(3.29,-9.25,0.));
#32882=CARTESIAN_POINT('Origin',(3.5,-9.25,0.));
#32883=CARTESIAN_POINT('',(3.29,-9.25,1.2));
#32884=CARTESIAN_POINT('',(3.29,-9.25,-0.1));
#32885=CARTESIAN_POINT('Origin',(3.5,-9.25,1.2));
#32886=CARTESIAN_POINT('Origin',(24.,-3.5,-0.1));
#32887=CARTESIAN_POINT('',(23.67,-3.5,0.));
#32888=CARTESIAN_POINT('Origin',(24.,-3.5,0.));
#32889=CARTESIAN_POINT('',(23.67,-3.5,1.2));
#32890=CARTESIAN_POINT('',(23.67,-3.5,-0.1));
#32891=CARTESIAN_POINT('Origin',(24.,-3.5,1.2));
#32892=CARTESIAN_POINT('Origin',(24.,3.5,-0.1));
#32893=CARTESIAN_POINT('',(23.67,3.5,0.));
#32894=CARTESIAN_POINT('Origin',(24.,3.5,0.));
#32895=CARTESIAN_POINT('',(23.67,3.5,1.2));
#32896=CARTESIAN_POINT('',(23.67,3.5,-0.1));
#32897=CARTESIAN_POINT('Origin',(24.,3.5,1.2));
#32898=CARTESIAN_POINT('Origin',(3.,-2.4,-0.1));
#32899=CARTESIAN_POINT('',(2.725,-2.4,0.));
#32900=CARTESIAN_POINT('Origin',(3.,-2.4,0.));
#32901=CARTESIAN_POINT('',(2.725,-2.4,1.2));
#32902=CARTESIAN_POINT('',(2.725,-2.4,-0.1));
#32903=CARTESIAN_POINT('Origin',(3.,-2.4,1.2));
#32904=CARTESIAN_POINT('Origin',(3.,2.4,-0.1));
#32905=CARTESIAN_POINT('',(2.725,2.4,0.));
#32906=CARTESIAN_POINT('Origin',(3.,2.4,0.));
#32907=CARTESIAN_POINT('',(2.725,2.4,1.2));
#32908=CARTESIAN_POINT('',(2.725,2.4,-0.1));
#32909=CARTESIAN_POINT('Origin',(3.,2.4,1.2));
#32910=CARTESIAN_POINT('Origin',(26.,-7.8,-0.1));
#32911=CARTESIAN_POINT('',(25.79,-7.8,0.));
#32912=CARTESIAN_POINT('Origin',(26.,-7.8,0.));
#32913=CARTESIAN_POINT('',(25.79,-7.8,1.2));
#32914=CARTESIAN_POINT('',(25.79,-7.8,-0.1));
#32915=CARTESIAN_POINT('Origin',(26.,-7.8,1.2));
#32916=CARTESIAN_POINT('Origin',(1.,-5.5,-0.1));
#32917=CARTESIAN_POINT('',(0.79,-5.5,0.));
#32918=CARTESIAN_POINT('Origin',(1.,-5.5,0.));
#32919=CARTESIAN_POINT('',(0.79,-5.5,1.2));
#32920=CARTESIAN_POINT('',(0.79,-5.5,-0.1));
#32921=CARTESIAN_POINT('Origin',(1.,-5.5,1.2));
#32922=CARTESIAN_POINT('Origin',(1.,-7.8,-0.1));
#32923=CARTESIAN_POINT('',(0.79,-7.8,0.));
#32924=CARTESIAN_POINT('Origin',(1.,-7.8,0.));
#32925=CARTESIAN_POINT('',(0.79,-7.8,1.2));
#32926=CARTESIAN_POINT('',(0.79,-7.8,-0.1));
#32927=CARTESIAN_POINT('Origin',(1.,-7.8,1.2));
#32928=CARTESIAN_POINT('Origin',(26.,-5.5,-0.1));
#32929=CARTESIAN_POINT('',(25.79,-5.5,0.));
#32930=CARTESIAN_POINT('Origin',(26.,-5.5,0.));
#32931=CARTESIAN_POINT('',(25.79,-5.5,1.2));
#32932=CARTESIAN_POINT('',(25.79,-5.5,-0.1));
#32933=CARTESIAN_POINT('Origin',(26.,-5.5,1.2));
#32934=CARTESIAN_POINT('Origin',(27.,5.,0.));
#32935=CARTESIAN_POINT('',(27.,5.,0.));
#32936=CARTESIAN_POINT('',(0.,5.,0.));
#32937=CARTESIAN_POINT('',(27.,5.,0.));
#32938=CARTESIAN_POINT('',(0.,5.,1.2));
#32939=CARTESIAN_POINT('',(0.,5.,0.));
#32940=CARTESIAN_POINT('',(27.,5.,1.2));
#32941=CARTESIAN_POINT('',(27.,5.,1.2));
#32942=CARTESIAN_POINT('',(27.,5.,0.));
#32943=CARTESIAN_POINT('Origin',(27.,-10.,0.));
#32944=CARTESIAN_POINT('',(27.,-10.,0.));
#32945=CARTESIAN_POINT('',(27.,-10.,0.));
#32946=CARTESIAN_POINT('',(27.,-10.,1.2));
#32947=CARTESIAN_POINT('',(27.,-10.,1.2));
#32948=CARTESIAN_POINT('',(27.,-10.,0.));
#32949=CARTESIAN_POINT('Origin',(0.,-10.,0.));
#32950=CARTESIAN_POINT('',(0.,-10.,0.));
#32951=CARTESIAN_POINT('',(0.,-10.,0.));
#32952=CARTESIAN_POINT('',(0.,-10.,1.2));
#32953=CARTESIAN_POINT('',(0.,-10.,1.2));
#32954=CARTESIAN_POINT('',(0.,-10.,0.));
#32955=CARTESIAN_POINT('Origin',(0.,5.,0.));
#32956=CARTESIAN_POINT('',(0.,5.,0.));
#32957=CARTESIAN_POINT('',(0.,5.,1.2));
#32958=CARTESIAN_POINT('Origin',(13.5,-2.5,1.2));
#32959=CARTESIAN_POINT('Origin',(13.5,-2.5,0.));
#32960=CARTESIAN_POINT('',(0.,0.,0.));
#32961=CARTESIAN_POINT('Origin',(27.,-9.,-1.));
#32962=CARTESIAN_POINT('',(27.,-9.,-1.));
#32963=CARTESIAN_POINT('',(0.,-9.,-1.));
#32964=CARTESIAN_POINT('',(27.,-9.,-1.));
#32965=CARTESIAN_POINT('',(0.,-9.,0.));
#32966=CARTESIAN_POINT('',(0.,-9.,-1.));
#32967=CARTESIAN_POINT('',(27.,-9.,0.));
#32968=CARTESIAN_POINT('',(27.,-9.,0.));
#32969=CARTESIAN_POINT('',(27.,-9.,-1.));
#32970=CARTESIAN_POINT('Origin',(27.,-10.,-1.));
#32971=CARTESIAN_POINT('',(27.,-10.,-1.));
#32972=CARTESIAN_POINT('',(27.,-10.,-1.));
#32973=CARTESIAN_POINT('',(27.,-10.,0.));
#32974=CARTESIAN_POINT('',(27.,-10.,0.));
#32975=CARTESIAN_POINT('',(27.,-10.,-1.));
#32976=CARTESIAN_POINT('Origin',(0.,-10.,-1.));
#32977=CARTESIAN_POINT('',(0.,-10.,-1.));
#32978=CARTESIAN_POINT('',(0.,-10.,-1.));
#32979=CARTESIAN_POINT('',(0.,-10.,0.));
#32980=CARTESIAN_POINT('',(0.,-10.,0.));
#32981=CARTESIAN_POINT('',(0.,-10.,-1.));
#32982=CARTESIAN_POINT('Origin',(0.,-9.,-1.));
#32983=CARTESIAN_POINT('',(0.,-9.,-1.));
#32984=CARTESIAN_POINT('',(0.,-9.,0.));
#32985=CARTESIAN_POINT('Origin',(13.5,-9.5,0.));
#32986=CARTESIAN_POINT('Origin',(13.5,-9.5,-1.));
#32987=CARTESIAN_POINT('',(0.,0.,0.));
#32988=CARTESIAN_POINT('Origin',(27.,5.,-1.));
#32989=CARTESIAN_POINT('',(27.,5.,-1.));
#32990=CARTESIAN_POINT('',(0.,5.,-1.));
#32991=CARTESIAN_POINT('',(27.,5.,-1.));
#32992=CARTESIAN_POINT('',(0.,5.,0.));
#32993=CARTESIAN_POINT('',(0.,5.,-1.));
#32994=CARTESIAN_POINT('',(27.,5.,0.));
#32995=CARTESIAN_POINT('',(27.,5.,0.));
#32996=CARTESIAN_POINT('',(27.,5.,-1.));
#32997=CARTESIAN_POINT('Origin',(27.,4.,-1.));
#32998=CARTESIAN_POINT('',(27.,4.,-1.));
#32999=CARTESIAN_POINT('',(27.,4.,-1.));
#33000=CARTESIAN_POINT('',(27.,4.,0.));
#33001=CARTESIAN_POINT('',(27.,4.,0.));
#33002=CARTESIAN_POINT('',(27.,4.,-1.));
#33003=CARTESIAN_POINT('Origin',(0.,4.,-1.));
#33004=CARTESIAN_POINT('',(0.,4.,-1.));
#33005=CARTESIAN_POINT('',(0.,4.,-1.));
#33006=CARTESIAN_POINT('',(0.,4.,0.));
#33007=CARTESIAN_POINT('',(0.,4.,0.));
#33008=CARTESIAN_POINT('',(0.,4.,-1.));
#33009=CARTESIAN_POINT('Origin',(0.,5.,-1.));
#33010=CARTESIAN_POINT('',(0.,5.,-1.));
#33011=CARTESIAN_POINT('',(0.,5.,0.));
#33012=CARTESIAN_POINT('Origin',(13.5,4.5,0.));
#33013=CARTESIAN_POINT('Origin',(13.5,4.5,-1.));
#33014=CARTESIAN_POINT('',(0.,0.,0.));
#33015=CARTESIAN_POINT('Origin',(26.,-5.5,2.2));
#33016=CARTESIAN_POINT('',(25.5,-5.5,2.2));
#33017=CARTESIAN_POINT('',(25.5,-5.5,2.8));
#33018=CARTESIAN_POINT('',(25.5,-5.5,2.2));
#33019=CARTESIAN_POINT('',(26.,-5.,2.2));
#33020=CARTESIAN_POINT('Origin',(26.,-5.5,2.2));
#33021=CARTESIAN_POINT('',(26.,-5.,2.8));
#33022=CARTESIAN_POINT('',(26.,-5.,2.2));
#33023=CARTESIAN_POINT('Origin',(26.,-5.5,2.8));
#33024=CARTESIAN_POINT('Origin',(1.,-5.5,2.2));
#33025=CARTESIAN_POINT('',(0.5,-5.5,2.2));
#33026=CARTESIAN_POINT('',(0.5,-5.5,2.8));
#33027=CARTESIAN_POINT('',(0.5,-5.5,2.2));
#33028=CARTESIAN_POINT('',(1.,-5.,2.2));
#33029=CARTESIAN_POINT('Origin',(1.,-5.5,2.2));
#33030=CARTESIAN_POINT('',(1.,-5.,2.8));
#33031=CARTESIAN_POINT('',(1.,-5.,2.2));
#33032=CARTESIAN_POINT('Origin',(1.,-5.5,2.8));
#33033=CARTESIAN_POINT('Origin',(16.5,-6.,1.1));
#33034=CARTESIAN_POINT('',(16.335,-6.,1.2));
#33035=CARTESIAN_POINT('Origin',(16.5,-6.,1.2));
#33036=CARTESIAN_POINT('',(16.335,-6.,2.8));
#33037=CARTESIAN_POINT('',(16.335,-6.,1.1));
#33038=CARTESIAN_POINT('Origin',(16.5,-6.,2.8));
#33039=CARTESIAN_POINT('Origin',(10.5,-6.,1.1));
#33040=CARTESIAN_POINT('',(10.335,-6.,1.2));
#33041=CARTESIAN_POINT('Origin',(10.5,-6.,1.2));
#33042=CARTESIAN_POINT('',(10.335,-6.,2.8));
#33043=CARTESIAN_POINT('',(10.335,-6.,1.1));
#33044=CARTESIAN_POINT('Origin',(10.5,-6.,2.8));
#33045=CARTESIAN_POINT('Origin',(4.5,-6.,1.1));
#33046=CARTESIAN_POINT('',(4.335,-6.,1.2));
#33047=CARTESIAN_POINT('Origin',(4.5,-6.,1.2));
#33048=CARTESIAN_POINT('',(4.335,-6.,2.8));
#33049=CARTESIAN_POINT('',(4.335,-6.,1.1));
#33050=CARTESIAN_POINT('Origin',(4.5,-6.,2.8));
#33051=CARTESIAN_POINT('Origin',(22.5,-6.,1.1));
#33052=CARTESIAN_POINT('',(22.335,-6.,1.2));
#33053=CARTESIAN_POINT('Origin',(22.5,-6.,1.2));
#33054=CARTESIAN_POINT('',(22.335,-6.,2.8));
#33055=CARTESIAN_POINT('',(22.335,-6.,1.1));
#33056=CARTESIAN_POINT('Origin',(22.5,-6.,2.8));
#33057=CARTESIAN_POINT('Origin',(26.,-7.8,2.2));
#33058=CARTESIAN_POINT('',(25.5,-7.8,2.2));
#33059=CARTESIAN_POINT('Origin',(26.,-7.8,2.2));
#33060=CARTESIAN_POINT('',(25.5,-7.8,2.8));
#33061=CARTESIAN_POINT('',(25.5,-7.8,2.2));
#33062=CARTESIAN_POINT('Origin',(26.,-7.8,2.8));
#33063=CARTESIAN_POINT('Origin',(26.,-7.8,2.2));
#33064=CARTESIAN_POINT('',(25.725,-7.8,2.2));
#33065=CARTESIAN_POINT('Origin',(26.,-7.8,2.2));
#33066=CARTESIAN_POINT('Origin',(1.,-5.5,2.2));
#33067=CARTESIAN_POINT('Origin',(1.,-5.5,2.8));
#33068=CARTESIAN_POINT('',(1.,-5.,2.2));
#33069=CARTESIAN_POINT('Origin',(1.,-5.5,2.2));
#33070=CARTESIAN_POINT('Origin',(1.,-5.5,2.2));
#33071=CARTESIAN_POINT('',(0.725,-5.5,2.2));
#33072=CARTESIAN_POINT('Origin',(1.,-5.5,2.2));
#33073=CARTESIAN_POINT('Origin',(1.,-7.8,2.2));
#33074=CARTESIAN_POINT('',(0.5,-7.8,2.2));
#33075=CARTESIAN_POINT('Origin',(1.,-7.8,2.2));
#33076=CARTESIAN_POINT('',(0.5,-7.8,2.8));
#33077=CARTESIAN_POINT('',(0.5,-7.8,2.2));
#33078=CARTESIAN_POINT('Origin',(1.,-7.8,2.8));
#33079=CARTESIAN_POINT('Origin',(1.,-7.8,2.2));
#33080=CARTESIAN_POINT('',(0.725,-7.8,2.2));
#33081=CARTESIAN_POINT('Origin',(1.,-7.8,2.2));
#33082=CARTESIAN_POINT('Origin',(26.,-5.5,2.2));
#33083=CARTESIAN_POINT('Origin',(26.,-5.5,2.8));
#33084=CARTESIAN_POINT('',(26.,-5.,2.2));
#33085=CARTESIAN_POINT('Origin',(26.,-5.5,2.2));
#33086=CARTESIAN_POINT('Origin',(26.,-5.5,2.2));
#33087=CARTESIAN_POINT('',(25.725,-5.5,2.2));
#33088=CARTESIAN_POINT('Origin',(26.,-5.5,2.2));
#33089=CARTESIAN_POINT('Origin',(13.5,-6.75,2.8));
#33090=CARTESIAN_POINT('',(0.,-5.,2.8));
#33091=CARTESIAN_POINT('',(0.,-8.5,2.8));
#33092=CARTESIAN_POINT('',(0.,-5.,2.8));
#33093=CARTESIAN_POINT('',(27.,-8.5,2.8));
#33094=CARTESIAN_POINT('',(0.,-8.5,2.8));
#33095=CARTESIAN_POINT('',(27.,-5.,2.8));
#33096=CARTESIAN_POINT('',(27.,-8.5,2.8));
#33097=CARTESIAN_POINT('',(27.,-5.,2.8));
#33098=CARTESIAN_POINT('',(27.,-5.,2.8));
#33099=CARTESIAN_POINT('',(27.,-5.,2.8));
#33100=CARTESIAN_POINT('Origin',(26.,-7.8,1.1));
#33101=CARTESIAN_POINT('',(25.725,-7.8,1.2));
#33102=CARTESIAN_POINT('Origin',(26.,-7.8,1.2));
#33103=CARTESIAN_POINT('',(25.725,-7.8,1.1));
#33104=CARTESIAN_POINT('Origin',(1.,-5.5,1.1));
#33105=CARTESIAN_POINT('',(0.725,-5.5,1.2));
#33106=CARTESIAN_POINT('Origin',(1.,-5.5,1.2));
#33107=CARTESIAN_POINT('',(0.725,-5.5,1.1));
#33108=CARTESIAN_POINT('Origin',(1.,-7.8,1.1));
#33109=CARTESIAN_POINT('',(0.725,-7.8,1.2));
#33110=CARTESIAN_POINT('Origin',(1.,-7.8,1.2));
#33111=CARTESIAN_POINT('',(0.725,-7.8,1.1));
#33112=CARTESIAN_POINT('Origin',(26.,-5.5,1.1));
#33113=CARTESIAN_POINT('',(25.725,-5.5,1.2));
#33114=CARTESIAN_POINT('Origin',(26.,-5.5,1.2));
#33115=CARTESIAN_POINT('',(25.725,-5.5,1.1));
#33116=CARTESIAN_POINT('Origin',(27.,-5.,1.2));
#33117=CARTESIAN_POINT('',(27.,-5.,1.2));
#33118=CARTESIAN_POINT('',(0.,-5.,1.2));
#33119=CARTESIAN_POINT('',(27.,-5.,1.2));
#33120=CARTESIAN_POINT('',(0.,-5.,1.2));
#33121=CARTESIAN_POINT('',(27.,-5.,1.2));
#33122=CARTESIAN_POINT('Origin',(27.,-8.5,1.2));
#33123=CARTESIAN_POINT('',(27.,-8.5,1.2));
#33124=CARTESIAN_POINT('',(27.,-8.5,1.2));
#33125=CARTESIAN_POINT('',(27.,-8.5,1.2));
#33126=CARTESIAN_POINT('Origin',(0.,-8.5,1.2));
#33127=CARTESIAN_POINT('',(0.,-8.5,1.2));
#33128=CARTESIAN_POINT('',(0.,-8.5,1.2));
#33129=CARTESIAN_POINT('',(0.,-8.5,1.2));
#33130=CARTESIAN_POINT('Origin',(0.,-5.,1.2));
#33131=CARTESIAN_POINT('',(0.,-5.,1.2));
#33132=CARTESIAN_POINT('Origin',(13.5,-6.75,1.2));
#33133=CARTESIAN_POINT('',(0.,0.,0.));
#33134=CARTESIAN_POINT('Origin',(1.9,-2.1,4.));
#33135=CARTESIAN_POINT('',(2.,-2.1,4.165));
#33136=CARTESIAN_POINT('Origin',(2.,-2.1,4.));
#33137=CARTESIAN_POINT('',(4.,-2.1,4.165));
#33138=CARTESIAN_POINT('',(1.9,-2.1,4.165));
#33139=CARTESIAN_POINT('Origin',(4.,-2.1,4.));
#33140=CARTESIAN_POINT('Origin',(1.9,2.1,4.));
#33141=CARTESIAN_POINT('',(2.,2.1,4.165));
#33142=CARTESIAN_POINT('Origin',(2.,2.1,4.));
#33143=CARTESIAN_POINT('',(4.,2.1,4.165));
#33144=CARTESIAN_POINT('',(1.9,2.1,4.165));
#33145=CARTESIAN_POINT('Origin',(4.,2.1,4.));
#33146=CARTESIAN_POINT('Origin',(1.9,0.,6.1));
#33147=CARTESIAN_POINT('',(2.,-2.02066721859313E-17,6.265));
#33148=CARTESIAN_POINT('Origin',(2.,0.,6.1));
#33149=CARTESIAN_POINT('',(4.,2.02066721859313E-17,6.265));
#33150=CARTESIAN_POINT('',(1.9,-2.02066721859313E-17,6.265));
#33151=CARTESIAN_POINT('Origin',(4.,0.,6.1));
#33152=CARTESIAN_POINT('Origin',(1.9,0.,4.));
#33153=CARTESIAN_POINT('',(2.,-1.95943487863577E-16,5.6));
#33154=CARTESIAN_POINT('Origin',(2.,0.,4.));
#33155=CARTESIAN_POINT('',(3.5,-1.95943487863577E-16,5.6));
#33156=CARTESIAN_POINT('',(1.9,-1.95943487863577E-16,5.6));
#33157=CARTESIAN_POINT('Origin',(3.5,0.,4.));
#33158=CARTESIAN_POINT('Origin',(3.5,0.,4.));
#33159=CARTESIAN_POINT('',(3.5,1.71450551880629E-16,5.4));
#33160=CARTESIAN_POINT('Origin',(3.5,0.,4.));
#33161=CARTESIAN_POINT('Origin',(1.9,0.,4.));
#33162=CARTESIAN_POINT('',(4.,1.71450551880629E-16,5.4));
#33163=CARTESIAN_POINT('',(1.9,-1.71450551880629E-16,5.4));
#33164=CARTESIAN_POINT('Origin',(4.,0.,4.));
#33165=CARTESIAN_POINT('Origin',(3.,-2.4,1.1));
#33166=CARTESIAN_POINT('',(2.79,-2.4,1.2));
#33167=CARTESIAN_POINT('Origin',(3.,-2.4,1.2));
#33168=CARTESIAN_POINT('',(2.79,-2.4,2.9));
#33169=CARTESIAN_POINT('',(2.79,-2.4,1.1));
#33170=CARTESIAN_POINT('Origin',(3.,-2.4,2.9));
#33171=CARTESIAN_POINT('Origin',(3.,-2.4,2.9));
#33172=CARTESIAN_POINT('Origin',(3.,2.4,1.1));
#33173=CARTESIAN_POINT('',(2.79,2.4,1.2));
#33174=CARTESIAN_POINT('Origin',(3.,2.4,1.2));
#33175=CARTESIAN_POINT('',(2.79,2.4,2.9));
#33176=CARTESIAN_POINT('',(2.79,2.4,1.1));
#33177=CARTESIAN_POINT('Origin',(3.,2.4,2.9));
#33178=CARTESIAN_POINT('Origin',(3.,2.4,2.9));
#33179=CARTESIAN_POINT('Origin',(4.,3.,1.2));
#33180=CARTESIAN_POINT('',(4.,3.,1.2));
#33181=CARTESIAN_POINT('',(2.,3.,1.2));
#33182=CARTESIAN_POINT('',(4.,3.,1.2));
#33183=CARTESIAN_POINT('',(2.,3.,7.));
#33184=CARTESIAN_POINT('',(2.,3.,1.2));
#33185=CARTESIAN_POINT('',(4.,3.,7.));
#33186=CARTESIAN_POINT('',(4.,3.,7.));
#33187=CARTESIAN_POINT('',(4.,3.,1.2));
#33188=CARTESIAN_POINT('Origin',(4.,-3.,1.2));
#33189=CARTESIAN_POINT('',(4.,-3.,1.2));
#33190=CARTESIAN_POINT('',(4.,-3.,1.2));
#33191=CARTESIAN_POINT('',(4.,-3.,7.));
#33192=CARTESIAN_POINT('',(4.,-3.,7.));
#33193=CARTESIAN_POINT('',(4.,-3.,1.2));
#33194=CARTESIAN_POINT('Origin',(2.,-3.,1.2));
#33195=CARTESIAN_POINT('',(2.,-3.,1.2));
#33196=CARTESIAN_POINT('',(2.,-3.,1.2));
#33197=CARTESIAN_POINT('',(2.,-3.,7.));
#33198=CARTESIAN_POINT('',(2.,-3.,7.));
#33199=CARTESIAN_POINT('',(2.,-3.,1.2));
#33200=CARTESIAN_POINT('Origin',(2.,3.,1.2));
#33201=CARTESIAN_POINT('',(2.,3.,1.2));
#33202=CARTESIAN_POINT('',(2.,3.,7.));
#33203=CARTESIAN_POINT('Origin',(3.,0.,7.));
#33204=CARTESIAN_POINT('Origin',(3.,0.,1.2));
#33205=CARTESIAN_POINT('',(0.,0.,0.));
#33206=CARTESIAN_POINT('Origin',(1.5,-2.1,4.));
#33207=CARTESIAN_POINT('',(1.6,-2.1,4.225));
#33208=CARTESIAN_POINT('Origin',(1.6,-2.1,4.));
#33209=CARTESIAN_POINT('',(2.,-2.1,4.225));
#33210=CARTESIAN_POINT('',(1.5,-2.1,4.225));
#33211=CARTESIAN_POINT('Origin',(2.,-2.1,4.));
#33212=CARTESIAN_POINT('Origin',(1.5,2.1,4.));
#33213=CARTESIAN_POINT('',(1.6,2.1,4.225));
#33214=CARTESIAN_POINT('Origin',(1.6,2.1,4.));
#33215=CARTESIAN_POINT('',(2.,2.1,4.225));
#33216=CARTESIAN_POINT('',(1.5,2.1,4.225));
#33217=CARTESIAN_POINT('Origin',(2.,2.1,4.));
#33218=CARTESIAN_POINT('Origin',(1.5,0.,6.1));
#33219=CARTESIAN_POINT('',(1.6,-2.75545529808154E-17,6.325));
#33220=CARTESIAN_POINT('Origin',(1.6,0.,6.1));
#33221=CARTESIAN_POINT('',(2.,2.75545529808154E-17,6.325));
#33222=CARTESIAN_POINT('',(1.5,-2.75545529808154E-17,6.325));
#33223=CARTESIAN_POINT('Origin',(2.,0.,6.1));
#33224=CARTESIAN_POINT('Origin',(2.,0.,4.));
#33225=CARTESIAN_POINT('',(2.5,-1.94718841064429E-16,5.59));
#33226=CARTESIAN_POINT('Origin',(2.5,0.,4.));
#33227=CARTESIAN_POINT('',(2.,-1.94718841064429E-16,5.59));
#33228=CARTESIAN_POINT('',(2.,-1.94718841064429E-16,5.59));
#33229=CARTESIAN_POINT('Origin',(2.,0.,4.));
#33230=CARTESIAN_POINT('Origin',(2.5,0.,4.));
#33231=CARTESIAN_POINT('',(2.5,-1.46957615897682E-16,5.2));
#33232=CARTESIAN_POINT('Origin',(2.5,0.,4.));
#33233=CARTESIAN_POINT('Origin',(1.6,0.,4.));
#33234=CARTESIAN_POINT('',(1.6,-1.46957615897682E-16,5.2));
#33235=CARTESIAN_POINT('',(1.6,-1.46957615897682E-16,5.2));
#33236=CARTESIAN_POINT('Origin',(1.6,0.,4.));
#33237=CARTESIAN_POINT('Origin',(1.6,0.,4.));
#33238=CARTESIAN_POINT('',(2.,-2.93915231795365E-16,6.4));
#33239=CARTESIAN_POINT('Origin',(2.,0.,4.));
#33240=CARTESIAN_POINT('',(1.6,-2.93915231795365E-16,6.4));
#33241=CARTESIAN_POINT('',(1.6,-2.93915231795365E-16,6.4));
#33242=CARTESIAN_POINT('Origin',(1.6,0.,4.));
#33243=CARTESIAN_POINT('Origin',(2.,0.,4.));
#33244=CARTESIAN_POINT('Origin',(1.6,0.,4.));
#33245=CARTESIAN_POINT('',(0.,0.,0.));
#33246=CARTESIAN_POINT('Origin',(22.9,-2.6,4.));
#33247=CARTESIAN_POINT('',(23.,-2.6,4.165));
#33248=CARTESIAN_POINT('Origin',(23.,-2.6,4.));
#33249=CARTESIAN_POINT('',(25.,-2.6,4.165));
#33250=CARTESIAN_POINT('',(22.9,-2.6,4.165));
#33251=CARTESIAN_POINT('Origin',(25.,-2.6,4.));
#33252=CARTESIAN_POINT('Origin',(22.9,2.6,4.));
#33253=CARTESIAN_POINT('',(23.,2.6,4.165));
#33254=CARTESIAN_POINT('Origin',(23.,2.6,4.));
#33255=CARTESIAN_POINT('',(25.,2.6,4.165));
#33256=CARTESIAN_POINT('',(22.9,2.6,4.165));
#33257=CARTESIAN_POINT('Origin',(25.,2.6,4.));
#33258=CARTESIAN_POINT('Origin',(22.9,0.,6.6));
#33259=CARTESIAN_POINT('',(23.,-2.02066721859313E-17,6.765));
#33260=CARTESIAN_POINT('Origin',(23.,0.,6.6));
#33261=CARTESIAN_POINT('',(25.,2.02066721859313E-17,6.765));
#33262=CARTESIAN_POINT('',(22.9,-2.02066721859313E-17,6.765));
#33263=CARTESIAN_POINT('Origin',(25.,0.,6.6));
#33264=CARTESIAN_POINT('Origin',(23.3,0.,4.));
#33265=CARTESIAN_POINT('',(23.3,-2.87791997799628E-16,6.35));
#33266=CARTESIAN_POINT('Origin',(23.3,0.,4.));
#33267=CARTESIAN_POINT('',(25.,2.87791997799628E-16,6.35));
#33268=CARTESIAN_POINT('',(23.3,-2.87791997799628E-16,6.35));
#33269=CARTESIAN_POINT('Origin',(25.,0.,4.));
#33270=CARTESIAN_POINT('Origin',(23.3,0.,4.));
#33271=CARTESIAN_POINT('',(23.3,-2.63299061816681E-16,6.15));
#33272=CARTESIAN_POINT('Origin',(23.3,0.,4.));
#33273=CARTESIAN_POINT('Origin',(22.9,0.,4.));
#33274=CARTESIAN_POINT('',(23.,-2.63299061816681E-16,6.15));
#33275=CARTESIAN_POINT('Origin',(23.,0.,4.));
#33276=CARTESIAN_POINT('',(22.9,-2.63299061816681E-16,6.15));
#33277=CARTESIAN_POINT('Origin',(24.,-3.5,1.1));
#33278=CARTESIAN_POINT('',(23.75,-3.5,1.2));
#33279=CARTESIAN_POINT('Origin',(24.,-3.5,1.2));
#33280=CARTESIAN_POINT('',(23.75,-3.5,2.9));
#33281=CARTESIAN_POINT('',(23.75,-3.5,1.1));
#33282=CARTESIAN_POINT('Origin',(24.,-3.5,2.9));
#33283=CARTESIAN_POINT('Origin',(24.,-3.5,2.9));
#33284=CARTESIAN_POINT('Origin',(24.,3.5,1.1));
#33285=CARTESIAN_POINT('',(23.75,3.5,1.2));
#33286=CARTESIAN_POINT('Origin',(24.,3.5,1.2));
#33287=CARTESIAN_POINT('',(23.75,3.5,2.9));
#33288=CARTESIAN_POINT('',(23.75,3.5,1.1));
#33289=CARTESIAN_POINT('Origin',(24.,3.5,2.9));
#33290=CARTESIAN_POINT('Origin',(24.,3.5,2.9));
#33291=CARTESIAN_POINT('Origin',(25.,5.,1.2));
#33292=CARTESIAN_POINT('',(25.,5.,1.2));
#33293=CARTESIAN_POINT('',(23.,5.,1.2));
#33294=CARTESIAN_POINT('',(25.,5.,1.2));
#33295=CARTESIAN_POINT('',(23.,5.,7.));
#33296=CARTESIAN_POINT('',(23.,5.,1.2));
#33297=CARTESIAN_POINT('',(25.,5.,7.));
#33298=CARTESIAN_POINT('',(25.,5.,7.));
#33299=CARTESIAN_POINT('',(25.,5.,1.2));
#33300=CARTESIAN_POINT('Origin',(25.,-5.,1.2));
#33301=CARTESIAN_POINT('',(25.,-5.,1.2));
#33302=CARTESIAN_POINT('',(25.,-5.,1.2));
#33303=CARTESIAN_POINT('',(25.,-5.,7.));
#33304=CARTESIAN_POINT('',(25.,-5.,7.));
#33305=CARTESIAN_POINT('',(25.,-5.,1.2));
#33306=CARTESIAN_POINT('Origin',(23.,-5.,1.2));
#33307=CARTESIAN_POINT('',(23.,-5.,1.2));
#33308=CARTESIAN_POINT('',(23.,-5.,1.2));
#33309=CARTESIAN_POINT('',(23.,-5.,7.));
#33310=CARTESIAN_POINT('',(23.,-5.,7.));
#33311=CARTESIAN_POINT('',(23.,-5.,1.2));
#33312=CARTESIAN_POINT('Origin',(23.,5.,1.2));
#33313=CARTESIAN_POINT('',(23.,5.,1.2));
#33314=CARTESIAN_POINT('',(23.,5.,7.));
#33315=CARTESIAN_POINT('Origin',(24.,0.,7.));
#33316=CARTESIAN_POINT('Origin',(24.,0.,1.2));
#33317=CARTESIAN_POINT('',(0.,0.,0.));
#33318=CARTESIAN_POINT('Origin',(24.9,-2.6,4.));
#33319=CARTESIAN_POINT('',(25.,-2.6,4.225));
#33320=CARTESIAN_POINT('Origin',(25.,-2.6,4.));
#33321=CARTESIAN_POINT('',(25.4,-2.6,4.225));
#33322=CARTESIAN_POINT('',(24.9,-2.6,4.225));
#33323=CARTESIAN_POINT('Origin',(25.4,-2.6,4.));
#33324=CARTESIAN_POINT('Origin',(24.9,2.6,4.));
#33325=CARTESIAN_POINT('',(25.,2.6,4.225));
#33326=CARTESIAN_POINT('Origin',(25.,2.6,4.));
#33327=CARTESIAN_POINT('',(25.4,2.6,4.225));
#33328=CARTESIAN_POINT('',(24.9,2.6,4.225));
#33329=CARTESIAN_POINT('Origin',(25.4,2.6,4.));
#33330=CARTESIAN_POINT('Origin',(24.9,0.,6.6));
#33331=CARTESIAN_POINT('',(25.,-2.75545529808154E-17,6.825));
#33332=CARTESIAN_POINT('Origin',(25.,0.,6.6));
#33333=CARTESIAN_POINT('',(25.4,2.75545529808154E-17,6.825));
#33334=CARTESIAN_POINT('',(24.9,-2.75545529808154E-17,6.825));
#33335=CARTESIAN_POINT('Origin',(25.4,0.,6.6));
#33336=CARTESIAN_POINT('Origin',(24.9,3.5,1.22));
#33337=CARTESIAN_POINT('',(25.,-1.12765242872084,1.22));
#33338=CARTESIAN_POINT('',(25.4,-1.12765242872084,1.22));
#33339=CARTESIAN_POINT('',(25.,-1.12765242872084,1.22));
#33340=CARTESIAN_POINT('',(25.,1.12765242872084,1.22));
#33341=CARTESIAN_POINT('',(25.,1.75,1.22));
#33342=CARTESIAN_POINT('',(25.4,1.12765242872084,1.22));
#33343=CARTESIAN_POINT('',(25.,1.12765242872084,1.22));
#33344=CARTESIAN_POINT('',(25.4,1.75,1.22));
#33345=CARTESIAN_POINT('Origin',(25.,0.,4.));
#33346=CARTESIAN_POINT('Origin',(25.,0.,4.));
#33347=CARTESIAN_POINT('',(25.,-2.86567351000481E-16,6.34));
#33348=CARTESIAN_POINT('Origin',(25.,0.,4.));
#33349=CARTESIAN_POINT('Origin',(25.,0.,4.));
#33350=CARTESIAN_POINT('Origin',(25.4,0.,4.));
#33351=CARTESIAN_POINT('Origin',(24.7,0.,4.));
#33352=CARTESIAN_POINT('',(24.7,-2.86567351000481E-16,6.34));
#33353=CARTESIAN_POINT('',(24.7,-2.86567351000481E-16,6.34));
#33354=CARTESIAN_POINT('Origin',(24.7,0.,4.));
#33355=CARTESIAN_POINT('Origin',(24.7,0.,4.));
#33356=CARTESIAN_POINT('',(24.7,-2.20436423846524E-16,5.8));
#33357=CARTESIAN_POINT('Origin',(24.7,0.,4.));
#33358=CARTESIAN_POINT('Origin',(25.,0.,4.));
#33359=CARTESIAN_POINT('',(25.4,-2.20436423846524E-16,5.8));
#33360=CARTESIAN_POINT('Origin',(25.4,0.,4.));
#33361=CARTESIAN_POINT('',(25.,-2.20436423846524E-16,5.8));
#33362=CARTESIAN_POINT('Origin',(25.4,0.,4.));
#33363=CARTESIAN_POINT('',(0.,0.,0.));
#33364=CARTESIAN_POINT('Origin',(3.5,-9.25,2.4));
#33365=CARTESIAN_POINT('',(3.025,-9.25,2.4));
#33366=CARTESIAN_POINT('Origin',(3.5,-9.25,2.4));
#33367=CARTESIAN_POINT('',(3.025,-9.25,7.));
#33368=CARTESIAN_POINT('',(3.025,-9.25,2.4));
#33369=CARTESIAN_POINT('Origin',(3.5,-9.25,7.));
#33370=CARTESIAN_POINT('Origin',(3.5,-9.25,2.4));
#33371=CARTESIAN_POINT('',(3.225,-9.25,2.4));
#33372=CARTESIAN_POINT('Origin',(3.5,-9.25,2.4));
#33373=CARTESIAN_POINT('Origin',(3.5,-9.25,1.1));
#33374=CARTESIAN_POINT('',(3.225,-9.25,1.2));
#33375=CARTESIAN_POINT('Origin',(3.5,-9.25,1.2));
#33376=CARTESIAN_POINT('',(3.225,-9.25,1.1));
#33377=CARTESIAN_POINT('Origin',(4.,-8.5,1.2));
#33378=CARTESIAN_POINT('',(4.,-8.5,1.2));
#33379=CARTESIAN_POINT('',(3.,-8.5,1.2));
#33380=CARTESIAN_POINT('',(4.,-8.5,1.2));
#33381=CARTESIAN_POINT('',(3.,-8.5,7.));
#33382=CARTESIAN_POINT('',(3.,-8.5,1.2));
#33383=CARTESIAN_POINT('',(4.,-8.5,7.));
#33384=CARTESIAN_POINT('',(4.,-8.5,7.));
#33385=CARTESIAN_POINT('',(4.,-8.5,1.2));
#33386=CARTESIAN_POINT('Origin',(4.,-10.,1.2));
#33387=CARTESIAN_POINT('',(4.,-10.,1.2));
#33388=CARTESIAN_POINT('',(4.,-10.,1.2));
#33389=CARTESIAN_POINT('',(4.,-10.,7.));
#33390=CARTESIAN_POINT('',(4.,-10.,7.));
#33391=CARTESIAN_POINT('',(4.,-10.,1.2));
#33392=CARTESIAN_POINT('Origin',(3.,-10.,1.2));
#33393=CARTESIAN_POINT('',(3.,-10.,1.2));
#33394=CARTESIAN_POINT('',(3.,-10.,1.2));
#33395=CARTESIAN_POINT('',(3.,-10.,7.));
#33396=CARTESIAN_POINT('',(3.,-10.,7.));
#33397=CARTESIAN_POINT('',(3.,-10.,1.2));
#33398=CARTESIAN_POINT('Origin',(3.,-8.5,1.2));
#33399=CARTESIAN_POINT('',(3.,-8.5,1.2));
#33400=CARTESIAN_POINT('',(3.,-8.5,7.));
#33401=CARTESIAN_POINT('Origin',(3.5,-9.25,7.));
#33402=CARTESIAN_POINT('Origin',(3.5,-9.25,1.2));
#33403=CARTESIAN_POINT('',(0.,0.,0.));
#33404=CARTESIAN_POINT('Origin',(23.5,-9.25,2.4));
#33405=CARTESIAN_POINT('',(23.025,-9.25,2.4));
#33406=CARTESIAN_POINT('Origin',(23.5,-9.25,2.4));
#33407=CARTESIAN_POINT('',(23.025,-9.25,7.));
#33408=CARTESIAN_POINT('',(23.025,-9.25,2.4));
#33409=CARTESIAN_POINT('Origin',(23.5,-9.25,7.));
#33410=CARTESIAN_POINT('Origin',(23.5,-9.25,2.4));
#33411=CARTESIAN_POINT('',(23.225,-9.25,2.4));
#33412=CARTESIAN_POINT('Origin',(23.5,-9.25,2.4));
#33413=CARTESIAN_POINT('Origin',(23.5,-9.25,1.1));
#33414=CARTESIAN_POINT('',(23.225,-9.25,1.2));
#33415=CARTESIAN_POINT('Origin',(23.5,-9.25,1.2));
#33416=CARTESIAN_POINT('',(23.225,-9.25,1.1));
#33417=CARTESIAN_POINT('Origin',(24.,-8.5,1.2));
#33418=CARTESIAN_POINT('',(24.,-8.5,1.2));
#33419=CARTESIAN_POINT('',(23.,-8.5,1.2));
#33420=CARTESIAN_POINT('',(24.,-8.5,1.2));
#33421=CARTESIAN_POINT('',(23.,-8.5,7.));
#33422=CARTESIAN_POINT('',(23.,-8.5,1.2));
#33423=CARTESIAN_POINT('',(24.,-8.5,7.));
#33424=CARTESIAN_POINT('',(24.,-8.5,7.));
#33425=CARTESIAN_POINT('',(24.,-8.5,1.2));
#33426=CARTESIAN_POINT('Origin',(24.,-10.,1.2));
#33427=CARTESIAN_POINT('',(24.,-10.,1.2));
#33428=CARTESIAN_POINT('',(24.,-10.,1.2));
#33429=CARTESIAN_POINT('',(24.,-10.,7.));
#33430=CARTESIAN_POINT('',(24.,-10.,7.));
#33431=CARTESIAN_POINT('',(24.,-10.,1.2));
#33432=CARTESIAN_POINT('Origin',(23.,-10.,1.2));
#33433=CARTESIAN_POINT('',(23.,-10.,1.2));
#33434=CARTESIAN_POINT('',(23.,-10.,1.2));
#33435=CARTESIAN_POINT('',(23.,-10.,7.));
#33436=CARTESIAN_POINT('',(23.,-10.,7.));
#33437=CARTESIAN_POINT('',(23.,-10.,1.2));
#33438=CARTESIAN_POINT('Origin',(23.,-8.5,1.2));
#33439=CARTESIAN_POINT('',(23.,-8.5,1.2));
#33440=CARTESIAN_POINT('',(23.,-8.5,7.));
#33441=CARTESIAN_POINT('Origin',(23.5,-9.25,7.));
#33442=CARTESIAN_POINT('Origin',(23.5,-9.25,1.2));
#33443=CARTESIAN_POINT('',(0.,0.,0.));
#33444=CARTESIAN_POINT('Origin',(14.,0.,0.97));
#33445=CARTESIAN_POINT('',(13.625,-4.59242549680257E-17,0.97));
#33446=CARTESIAN_POINT('Origin',(14.,0.,0.97));
#33447=CARTESIAN_POINT('',(13.625,4.59242549680257E-17,1.5));
#33448=CARTESIAN_POINT('',(13.625,-4.59242549680257E-17,0.97));
#33449=CARTESIAN_POINT('Origin',(14.,0.,1.5));
#33450=CARTESIAN_POINT('Origin',(14.,0.,0.97));
#33451=CARTESIAN_POINT('',(13.775,-2.75545529808154E-17,0.97));
#33452=CARTESIAN_POINT('Origin',(14.,0.,0.97));
#33453=CARTESIAN_POINT('Origin',(8.,0.,0.97));
#33454=CARTESIAN_POINT('',(7.625,-4.59242549680257E-17,0.97));
#33455=CARTESIAN_POINT('Origin',(8.,0.,0.97));
#33456=CARTESIAN_POINT('',(7.625,4.59242549680257E-17,1.5));
#33457=CARTESIAN_POINT('',(7.625,-4.59242549680257E-17,0.97));
#33458=CARTESIAN_POINT('Origin',(8.,0.,1.5));
#33459=CARTESIAN_POINT('Origin',(8.,0.,0.97));
#33460=CARTESIAN_POINT('',(7.775,-2.75545529808154E-17,0.97));
#33461=CARTESIAN_POINT('Origin',(8.,0.,0.97));
#33462=CARTESIAN_POINT('Origin',(2.,0.,0.97));
#33463=CARTESIAN_POINT('',(1.625,-4.59242549680257E-17,0.97));
#33464=CARTESIAN_POINT('Origin',(2.,0.,0.97));
#33465=CARTESIAN_POINT('',(1.625,4.59242549680257E-17,1.5));
#33466=CARTESIAN_POINT('',(1.625,-4.59242549680257E-17,0.97));
#33467=CARTESIAN_POINT('Origin',(2.,0.,1.5));
#33468=CARTESIAN_POINT('Origin',(2.,0.,0.97));
#33469=CARTESIAN_POINT('',(1.775,-2.75545529808155E-17,0.97));
#33470=CARTESIAN_POINT('Origin',(2.,0.,0.97));
#33471=CARTESIAN_POINT('Origin',(20.,0.,0.97));
#33472=CARTESIAN_POINT('',(19.625,-4.59242549680257E-17,0.97));
#33473=CARTESIAN_POINT('Origin',(20.,0.,0.97));
#33474=CARTESIAN_POINT('',(19.625,4.59242549680257E-17,1.5));
#33475=CARTESIAN_POINT('',(19.625,-4.59242549680257E-17,0.97));
#33476=CARTESIAN_POINT('Origin',(20.,0.,1.5));
#33477=CARTESIAN_POINT('Origin',(20.,0.,0.97));
#33478=CARTESIAN_POINT('',(19.775,-2.75545529808156E-17,0.97));
#33479=CARTESIAN_POINT('Origin',(20.,0.,0.97));
#33480=CARTESIAN_POINT('Origin',(14.,0.,-0.1));
#33481=CARTESIAN_POINT('',(13.775,-2.75545529808154E-17,0.));
#33482=CARTESIAN_POINT('Origin',(14.,0.,0.));
#33483=CARTESIAN_POINT('',(13.775,-2.75545529808154E-17,-0.1));
#33484=CARTESIAN_POINT('Origin',(8.,0.,-0.1));
#33485=CARTESIAN_POINT('',(7.775,-2.75545529808154E-17,0.));
#33486=CARTESIAN_POINT('Origin',(8.,0.,0.));
#33487=CARTESIAN_POINT('',(7.775,-2.75545529808154E-17,-0.1));
#33488=CARTESIAN_POINT('Origin',(2.,0.,-0.1));
#33489=CARTESIAN_POINT('',(1.775,-2.75545529808155E-17,0.));
#33490=CARTESIAN_POINT('Origin',(2.,0.,0.));
#33491=CARTESIAN_POINT('',(1.775,-2.75545529808155E-17,-0.1));
#33492=CARTESIAN_POINT('Origin',(20.,0.,-0.1));
#33493=CARTESIAN_POINT('',(19.775,-2.75545529808156E-17,0.));
#33494=CARTESIAN_POINT('Origin',(20.,0.,0.));
#33495=CARTESIAN_POINT('',(19.775,-2.75545529808156E-17,-0.1));
#33496=CARTESIAN_POINT('Origin',(0.,-0.53,1.));
#33497=CARTESIAN_POINT('',(0.,-0.53,1.));
#33498=CARTESIAN_POINT('',(0.,-0.75,0.85));
#33499=CARTESIAN_POINT('',(0.,-0.53,1.));
#33500=CARTESIAN_POINT('',(22.,-0.75,0.85));
#33501=CARTESIAN_POINT('',(0.,-0.75,0.85));
#33502=CARTESIAN_POINT('',(22.,-0.53,1.));
#33503=CARTESIAN_POINT('',(22.,-0.53,1.));
#33504=CARTESIAN_POINT('',(0.,-0.53,1.));
#33505=CARTESIAN_POINT('Origin',(0.,-0.53,1.15));
#33506=CARTESIAN_POINT('',(0.,-0.53,1.15));
#33507=CARTESIAN_POINT('',(0.,-0.53,1.15));
#33508=CARTESIAN_POINT('',(22.,-0.53,1.15));
#33509=CARTESIAN_POINT('',(22.,-0.53,1.15));
#33510=CARTESIAN_POINT('',(0.,-0.53,1.15));
#33511=CARTESIAN_POINT('Origin',(0.,-0.75,1.3));
#33512=CARTESIAN_POINT('',(0.,-0.75,1.3));
#33513=CARTESIAN_POINT('',(0.,-0.75,1.3));
#33514=CARTESIAN_POINT('',(22.,-0.75,1.3));
#33515=CARTESIAN_POINT('',(22.,-0.75,1.3));
#33516=CARTESIAN_POINT('',(0.,-0.75,1.3));
#33517=CARTESIAN_POINT('Origin',(0.,-0.75,1.5));
#33518=CARTESIAN_POINT('',(0.,-0.75,1.5));
#33519=CARTESIAN_POINT('',(0.,-0.75,1.5));
#33520=CARTESIAN_POINT('',(22.,-0.75,1.5));
#33521=CARTESIAN_POINT('',(22.,-0.75,1.5));
#33522=CARTESIAN_POINT('',(0.,-0.75,1.5));
#33523=CARTESIAN_POINT('Origin',(0.,0.75,1.5));
#33524=CARTESIAN_POINT('',(0.,0.75,1.5));
#33525=CARTESIAN_POINT('',(0.,0.75,1.5));
#33526=CARTESIAN_POINT('',(22.,0.75,1.5));
#33527=CARTESIAN_POINT('',(22.,0.75,1.5));
#33528=CARTESIAN_POINT('',(0.,0.75,1.5));
#33529=CARTESIAN_POINT('Origin',(0.,0.75,1.3));
#33530=CARTESIAN_POINT('',(0.,0.75,1.3));
#33531=CARTESIAN_POINT('',(0.,0.75,1.3));
#33532=CARTESIAN_POINT('',(22.,0.75,1.3));
#33533=CARTESIAN_POINT('',(22.,0.75,1.3));
#33534=CARTESIAN_POINT('',(0.,0.75,1.3));
#33535=CARTESIAN_POINT('Origin',(0.,0.53,1.15));
#33536=CARTESIAN_POINT('',(0.,0.53,1.15));
#33537=CARTESIAN_POINT('',(0.,0.53,1.15));
#33538=CARTESIAN_POINT('',(22.,0.53,1.15));
#33539=CARTESIAN_POINT('',(22.,0.53,1.15));
#33540=CARTESIAN_POINT('',(0.,0.53,1.15));
#33541=CARTESIAN_POINT('Origin',(0.,0.53,1.));
#33542=CARTESIAN_POINT('',(0.,0.53,1.));
#33543=CARTESIAN_POINT('',(0.,0.53,1.));
#33544=CARTESIAN_POINT('',(22.,0.53,1.));
#33545=CARTESIAN_POINT('',(22.,0.53,1.));
#33546=CARTESIAN_POINT('',(0.,0.53,1.));
#33547=CARTESIAN_POINT('Origin',(0.,0.75,0.85));
#33548=CARTESIAN_POINT('',(0.,0.75,0.85));
#33549=CARTESIAN_POINT('',(0.,0.75,0.85));
#33550=CARTESIAN_POINT('',(22.,0.75,0.85));
#33551=CARTESIAN_POINT('',(22.,0.75,0.85));
#33552=CARTESIAN_POINT('',(0.,0.75,0.85));
#33553=CARTESIAN_POINT('Origin',(0.,0.75,0.));
#33554=CARTESIAN_POINT('',(0.,0.75,0.));
#33555=CARTESIAN_POINT('',(0.,0.75,0.));
#33556=CARTESIAN_POINT('',(22.,0.75,0.));
#33557=CARTESIAN_POINT('',(22.,0.75,0.));
#33558=CARTESIAN_POINT('',(0.,0.75,0.));
#33559=CARTESIAN_POINT('Origin',(0.,-0.75,0.));
#33560=CARTESIAN_POINT('',(0.,-0.75,0.));
#33561=CARTESIAN_POINT('',(0.,-0.75,0.));
#33562=CARTESIAN_POINT('',(22.,-0.75,0.));
#33563=CARTESIAN_POINT('',(22.,-0.75,0.));
#33564=CARTESIAN_POINT('',(0.,-0.75,0.));
#33565=CARTESIAN_POINT('Origin',(0.,-0.75,0.85));
#33566=CARTESIAN_POINT('',(0.,-0.75,0.85));
#33567=CARTESIAN_POINT('',(22.,-0.75,0.85));
#33568=CARTESIAN_POINT('Origin',(22.,0.,0.75));
#33569=CARTESIAN_POINT('Origin',(0.,0.,0.75));
#33570=CARTESIAN_POINT('',(0.,0.,0.));
#33571=CARTESIAN_POINT('',(0.,0.,0.));
#33572=CARTESIAN_POINT('Origin',(0.,0.,0.));
#33573=CARTESIAN_POINT('',(-1.070235,-0.308121667383195,-1.31065986708547E-16));
#33574=CARTESIAN_POINT('',(-1.31065986708547E-16,-0.308121667383195,1.070235));
#33575=CARTESIAN_POINT('Origin',(0.,-0.308121667383195,0.));
#33576=CARTESIAN_POINT('Origin',(0.,-0.308121667383195,0.));
#33577=CARTESIAN_POINT('',(-1.31065986708547E-16,0.308121667383195,1.070235));
#33578=CARTESIAN_POINT('Origin',(-1.34711147906209E-16,0.,1.1));
#33579=CARTESIAN_POINT('',(-1.070235,0.308121667383195,1.31065986708547E-16));
#33580=CARTESIAN_POINT('Origin',(0.,0.308121667383195,0.));
#33581=CARTESIAN_POINT('Origin',(0.,0.308121667383195,0.));
#33582=CARTESIAN_POINT('Origin',(0.,0.,0.));
#33583=CARTESIAN_POINT('',(-1.070235,0.5,-1.31065986708547E-16));
#33584=CARTESIAN_POINT('',(-1.070235,0.,-1.31065986708547E-16));
#33585=CARTESIAN_POINT('Origin',(0.,0.5,0.));
#33586=CARTESIAN_POINT('Origin',(0.,0.,0.));
#33587=CARTESIAN_POINT('',(-0.6,-0.44,-7.34788079488412E-17));
#33588=CARTESIAN_POINT('Origin',(0.,-0.44,0.));
#33589=CARTESIAN_POINT('',(-0.6,0.44,-7.34788079488412E-17));
#33590=CARTESIAN_POINT('',(-0.6,0.,-7.34788079488412E-17));
#33591=CARTESIAN_POINT('Origin',(0.,0.44,0.));
#33592=CARTESIAN_POINT('Origin',(0.,0.47,0.));
#33593=CARTESIAN_POINT('',(-0.66,0.5,-8.08266887437253E-17));
#33594=CARTESIAN_POINT('',(-0.63,0.47,-7.71527483462832E-17));
#33595=CARTESIAN_POINT('Origin',(0.,0.5,0.));
#33596=CARTESIAN_POINT('Origin',(1.070235,0.5,0.));
#33597=CARTESIAN_POINT('Origin',(0.,0.,0.));
#33598=CARTESIAN_POINT('',(-1.070235,-0.5,-1.31065986708547E-16));
#33599=CARTESIAN_POINT('Origin',(0.,-0.5,0.));
#33600=CARTESIAN_POINT('',(-1.070235,0.,-1.31065986708547E-16));
#33601=CARTESIAN_POINT('Origin',(0.66,-0.5,0.));
#33602=CARTESIAN_POINT('',(-0.66,-0.5,-8.08266887437253E-17));
#33603=CARTESIAN_POINT('Origin',(0.,-0.5,0.));
#33604=CARTESIAN_POINT('Origin',(0.,-0.47,0.));
#33605=CARTESIAN_POINT('',(-0.63,-0.47,-7.71527483462832E-17));
#33606=CARTESIAN_POINT('',(0.,0.,0.));
#33607=CARTESIAN_POINT('Origin',(0.,0.,0.));
#33608=CARTESIAN_POINT('',(-1.129765,0.308121667383195,-1.38356309103871E-16));
#33609=CARTESIAN_POINT('',(-1.38356309103871E-16,0.308121667383195,1.129765));
#33610=CARTESIAN_POINT('Origin',(0.,0.308121667383195,0.));
#33611=CARTESIAN_POINT('Origin',(0.,0.308121667383195,0.));
#33612=CARTESIAN_POINT('',(-1.38356309103871E-16,-0.308121667383195,1.129765));
#33613=CARTESIAN_POINT('Origin',(-1.34711147906209E-16,0.,1.1));
#33614=CARTESIAN_POINT('',(-1.129765,-0.308121667383195,1.38356309103871E-16));
#33615=CARTESIAN_POINT('Origin',(0.,-0.308121667383195,0.));
#33616=CARTESIAN_POINT('Origin',(0.,-0.308121667383195,0.));
#33617=CARTESIAN_POINT('Origin',(0.,0.,0.));
#33618=CARTESIAN_POINT('',(-1.129765,-0.5,-1.38356309103871E-16));
#33619=CARTESIAN_POINT('Origin',(0.,-0.5,0.));
#33620=CARTESIAN_POINT('',(-1.129765,0.,-1.38356309103871E-16));
#33621=CARTESIAN_POINT('Origin',(1.54,0.5,0.));
#33622=CARTESIAN_POINT('',(-1.54,0.5,-1.88595607068692E-16));
#33623=CARTESIAN_POINT('Origin',(0.,0.5,0.));
#33624=CARTESIAN_POINT('',(-1.129765,0.5,-1.38356309103871E-16));
#33625=CARTESIAN_POINT('Origin',(0.,0.5,0.));
#33626=CARTESIAN_POINT('Origin',(0.,0.47,0.));
#33627=CARTESIAN_POINT('',(-1.6,0.44,-1.95943487863577E-16));
#33628=CARTESIAN_POINT('Origin',(0.,0.44,0.));
#33629=CARTESIAN_POINT('',(-1.57,0.47,-1.92269547466134E-16));
#33630=CARTESIAN_POINT('Origin',(0.,0.,0.));
#33631=CARTESIAN_POINT('',(-1.6,-0.44,-1.95943487863577E-16));
#33632=CARTESIAN_POINT('Origin',(0.,-0.44,0.));
#33633=CARTESIAN_POINT('',(-1.6,0.,-1.95943487863577E-16));
#33634=CARTESIAN_POINT('Origin',(0.,-0.47,0.));
#33635=CARTESIAN_POINT('',(-1.54,-0.5,-1.88595607068692E-16));
#33636=CARTESIAN_POINT('Origin',(0.,-0.5,0.));
#33637=CARTESIAN_POINT('',(-1.57,-0.47,-1.92269547466134E-16));
#33638=CARTESIAN_POINT('Origin',(1.129765,-0.5,0.));
#33639=CARTESIAN_POINT('Origin',(0.,0.,0.));
#33640=CARTESIAN_POINT('',(-1.129765,0.,-1.38356309103871E-16));
#33641=CARTESIAN_POINT('',(0.,0.,0.));
#33642=CARTESIAN_POINT('Origin',(1.1,0.,0.));
#33643=CARTESIAN_POINT('',(1.1,-2.23201749654651E-33,0.29765));
#33644=CARTESIAN_POINT('',(1.1,-2.23201749654651E-33,-0.29765));
#33645=CARTESIAN_POINT('Origin',(1.1,0.,0.));
#33646=CARTESIAN_POINT('Origin',(0.685838782044607,0.,-0.860014630714833));
#33647=CARTESIAN_POINT('',(0.918550922801216,-5.31350540756609E-33,-0.674432891191581));
#33648=CARTESIAN_POINT('',(0.453126641287998,8.49470414473068E-34,-1.04559637023808));
#33649=CARTESIAN_POINT('Origin',(0.685838782044607,0.,-0.860014630714833));
#33650=CARTESIAN_POINT('Origin',(-0.244773027351946,0.,-1.07242070340001));
#33651=CARTESIAN_POINT('',(0.0454142657089739,-2.23201749654651E-33,-1.1386540593921));
#33652=CARTESIAN_POINT('',(-0.534960320412865,-2.23201749654651E-33,-1.00618734740791));
#33653=CARTESIAN_POINT('Origin',(-0.244773027351946,0.,-1.07242070340001));
#33654=CARTESIAN_POINT('Origin',(-0.991065754692661,0.,-0.477272113029314));
#33655=CARTESIAN_POINT('',(-0.86192025974432,8.49470414473067E-34,-0.745445496560469));
#33656=CARTESIAN_POINT('',(-1.120211249641,-5.31350540756609E-33,-0.209098729498159));
#33657=CARTESIAN_POINT('Origin',(-0.991065754692661,0.,-0.477272113029314));
#33658=CARTESIAN_POINT('Origin',(-0.991065754692661,0.,0.477272113029314));
#33659=CARTESIAN_POINT('',(-1.120211249641,-2.23201749654651E-33,0.209098729498159));
#33660=CARTESIAN_POINT('',(-0.86192025974432,-2.23201749654651E-33,0.745445496560469));
#33661=CARTESIAN_POINT('Origin',(-0.991065754692661,0.,0.477272113029314));
#33662=CARTESIAN_POINT('Origin',(-0.244773027351946,0.,1.07242070340001));
#33663=CARTESIAN_POINT('',(-0.534960320412866,-2.23201749654651E-33,1.00618734740791));
#33664=CARTESIAN_POINT('',(0.0454142657089737,-2.23201749654651E-33,1.1386540593921));
#33665=CARTESIAN_POINT('Origin',(-0.244773027351946,0.,1.07242070340001));
#33666=CARTESIAN_POINT('Origin',(0.685838782044607,0.,0.860014630714833));
#33667=CARTESIAN_POINT('',(0.453126641287998,-2.23201749654651E-33,1.04559637023808));
#33668=CARTESIAN_POINT('',(0.918550922801216,-2.23201749654651E-33,0.674432891191581));
#33669=CARTESIAN_POINT('Origin',(0.685838782044607,0.,0.860014630714833));
#33670=CARTESIAN_POINT('',(0.,0.,0.));
#33671=CARTESIAN_POINT('Origin',(0.685838782044607,0.,0.860014630714833));
#33672=CARTESIAN_POINT('',(0.413083465285518,-0.05953,0.993751811093549));
#33673=CARTESIAN_POINT('',(0.876916659919095,-0.05953,0.623857181492959));
#33674=CARTESIAN_POINT('Ctrl Pts',(0.413083465285518,-0.05953,0.993751811093549));
#33675=CARTESIAN_POINT('Ctrl Pts',(0.419070565453383,-0.0925528133349865,
0.991263089003441));
#33676=CARTESIAN_POINT('Ctrl Pts',(0.430199341854858,-0.124911173756694,
0.986608710139579));
#33677=CARTESIAN_POINT('Ctrl Pts',(0.457978755888596,-0.177924977804098,
0.973971221090534));
#33678=CARTESIAN_POINT('Ctrl Pts',(0.473077587363685,-0.199697230012983,
0.966820759530997));
#33679=CARTESIAN_POINT('Ctrl Pts',(0.507057380724533,-0.237895043532788,
0.949440676105255));
#33680=CARTESIAN_POINT('Ctrl Pts',(0.525933334162555,-0.254319232363049,
0.939198248544428));
#33681=CARTESIAN_POINT('Ctrl Pts',(0.564362943424238,-0.28018331644634,
0.916597376014514));
#33682=CARTESIAN_POINT('Ctrl Pts',(0.585840553788742,-0.29104845371857,
0.903141581680914));
#33683=CARTESIAN_POINT('Ctrl Pts',(0.629305439856167,-0.30527573347708,
0.873412008702649));
#33684=CARTESIAN_POINT('Ctrl Pts',(0.651278921914856,-0.308638795020976,
0.857118508332695));
#33685=CARTESIAN_POINT('Ctrl Pts',(0.690705563850638,-0.308638795020976,
0.825676810575914));
#33686=CARTESIAN_POINT('Ctrl Pts',(0.711480111898423,-0.30527573347708,
0.807879894508811));
#33687=CARTESIAN_POINT('Ctrl Pts',(0.750136149454208,-0.29104845371857,
0.772120216227122));
#33688=CARTESIAN_POINT('Ctrl Pts',(0.768033796848072,-0.28018331644634,
0.754175290318038));
#33689=CARTESIAN_POINT('Ctrl Pts',(0.798619410861634,-0.254319232363049,
0.721738358858166));
#33690=CARTESIAN_POINT('Ctrl Pts',(0.812805334167529,-0.237895043532788,
0.705614819529209));
#33691=CARTESIAN_POINT('Ctrl Pts',(0.837310877969633,-0.199697230012983,
0.676354402927683));
#33692=CARTESIAN_POINT('Ctrl Pts',(0.847641868610495,-0.177924977804098,
0.663225258065736));
#33693=CARTESIAN_POINT('Ctrl Pts',(0.866144010579847,-0.124911173756694,
0.638954437806245));
#33694=CARTESIAN_POINT('Ctrl Pts',(0.873158080166742,-0.0925528133349865,
0.62914037979579));
#33695=CARTESIAN_POINT('Ctrl Pts',(0.876916659919095,-0.05953,0.623857181492959));
#33696=CARTESIAN_POINT('',(0.437601487681057,-0.05953,1.03511272300331));
#33697=CARTESIAN_POINT('Origin',(0.685838782044607,-0.05953,0.860014630714833));
#33698=CARTESIAN_POINT('',(0.911784794170997,-0.05953,0.656964154625313));
#33699=CARTESIAN_POINT('Ctrl Pts',(0.911784794170998,-0.0595300000000001,
0.656964154625312));
#33700=CARTESIAN_POINT('Ctrl Pts',(0.909827729890942,-0.0762225747374255,
0.659680317203144));
#33701=CARTESIAN_POINT('Ctrl Pts',(0.907004864562642,-0.0928409665394228,
0.663576540841106));
#33702=CARTESIAN_POINT('Ctrl Pts',(0.895234408667242,-0.144299303100741,
0.679480524217551));
#33703=CARTESIAN_POINT('Ctrl Pts',(0.882797231409153,-0.177024326825049,
0.695831250979106));
#33704=CARTESIAN_POINT('Ctrl Pts',(0.854332839576145,-0.227269801620064,
0.73042219438957));
#33705=CARTESIAN_POINT('Ctrl Pts',(0.834863020612702,-0.251265615809407,
0.752807465209441));
#33706=CARTESIAN_POINT('Ctrl Pts',(0.800439809856111,-0.279889827963178,
0.789147407129766));
#33707=CARTESIAN_POINT('Ctrl Pts',(0.781998747691871,-0.290879136862659,
0.80756613568454));
#33708=CARTESIAN_POINT('Ctrl Pts',(0.742239891936898,-0.305251990234487,
0.844254137480382));
#33709=CARTESIAN_POINT('Ctrl Pts',(0.720906778729541,-0.308638795020976,
0.862505527716294));
#33710=CARTESIAN_POINT('Ctrl Pts',(0.680463863683392,-0.308638795020976,
0.894757676234429));
#33711=CARTESIAN_POINT('Ctrl Pts',(0.657923009631182,-0.305251990234488,
0.91149460735272));
#33712=CARTESIAN_POINT('Ctrl Pts',(0.613307674922609,-0.290879136862659,
0.942092777160053));
#33713=CARTESIAN_POINT('Ctrl Pts',(0.591247219971725,-0.279889827963178,
0.955972930713954));
#33714=CARTESIAN_POINT('Ctrl Pts',(0.548158511259202,-0.251265615809407,
0.981446681891443));
#33715=CARTESIAN_POINT('Ctrl Pts',(0.522002043615455,-0.227269801620063,
0.995447160474328));
#33716=CARTESIAN_POINT('Ctrl Pts',(0.481944444320713,-0.177024326825049,
1.01550068154148));
#33717=CARTESIAN_POINT('Ctrl Pts',(0.463236132117164,-0.14429930310074,
1.0239876538093));
#33718=CARTESIAN_POINT('Ctrl Pts',(0.445111721969657,-0.0928409665394226,
1.03192403056628));
#33719=CARTESIAN_POINT('Ctrl Pts',(0.440685038163619,-0.0762225747374254,
1.03380912944435));
#33720=CARTESIAN_POINT('Ctrl Pts',(0.437601487681056,-0.05953,1.03511272300331));
#33721=CARTESIAN_POINT('Origin',(0.685838782044607,-0.05953,0.860014630714833));
#33722=CARTESIAN_POINT('Origin',(0.,-0.208355,0.));
#33723=CARTESIAN_POINT('',(0.0548532617164168,-0.05953,1.12247250791415));
#33724=CARTESIAN_POINT('Origin',(0.,-0.05953,0.));
#33725=CARTESIAN_POINT('',(-0.536443649899848,-0.05953,0.987512846410683));
#33726=CARTESIAN_POINT('Ctrl Pts',(0.0548532617164173,-0.0595300000000001,
1.12247250791414));
#33727=CARTESIAN_POINT('Ctrl Pts',(0.05150947068137,-0.0762225747374254,
1.12263591311425));
#33728=CARTESIAN_POINT('Ctrl Pts',(0.0467032526342597,-0.0928409665394227,
1.12285816383385));
#33729=CARTESIAN_POINT('Ctrl Pts',(0.0269302585198975,-0.144299303100741,
1.12357162229597));
#33730=CARTESIAN_POINT('Ctrl Pts',(0.006392292392153,-0.177024326825049,
1.12404235695137));
#33731=CARTESIAN_POINT('Ctrl Pts',(-0.0383992541984087,-0.227269801620063,
1.12335509974011));
#33732=CARTESIAN_POINT('Ctrl Pts',(-0.0680399972366993,-0.251265615809407,
1.12208997038458));
#33733=CARTESIAN_POINT('Ctrl Pts',(-0.117914228755037,-0.279889827963178,
1.1178344036749));
#33734=CARTESIAN_POINT('Ctrl Pts',(-0.14381238480104,-0.290879136862659,
1.11490049012186));
#33735=CARTESIAN_POINT('Ctrl Pts',(-0.19728546073067,-0.305251990234488,
1.10669035995599));
#33736=CARTESIAN_POINT('Ctrl Pts',(-0.224855950742601,-0.308638795020976,
1.10139101611326));
#33737=CARTESIAN_POINT('Ctrl Pts',(-0.275287440920027,-0.308638795020976,
1.0898803575765));
#33738=CARTESIAN_POINT('Ctrl Pts',(-0.302426893214945,-0.305251990234488,
1.08269251410343));
#33739=CARTESIAN_POINT('Ctrl Pts',(-0.35416671187353,-0.290879136862659,
1.06688848765783));
#33740=CARTESIAN_POINT('Ctrl Pts',(-0.3787731215897,-0.279889827963178,
1.05829506364875));
#33741=CARTESIAN_POINT('Ctrl Pts',(-0.425554672694338,-0.251265615809407,
1.04048957871266));
#33742=CARTESIAN_POINT('Ctrl Pts',(-0.452808978448581,-0.227269801620063,
1.02876878445619));
#33743=CARTESIAN_POINT('Ctrl Pts',(-0.493462957200432,-0.177024326825049,
1.0099536580922));
#33744=CARTESIAN_POINT('Ctrl Pts',(-0.511762781179148,-0.14429930310074,
1.00061845128527));
#33745=CARTESIAN_POINT('Ctrl Pts',(-0.529268075276157,-0.0928409665394226,
0.991396466802468));
#33746=CARTESIAN_POINT('Ctrl Pts',(-0.533501897135713,-0.0762225747374254,
0.989110885965947));
#33747=CARTESIAN_POINT('Ctrl Pts',(-0.536443649899848,-0.0595300000000001,
0.987512846410683));
#33748=CARTESIAN_POINT('',(-0.843383895613249,-0.05953,0.742736168477219));
#33749=CARTESIAN_POINT('Origin',(0.,-0.05953,0.));
#33750=CARTESIAN_POINT('',(-1.10653577764992,-0.05953,0.196295654879792));
#33751=CARTESIAN_POINT('Ctrl Pts',(-0.843383895613249,-0.0595300000000001,
0.742736168477219));
#33752=CARTESIAN_POINT('Ctrl Pts',(-0.84559647055299,-0.0762225747374255,
0.740223768851062));
#33753=CARTESIAN_POINT('Ctrl Pts',(-0.848766861100456,-0.0928409665394227,
0.736604687327351));
#33754=CARTESIAN_POINT('Ctrl Pts',(-0.861652925570091,-0.144299303100741,
0.721590372101268));
#33755=CARTESIAN_POINT('Ctrl Pts',(-0.87482617317514,-0.177024326825049,
0.705826641853758));
#33756=CARTESIAN_POINT('Ctrl Pts',(-0.902215926359523,-0.227269801620063,
0.670378702718353));
#33757=CARTESIAN_POINT('Ctrl Pts',(-0.919707509403859,-0.251265615809407,
0.646415841396062));
#33758=CARTESIAN_POINT('Ctrl Pts',(-0.947476448101718,-0.279889827963178,
0.604769294586516));
#33759=CARTESIAN_POINT('Ctrl Pts',(-0.961329858300736,-0.290879136862659,
0.582692035672022));
#33760=CARTESIAN_POINT('Ctrl Pts',(-0.988250837578047,-0.305251990234488,
0.535766169015486));
#33761=CARTESIAN_POINT('Ctrl Pts',(-1.00129756308006,-0.308638795020976,
0.510906605094603));
#33762=CARTESIAN_POINT('Ctrl Pts',(-1.02374168767024,-0.308638795020976,
0.46430090015576));
#33763=CARTESIAN_POINT('Ctrl Pts',(-1.03504317708586,-0.305251990234488,
0.438600874831839));
#33764=CARTESIAN_POINT('Ctrl Pts',(-1.05494634094458,-0.290879136862659,
0.388295406390235));
#33765=CARTESIAN_POINT('Ctrl Pts',(-1.06356957703048,-0.279889827963178,
0.363699428370917));
#33766=CARTESIAN_POINT('Ctrl Pts',(-1.0788165083757,-0.251265615809407,
0.316022600643821));
#33767=CARTESIAN_POINT('Ctrl Pts',(-1.08664560412098,-0.227269801620063,
0.287406530683752));
#33768=CARTESIAN_POINT('Ctrl Pts',(-1.09728268713976,-0.177024326825049,
0.243890930799337));
#33769=CARTESIAN_POINT('Ctrl Pts',(-1.10139388218929,-0.144299303100741,
0.22376314604679));
#33770=CARTESIAN_POINT('Ctrl Pts',(-1.10509821673782,-0.0928409665394227,
0.204327142733961));
#33771=CARTESIAN_POINT('Ctrl Pts',(-1.10595102243643,-0.0762225747374254,
0.199591971170104));
#33772=CARTESIAN_POINT('Ctrl Pts',(-1.10653577764992,-0.0595300000000001,
0.196295654879792));
#33773=CARTESIAN_POINT('',(-1.123812,-0.05953,1.37627276864339E-16));
#33774=CARTESIAN_POINT('Origin',(0.,-0.05953,0.));
#33775=CARTESIAN_POINT('',(-1.123812,-0.35718,1.37627276864339E-16));
#33776=CARTESIAN_POINT('',(-1.123812,-0.208355,1.37627276864339E-16));
#33777=CARTESIAN_POINT('Origin',(0.,-0.35718,0.));
#33778=CARTESIAN_POINT('',(-1.10653577764992,-0.05953,-0.196295654879793));
#33779=CARTESIAN_POINT('Origin',(0.,-0.05953,0.));
#33780=CARTESIAN_POINT('',(-0.843383895613249,-0.05953,-0.742736168477219));
#33781=CARTESIAN_POINT('Ctrl Pts',(-1.10653577764992,-0.0595300000000001,
-0.196295654879792));
#33782=CARTESIAN_POINT('Ctrl Pts',(-1.10595102243643,-0.0762225747374255,
-0.199591971170104));
#33783=CARTESIAN_POINT('Ctrl Pts',(-1.10509821673782,-0.0928409665394228,
-0.204327142733962));
#33784=CARTESIAN_POINT('Ctrl Pts',(-1.10139388218929,-0.144299303100741,
-0.22376314604679));
#33785=CARTESIAN_POINT('Ctrl Pts',(-1.09728268713976,-0.177024326825049,
-0.243890930799338));
#33786=CARTESIAN_POINT('Ctrl Pts',(-1.08664560412098,-0.227269801620063,
-0.287406530683753));
#33787=CARTESIAN_POINT('Ctrl Pts',(-1.0788165083757,-0.251265615809407,
-0.316022600643821));
#33788=CARTESIAN_POINT('Ctrl Pts',(-1.06356957703048,-0.279889827963178,
-0.363699428370918));
#33789=CARTESIAN_POINT('Ctrl Pts',(-1.05494634094458,-0.290879136862659,
-0.388295406390235));
#33790=CARTESIAN_POINT('Ctrl Pts',(-1.03504317708586,-0.305251990234488,
-0.438600874831839));
#33791=CARTESIAN_POINT('Ctrl Pts',(-1.02374168767024,-0.308638795020976,
-0.46430090015576));
#33792=CARTESIAN_POINT('Ctrl Pts',(-1.00129756308006,-0.308638795020976,
-0.510906605094603));
#33793=CARTESIAN_POINT('Ctrl Pts',(-0.988250837578047,-0.305251990234488,
-0.535766169015486));
#33794=CARTESIAN_POINT('Ctrl Pts',(-0.961329858300736,-0.290879136862659,
-0.582692035672022));
#33795=CARTESIAN_POINT('Ctrl Pts',(-0.947476448101718,-0.279889827963178,
-0.604769294586516));
#33796=CARTESIAN_POINT('Ctrl Pts',(-0.919707509403859,-0.251265615809407,
-0.646415841396062));
#33797=CARTESIAN_POINT('Ctrl Pts',(-0.902215926359523,-0.227269801620064,
-0.670378702718353));
#33798=CARTESIAN_POINT('Ctrl Pts',(-0.87482617317514,-0.177024326825049,
-0.705826641853758));
#33799=CARTESIAN_POINT('Ctrl Pts',(-0.861652925570091,-0.144299303100741,
-0.721590372101268));
#33800=CARTESIAN_POINT('Ctrl Pts',(-0.848766861100456,-0.0928409665394229,
-0.736604687327351));
#33801=CARTESIAN_POINT('Ctrl Pts',(-0.84559647055299,-0.0762225747374255,
-0.740223768851063));
#33802=CARTESIAN_POINT('Ctrl Pts',(-0.843383895613249,-0.0595300000000001,
-0.742736168477219));
#33803=CARTESIAN_POINT('',(-0.536443649899847,-0.05953,-0.987512846410683));
#33804=CARTESIAN_POINT('Origin',(0.,-0.05953,0.));
#33805=CARTESIAN_POINT('',(0.0548532617164172,-0.05953,-1.12247250791415));
#33806=CARTESIAN_POINT('Ctrl Pts',(-0.536443649899848,-0.0595300000000001,
-0.987512846410683));
#33807=CARTESIAN_POINT('Ctrl Pts',(-0.533501897135712,-0.0762225747374254,
-0.989110885965947));
#33808=CARTESIAN_POINT('Ctrl Pts',(-0.529268075276156,-0.0928409665394227,
-0.991396466802469));
#33809=CARTESIAN_POINT('Ctrl Pts',(-0.511762781179147,-0.144299303100741,
-1.00061845128527));
#33810=CARTESIAN_POINT('Ctrl Pts',(-0.493462957200432,-0.177024326825049,
-1.0099536580922));
#33811=CARTESIAN_POINT('Ctrl Pts',(-0.45280897844858,-0.227269801620063,
-1.02876878445619));
#33812=CARTESIAN_POINT('Ctrl Pts',(-0.425554672694337,-0.251265615809407,
-1.04048957871266));
#33813=CARTESIAN_POINT('Ctrl Pts',(-0.3787731215897,-0.279889827963178,
-1.05829506364875));
#33814=CARTESIAN_POINT('Ctrl Pts',(-0.354166711873529,-0.290879136862659,
-1.06688848765783));
#33815=CARTESIAN_POINT('Ctrl Pts',(-0.302426893214944,-0.305251990234488,
-1.08269251410343));
#33816=CARTESIAN_POINT('Ctrl Pts',(-0.275287440920027,-0.308638795020976,
-1.0898803575765));
#33817=CARTESIAN_POINT('Ctrl Pts',(-0.224855950742601,-0.308638795020976,
-1.10139101611326));
#33818=CARTESIAN_POINT('Ctrl Pts',(-0.19728546073067,-0.305251990234488,
-1.10669035995599));
#33819=CARTESIAN_POINT('Ctrl Pts',(-0.143812384801039,-0.290879136862659,
-1.11490049012186));
#33820=CARTESIAN_POINT('Ctrl Pts',(-0.117914228755037,-0.279889827963178,
-1.1178344036749));
#33821=CARTESIAN_POINT('Ctrl Pts',(-0.0680399972366989,-0.251265615809407,
-1.12208997038458));
#33822=CARTESIAN_POINT('Ctrl Pts',(-0.0383992541984084,-0.227269801620063,
-1.12335509974011));
#33823=CARTESIAN_POINT('Ctrl Pts',(0.00639229239215326,-0.177024326825049,
-1.12404235695137));
#33824=CARTESIAN_POINT('Ctrl Pts',(0.0269302585198977,-0.144299303100741,
-1.12357162229597));
#33825=CARTESIAN_POINT('Ctrl Pts',(0.04670325263426,-0.0928409665394228,
-1.12285816383385));
#33826=CARTESIAN_POINT('Ctrl Pts',(0.0515094706813703,-0.0762225747374255,
-1.12263591311425));
#33827=CARTESIAN_POINT('Ctrl Pts',(0.0548532617164176,-0.0595300000000001,
-1.12247250791414));
#33828=CARTESIAN_POINT('',(0.437601487681057,-0.05953,-1.03511272300331));
#33829=CARTESIAN_POINT('Origin',(0.,-0.05953,0.));
#33830=CARTESIAN_POINT('',(0.911784794170997,-0.05953,-0.656964154625313));
#33831=CARTESIAN_POINT('Ctrl Pts',(0.437601487681056,-0.0595300000000001,
-1.03511272300331));
#33832=CARTESIAN_POINT('Ctrl Pts',(0.440685038163619,-0.0762225747374255,
-1.03380912944435));
#33833=CARTESIAN_POINT('Ctrl Pts',(0.445111721969657,-0.0928409665394228,
-1.03192403056628));
#33834=CARTESIAN_POINT('Ctrl Pts',(0.463236132117164,-0.144299303100741,
-1.0239876538093));
#33835=CARTESIAN_POINT('Ctrl Pts',(0.481944444320713,-0.177024326825049,
-1.01550068154148));
#33836=CARTESIAN_POINT('Ctrl Pts',(0.522002043615455,-0.227269801620064,
-0.995447160474328));
#33837=CARTESIAN_POINT('Ctrl Pts',(0.548158511259203,-0.251265615809407,
-0.981446681891443));
#33838=CARTESIAN_POINT('Ctrl Pts',(0.591247219971725,-0.279889827963178,
-0.955972930713954));
#33839=CARTESIAN_POINT('Ctrl Pts',(0.613307674922609,-0.290879136862659,
-0.942092777160053));
#33840=CARTESIAN_POINT('Ctrl Pts',(0.657923009631182,-0.305251990234487,
-0.91149460735272));
#33841=CARTESIAN_POINT('Ctrl Pts',(0.680463863683393,-0.308638795020976,
-0.894757676234429));
#33842=CARTESIAN_POINT('Ctrl Pts',(0.720906778729542,-0.308638795020976,
-0.862505527716294));
#33843=CARTESIAN_POINT('Ctrl Pts',(0.742239891936899,-0.305251990234488,
-0.844254137480381));
#33844=CARTESIAN_POINT('Ctrl Pts',(0.781998747691872,-0.290879136862659,
-0.80756613568454));
#33845=CARTESIAN_POINT('Ctrl Pts',(0.800439809856112,-0.279889827963178,
-0.789147407129765));
#33846=CARTESIAN_POINT('Ctrl Pts',(0.834863020612702,-0.251265615809407,
-0.752807465209441));
#33847=CARTESIAN_POINT('Ctrl Pts',(0.854332839576145,-0.227269801620064,
-0.73042219438957));
#33848=CARTESIAN_POINT('Ctrl Pts',(0.882797231409153,-0.177024326825049,
-0.695831250979106));
#33849=CARTESIAN_POINT('Ctrl Pts',(0.895234408667242,-0.144299303100741,
-0.679480524217551));
#33850=CARTESIAN_POINT('Ctrl Pts',(0.907004864562642,-0.0928409665394228,
-0.663576540841106));
#33851=CARTESIAN_POINT('Ctrl Pts',(0.909827729890942,-0.0762225747374256,
-0.659680317203144));
#33852=CARTESIAN_POINT('Ctrl Pts',(0.911784794170998,-0.0595300000000001,
-0.656964154625312));
#33853=CARTESIAN_POINT('',(1.08212377959455,-0.05953,-0.303251606722892));
#33854=CARTESIAN_POINT('Origin',(0.,-0.05953,0.));
#33855=CARTESIAN_POINT('',(1.08212377959455,-0.05953,0.303251606722892));
#33856=CARTESIAN_POINT('Ctrl Pts',(1.08212377959455,-0.0595300000000001,
-0.303251606722892));
#33857=CARTESIAN_POINT('Ctrl Pts',(1.0830271513892,-0.0762225747374255,
-0.300028012588062));
#33858=CARTESIAN_POINT('Ctrl Pts',(1.08431331394788,-0.0928409665394228,
-0.2953917518996));
#33859=CARTESIAN_POINT('Ctrl Pts',(1.08940878963422,-0.144299303100741,
-0.276273267473431));
#33860=CARTESIAN_POINT('Ctrl Pts',(1.09443784939331,-0.177024326825049,
-0.256354979351213));
#33861=CARTESIAN_POINT('Ctrl Pts',(1.10373487993589,-0.227269801620064,
-0.212533521233765));
#33862=CARTESIAN_POINT('Ctrl Pts',(1.10909715583869,-0.251265615809407,
-0.183354415742157));
#33863=CARTESIAN_POINT('Ctrl Pts',(1.1160463456491,-0.279889827963178,-0.133783682657561));
#33864=CARTESIAN_POINT('Ctrl Pts',(1.11894887330541,-0.290879136862659,
-0.107881990270302));
#33865=CARTESIAN_POINT('Ctrl Pts',(1.12284346704144,-0.305251990234488,
-0.0539226701638766));
#33866=CARTESIAN_POINT('Ctrl Pts',(1.123812,-0.308638795020976,-0.025864214957475));
#33867=CARTESIAN_POINT('Ctrl Pts',(1.123812,-0.308638795020976,0.025864214957475));
#33868=CARTESIAN_POINT('Ctrl Pts',(1.12284346704144,-0.305251990234488,
0.0539226701638766));
#33869=CARTESIAN_POINT('Ctrl Pts',(1.11894887330541,-0.290879136862659,
0.107881990270302));
#33870=CARTESIAN_POINT('Ctrl Pts',(1.1160463456491,-0.279889827963178,0.133783682657561));
#33871=CARTESIAN_POINT('Ctrl Pts',(1.10909715583869,-0.251265615809407,
0.183354415742157));
#33872=CARTESIAN_POINT('Ctrl Pts',(1.10373487993589,-0.227269801620064,
0.212533521233765));
#33873=CARTESIAN_POINT('Ctrl Pts',(1.09443784939331,-0.177024326825049,
0.256354979351213));
#33874=CARTESIAN_POINT('Ctrl Pts',(1.08940878963422,-0.144299303100741,
0.276273267473431));
#33875=CARTESIAN_POINT('Ctrl Pts',(1.08431331394788,-0.0928409665394228,
0.2953917518996));
#33876=CARTESIAN_POINT('Ctrl Pts',(1.0830271513892,-0.0762225747374255,
0.300028012588062));
#33877=CARTESIAN_POINT('Ctrl Pts',(1.08212377959455,-0.0595300000000001,
0.303251606722892));
#33878=CARTESIAN_POINT('Origin',(0.,-0.05953,0.));
#33879=CARTESIAN_POINT('Origin',(0.,-0.05953,0.));
#33880=CARTESIAN_POINT('',(0.0589974094846122,-0.05953,1.07456964270265));
#33881=CARTESIAN_POINT('Origin',(0.,-0.05953,0.));
#33882=CARTESIAN_POINT('Origin',(-0.244773027351946,-0.05953,1.07242070340001));
#33883=CARTESIAN_POINT('Origin',(-0.244773027351946,0.,1.07242070340001));
#33884=CARTESIAN_POINT('',(-0.519393123750572,-0.05953,0.942555777842682));
#33885=CARTESIAN_POINT('Ctrl Pts',(-0.519393123750572,-0.05953,0.942555777842682));
#33886=CARTESIAN_POINT('Ctrl Pts',(-0.513714466572041,-0.0925528133349865,
0.945684988399766));
#33887=CARTESIAN_POINT('Ctrl Pts',(-0.503136848051455,-0.124911173756694,
0.951483858396181));
#33888=CARTESIAN_POINT('Ctrl Pts',(-0.47593627990192,-0.177924977804098,
0.965323333309091));
#33889=CARTESIAN_POINT('Ctrl Pts',(-0.460931856495794,-0.199697230012983,
0.972669835243841));
#33890=CARTESIAN_POINT('Ctrl Pts',(-0.426157505475872,-0.237895043532788,
0.988400002689705));
#33891=CARTESIAN_POINT('Ctrl Pts',(-0.406380688682952,-0.254319232363049,
0.996771768218699));
#33892=CARTESIAN_POINT('Ctrl Pts',(-0.364750145543744,-0.28018331644634,
1.01272583306292));
#33893=CARTESIAN_POINT('Ctrl Pts',(-0.340838910881557,-0.29104845371857,
1.02112815447116));
#33894=CARTESIAN_POINT('Ctrl Pts',(-0.290495481564827,-0.30527573347708,
1.036574285215));
#33895=CARTESIAN_POINT('Ctrl Pts',(-0.264056468041074,-0.308638795020976,
1.04359501395068));
#33896=CARTESIAN_POINT('Ctrl Pts',(-0.214892249704082,-0.308638795020976,
1.05481642595959));
#33897=CARTESIAN_POINT('Ctrl Pts',(-0.188025341585962,-0.30527573347708,
1.05996242598502));
#33898=CARTESIAN_POINT('Ctrl Pts',(-0.135965654106109,-0.29104845371857,
1.06788913840721));
#33899=CARTESIAN_POINT('Ctrl Pts',(-0.110776745452494,-0.28018331644634,
1.07069360430242));
#33900=CARTESIAN_POINT('Ctrl Pts',(-0.0663467128214646,-0.254319232363049,
1.07438230428002));
#33901=CARTESIAN_POINT('Ctrl Pts',(-0.0448960436540983,-0.237895043532788,
1.07542044338697));
#33902=CARTESIAN_POINT('Ctrl Pts',(-0.00674037211528124,-0.199697230012983,
1.07633607767727));
#33903=CARTESIAN_POINT('Ctrl Pts',(0.00996567398334777,-0.177924977804098,
1.07622728347683));
#33904=CARTESIAN_POINT('Ctrl Pts',(0.0404772621979741,-0.124911173756694,
1.07556023164702));
#33905=CARTESIAN_POINT('Ctrl Pts',(0.0525234025782719,-0.0925528133349865,
1.07492508698591));
#33906=CARTESIAN_POINT('Ctrl Pts',(0.0589974094846124,-0.05953,1.07456964270265));
#33907=CARTESIAN_POINT('Origin',(-0.244773027351946,-0.05953,1.07242070340001));
#33908=CARTESIAN_POINT('Origin',(0.,-0.05953,0.));
#33909=CARTESIAN_POINT('',(-0.803348093619616,-0.05953,0.716109245731214));
#33910=CARTESIAN_POINT('Origin',(0.,-0.05953,0.));
#33911=CARTESIAN_POINT('Origin',(-0.991065754692661,-0.05953,0.477272113029314));
#33912=CARTESIAN_POINT('Origin',(-0.991065754692661,0.,0.477272113029314));
#33913=CARTESIAN_POINT('',(-1.06075609691358,-0.05953,0.181596019242328));
#33914=CARTESIAN_POINT('Ctrl Pts',(-1.06075609691358,-0.05953,0.181596019242328));
#33915=CARTESIAN_POINT('Ctrl Pts',(-1.05966202740332,-0.0925528133349865,
0.187986803072856));
#33916=CARTESIAN_POINT('Ctrl Pts',(-1.05760072925372,-0.124911173756694,
0.199872254546857));
#33917=CARTESIAN_POINT('Ctrl Pts',(-1.05146158959546,-0.177924977804098,
0.22976728653846));
#33918=CARTESIAN_POINT('Ctrl Pts',(-1.04785021111757,-0.199697230012983,
0.246078686169301));
#33919=CARTESIAN_POINT('Ctrl Pts',(-1.03846709802406,-0.237895043532788,
0.283073967563097));
#33920=CARTESIAN_POINT('Ctrl Pts',(-1.03268176429485,-0.254319232363049,
0.303755815985685));
#33921=CARTESIAN_POINT('Ctrl Pts',(-1.01919893537026,-0.28018331644634,
0.346251081972725));
#33922=CARTESIAN_POINT('Ctrl Pts',(-1.01085972381132,-0.29104845371857,
0.370184399726282));
#33923=CARTESIAN_POINT('Ctrl Pts',(-0.99154738033959,-0.30527573347708,
0.419174982698463));
#33924=CARTESIAN_POINT('Ctrl Pts',(-0.980551951791748,-0.308638795020976,
0.444223188605045));
#33925=CARTESIAN_POINT('Ctrl Pts',(-0.958671816228589,-0.308638795020976,
0.489657758261848));
#33926=CARTESIAN_POINT('Ctrl Pts',(-0.945943877838127,-0.30527573347708,
0.51387163140139));
#33927=CARTESIAN_POINT('Ctrl Pts',(-0.91968254693063,-0.29104845371857,
0.559515758398093));
#33928=CARTESIAN_POINT('Ctrl Pts',(-0.906170138993533,-0.28018331644634,
0.580957796077825));
#33929=CARTESIAN_POINT('Ctrl Pts',(-0.8813524085237,-0.254319232363049,
0.617994461173994));
#33930=CARTESIAN_POINT('Ctrl Pts',(-0.868789784891799,-0.237895043532788,
0.635412538795143));
#33931=CARTESIAN_POINT('Ctrl Pts',(-0.845715984518854,-0.199697230012983,
0.66581473268113));
#33932=CARTESIAN_POINT('Ctrl Pts',(-0.835214876415962,-0.177924977804098,
0.678808213394124));
#33933=CARTESIAN_POINT('Ctrl Pts',(-0.815669690204649,-0.124911173756694,
0.702247233627224));
#33934=CARTESIAN_POINT('Ctrl Pts',(-0.807662468433796,-0.0925528133349865,
0.711269279199861));
#33935=CARTESIAN_POINT('Ctrl Pts',(-0.803348093619616,-0.05953,0.716109245731214));
#33936=CARTESIAN_POINT('Origin',(-0.991065754692661,-0.05953,0.477272113029314));
#33937=CARTESIAN_POINT('Origin',(0.,-0.05953,0.));
#33938=CARTESIAN_POINT('',(-1.076188,-0.05953,1.31795018948079E-16));
#33939=CARTESIAN_POINT('Origin',(0.,-0.05953,0.));
#33940=CARTESIAN_POINT('',(-1.06075609691358,-0.05953,-0.181596019242328));
#33941=CARTESIAN_POINT('Origin',(0.,-0.05953,0.));
#33942=CARTESIAN_POINT('Origin',(-0.991065754692661,-0.05953,-0.477272113029314));
#33943=CARTESIAN_POINT('Origin',(-0.991065754692661,0.,-0.477272113029314));
#33944=CARTESIAN_POINT('',(-0.803348093619616,-0.05953,-0.716109245731215));
#33945=CARTESIAN_POINT('Ctrl Pts',(-0.803348093619616,-0.05953,-0.716109245731215));
#33946=CARTESIAN_POINT('Ctrl Pts',(-0.807662468433795,-0.0925528133349865,
-0.711269279199862));
#33947=CARTESIAN_POINT('Ctrl Pts',(-0.815669690204649,-0.124911173756694,
-0.702247233627224));
#33948=CARTESIAN_POINT('Ctrl Pts',(-0.835214876415962,-0.177924977804098,
-0.678808213394124));
#33949=CARTESIAN_POINT('Ctrl Pts',(-0.845715984518854,-0.199697230012983,
-0.66581473268113));
#33950=CARTESIAN_POINT('Ctrl Pts',(-0.868789784891799,-0.237895043532788,
-0.635412538795143));
#33951=CARTESIAN_POINT('Ctrl Pts',(-0.8813524085237,-0.254319232363049,
-0.617994461173994));
#33952=CARTESIAN_POINT('Ctrl Pts',(-0.906170138993533,-0.28018331644634,
-0.580957796077826));
#33953=CARTESIAN_POINT('Ctrl Pts',(-0.91968254693063,-0.29104845371857,
-0.559515758398093));
#33954=CARTESIAN_POINT('Ctrl Pts',(-0.945943877838127,-0.30527573347708,
-0.51387163140139));
#33955=CARTESIAN_POINT('Ctrl Pts',(-0.958671816228589,-0.308638795020976,
-0.489657758261848));
#33956=CARTESIAN_POINT('Ctrl Pts',(-0.980551951791748,-0.308638795020976,
-0.444223188605045));
#33957=CARTESIAN_POINT('Ctrl Pts',(-0.99154738033959,-0.30527573347708,
-0.419174982698463));
#33958=CARTESIAN_POINT('Ctrl Pts',(-1.01085972381132,-0.29104845371857,
-0.370184399726282));
#33959=CARTESIAN_POINT('Ctrl Pts',(-1.01919893537026,-0.28018331644634,
-0.346251081972725));
#33960=CARTESIAN_POINT('Ctrl Pts',(-1.03268176429485,-0.254319232363049,
-0.303755815985685));
#33961=CARTESIAN_POINT('Ctrl Pts',(-1.03846709802406,-0.237895043532788,
-0.283073967563097));
#33962=CARTESIAN_POINT('Ctrl Pts',(-1.04785021111757,-0.199697230012983,
-0.246078686169302));
#33963=CARTESIAN_POINT('Ctrl Pts',(-1.05146158959546,-0.177924977804098,
-0.229767286538461));
#33964=CARTESIAN_POINT('Ctrl Pts',(-1.05760072925372,-0.124911173756694,
-0.199872254546858));
#33965=CARTESIAN_POINT('Ctrl Pts',(-1.05966202740332,-0.0925528133349864,
-0.187986803072857));
#33966=CARTESIAN_POINT('Ctrl Pts',(-1.06075609691358,-0.05953,-0.181596019242328));
#33967=CARTESIAN_POINT('Origin',(-0.991065754692661,-0.05953,-0.477272113029314));
#33968=CARTESIAN_POINT('Origin',(0.,-0.05953,0.));
#33969=CARTESIAN_POINT('',(-0.519393123750572,-0.05953,-0.942555777842682));
#33970=CARTESIAN_POINT('Origin',(0.,-0.05953,0.));
#33971=CARTESIAN_POINT('Origin',(-0.244773027351946,-0.05953,-1.07242070340001));
#33972=CARTESIAN_POINT('Origin',(-0.244773027351946,0.,-1.07242070340001));
#33973=CARTESIAN_POINT('',(0.0589974094846125,-0.05953,-1.07456964270265));
#33974=CARTESIAN_POINT('Ctrl Pts',(0.0589974094846127,-0.05953,-1.07456964270265));
#33975=CARTESIAN_POINT('Ctrl Pts',(0.0525234025782722,-0.0925528133349865,
-1.07492508698591));
#33976=CARTESIAN_POINT('Ctrl Pts',(0.0404772621979744,-0.124911173756694,
-1.07556023164702));
#33977=CARTESIAN_POINT('Ctrl Pts',(0.0099656739833481,-0.177924977804098,
-1.07622728347683));
#33978=CARTESIAN_POINT('Ctrl Pts',(-0.00674037211528096,-0.199697230012983,
-1.07633607767727));
#33979=CARTESIAN_POINT('Ctrl Pts',(-0.044896043654098,-0.237895043532788,
-1.07542044338697));
#33980=CARTESIAN_POINT('Ctrl Pts',(-0.0663467128214644,-0.254319232363049,
-1.07438230428002));
#33981=CARTESIAN_POINT('Ctrl Pts',(-0.110776745452493,-0.28018331644634,
-1.07069360430242));
#33982=CARTESIAN_POINT('Ctrl Pts',(-0.135965654106109,-0.29104845371857,
-1.06788913840721));
#33983=CARTESIAN_POINT('Ctrl Pts',(-0.188025341585962,-0.30527573347708,
-1.05996242598502));
#33984=CARTESIAN_POINT('Ctrl Pts',(-0.214892249704082,-0.308638795020976,
-1.05481642595959));
#33985=CARTESIAN_POINT('Ctrl Pts',(-0.264056468041074,-0.308638795020976,
-1.04359501395068));
#33986=CARTESIAN_POINT('Ctrl Pts',(-0.290495481564827,-0.30527573347708,
-1.036574285215));
#33987=CARTESIAN_POINT('Ctrl Pts',(-0.340838910881557,-0.291048453718569,
-1.02112815447116));
#33988=CARTESIAN_POINT('Ctrl Pts',(-0.364750145543744,-0.28018331644634,
-1.01272583306292));
#33989=CARTESIAN_POINT('Ctrl Pts',(-0.406380688682952,-0.254319232363049,
-0.996771768218699));
#33990=CARTESIAN_POINT('Ctrl Pts',(-0.426157505475872,-0.237895043532788,
-0.988400002689705));
#33991=CARTESIAN_POINT('Ctrl Pts',(-0.460931856495794,-0.199697230012983,
-0.972669835243841));
#33992=CARTESIAN_POINT('Ctrl Pts',(-0.475936279901919,-0.177924977804098,
-0.965323333309091));
#33993=CARTESIAN_POINT('Ctrl Pts',(-0.503136848051454,-0.124911173756694,
-0.951483858396181));
#33994=CARTESIAN_POINT('Ctrl Pts',(-0.513714466572041,-0.0925528133349865,
-0.945684988399766));
#33995=CARTESIAN_POINT('Ctrl Pts',(-0.519393123750572,-0.05953,-0.942555777842682));
#33996=CARTESIAN_POINT('Origin',(-0.244773027351946,-0.05953,-1.07242070340001));
#33997=CARTESIAN_POINT('Origin',(0.,-0.05953,0.));
#33998=CARTESIAN_POINT('',(0.413083465285518,-0.05953,-0.993751811093549));
#33999=CARTESIAN_POINT('Origin',(0.,-0.05953,0.));
#34000=CARTESIAN_POINT('Origin',(0.685838782044607,-0.05953,-0.860014630714833));
#34001=CARTESIAN_POINT('Origin',(0.685838782044607,0.,-0.860014630714833));
#34002=CARTESIAN_POINT('',(0.876916659919095,-0.05953,-0.623857181492959));
#34003=CARTESIAN_POINT('Ctrl Pts',(0.876916659919095,-0.05953,-0.623857181492958));
#34004=CARTESIAN_POINT('Ctrl Pts',(0.873158080166742,-0.0925528133349865,
-0.62914037979579));
#34005=CARTESIAN_POINT('Ctrl Pts',(0.866144010579847,-0.124911173756694,
-0.638954437806245));
#34006=CARTESIAN_POINT('Ctrl Pts',(0.847641868610495,-0.177924977804098,
-0.663225258065736));
#34007=CARTESIAN_POINT('Ctrl Pts',(0.837310877969633,-0.199697230012983,
-0.676354402927683));
#34008=CARTESIAN_POINT('Ctrl Pts',(0.81280533416753,-0.237895043532788,
-0.705614819529209));
#34009=CARTESIAN_POINT('Ctrl Pts',(0.798619410861634,-0.254319232363049,
-0.721738358858166));
#34010=CARTESIAN_POINT('Ctrl Pts',(0.768033796848072,-0.28018331644634,
-0.754175290318038));
#34011=CARTESIAN_POINT('Ctrl Pts',(0.750136149454208,-0.29104845371857,
-0.772120216227122));
#34012=CARTESIAN_POINT('Ctrl Pts',(0.711480111898423,-0.30527573347708,
-0.807879894508811));
#34013=CARTESIAN_POINT('Ctrl Pts',(0.690705563850638,-0.308638795020976,
-0.825676810575913));
#34014=CARTESIAN_POINT('Ctrl Pts',(0.651278921914856,-0.308638795020976,
-0.857118508332695));
#34015=CARTESIAN_POINT('Ctrl Pts',(0.629305439856167,-0.30527573347708,
-0.873412008702649));
#34016=CARTESIAN_POINT('Ctrl Pts',(0.585840553788742,-0.29104845371857,
-0.903141581680914));
#34017=CARTESIAN_POINT('Ctrl Pts',(0.564362943424239,-0.28018331644634,
-0.916597376014514));
#34018=CARTESIAN_POINT('Ctrl Pts',(0.525933334162556,-0.254319232363049,
-0.939198248544427));
#34019=CARTESIAN_POINT('Ctrl Pts',(0.507057380724533,-0.237895043532788,
-0.949440676105255));
#34020=CARTESIAN_POINT('Ctrl Pts',(0.473077587363686,-0.199697230012983,
-0.966820759530997));
#34021=CARTESIAN_POINT('Ctrl Pts',(0.457978755888596,-0.177924977804098,
-0.973971221090534));
#34022=CARTESIAN_POINT('Ctrl Pts',(0.430199341854858,-0.124911173756694,
-0.986608710139579));
#34023=CARTESIAN_POINT('Ctrl Pts',(0.419070565453384,-0.0925528133349865,
-0.991263089003441));
#34024=CARTESIAN_POINT('Ctrl Pts',(0.413083465285518,-0.05953,-0.993751811093549));
#34025=CARTESIAN_POINT('Origin',(0.685838782044607,-0.05953,-0.860014630714833));
#34026=CARTESIAN_POINT('Origin',(0.,-0.208355,0.));
#34027=CARTESIAN_POINT('',(-1.076188,-0.35718,1.31795018948079E-16));
#34028=CARTESIAN_POINT('Origin',(0.,-0.35718,0.));
#34029=CARTESIAN_POINT('',(-1.076188,-0.208355,1.31795018948079E-16));
#34030=CARTESIAN_POINT('',(1.03449977959455,-0.05953,0.296632461748266));
#34031=CARTESIAN_POINT('Origin',(0.,-0.05953,0.));
#34032=CARTESIAN_POINT('',(1.03449977959455,-0.05953,-0.296632461748266));
#34033=CARTESIAN_POINT('Ctrl Pts',(1.03449977959455,-0.05953,0.296632461748267));
#34034=CARTESIAN_POINT('Ctrl Pts',(1.03628691421076,-0.0925528133349865,
0.290399865505497));
#34035=CARTESIAN_POINT('Ctrl Pts',(1.03958665287714,-0.124911173756694,
0.278797079997872));
#34036=CARTESIAN_POINT('Ctrl Pts',(1.0470264474309,-0.177924977804098,0.249198913998601));
#34037=CARTESIAN_POINT('Ctrl Pts',(1.05084995891418,-0.199697230012983,
0.232935932341942));
#34038=CARTESIAN_POINT('Ctrl Pts',(1.05844771715377,-0.237895043532788,
0.195533155353269));
#34039=CARTESIAN_POINT('Ctrl Pts',(1.06220882929878,-0.254319232363049,
0.17438929156337));
#34040=CARTESIAN_POINT('Ctrl Pts',(1.06849922508772,-0.28018331644634,0.130252399648131));
#34041=CARTESIAN_POINT('Ctrl Pts',(1.07137013248666,-0.29104845371857,0.105070977154072));
#34042=CARTESIAN_POINT('Ctrl Pts',(1.07522652957392,-0.30527573347708,0.0525526752791107));
#34043=CARTESIAN_POINT('Ctrl Pts',(1.076188,-0.308638795020976,0.025214283908933));
#34044=CARTESIAN_POINT('Ctrl Pts',(1.076188,-0.308638795020976,-0.025214283908933));
#34045=CARTESIAN_POINT('Ctrl Pts',(1.07522652957392,-0.30527573347708,-0.0525526752791107));
#34046=CARTESIAN_POINT('Ctrl Pts',(1.07137013248666,-0.29104845371857,-0.105070977154072));
#34047=CARTESIAN_POINT('Ctrl Pts',(1.06849922508772,-0.28018331644634,-0.130252399648131));
#34048=CARTESIAN_POINT('Ctrl Pts',(1.06220882929878,-0.254319232363049,
-0.17438929156337));
#34049=CARTESIAN_POINT('Ctrl Pts',(1.05844771715377,-0.237895043532788,
-0.195533155353269));
#34050=CARTESIAN_POINT('Ctrl Pts',(1.05084995891418,-0.199697230012983,
-0.232935932341942));
#34051=CARTESIAN_POINT('Ctrl Pts',(1.0470264474309,-0.177924977804098,-0.249198913998601));
#34052=CARTESIAN_POINT('Ctrl Pts',(1.03958665287714,-0.124911173756694,
-0.278797079997872));
#34053=CARTESIAN_POINT('Ctrl Pts',(1.03628691421076,-0.0925528133349865,
-0.290399865505497));
#34054=CARTESIAN_POINT('Ctrl Pts',(1.03449977959455,-0.05953,-0.296632461748267));
#34055=CARTESIAN_POINT('Origin',(0.,-0.05953,0.));
#34056=CARTESIAN_POINT('Origin',(0.,-0.05953,0.));
#34057=CARTESIAN_POINT('Origin',(1.1,-0.05953,0.));
#34058=CARTESIAN_POINT('Origin',(1.1,0.,0.));
#34059=CARTESIAN_POINT('Origin',(1.1,-0.05953,0.));
#34060=CARTESIAN_POINT('Origin',(0.,-0.35718,0.));
#34061=CARTESIAN_POINT('Origin',(0.,-0.05953,0.));
#34062=CARTESIAN_POINT('',(0.,0.,0.));
#34063=CARTESIAN_POINT('Origin',(1.119765,0.495,0.));
#34064=CARTESIAN_POINT('',(-1.119765,0.495,-1.37131662304724E-16));
#34065=CARTESIAN_POINT('Origin',(0.,0.495,0.));
#34066=CARTESIAN_POINT('',(-1.085235,0.495,-1.32902956907268E-16));
#34067=CARTESIAN_POINT('Origin',(0.,0.495,0.));
#34068=CARTESIAN_POINT('Origin',(0.,0.4575,0.));
#34069=CARTESIAN_POINT('',(-1.119765,0.42,-1.37131662304724E-16));
#34070=CARTESIAN_POINT('Origin',(0.,0.42,0.));
#34071=CARTESIAN_POINT('',(-1.119765,0.4575,-1.37131662304724E-16));
#34072=CARTESIAN_POINT('Origin',(1.085235,0.42,0.));
#34073=CARTESIAN_POINT('',(-1.085235,0.42,-1.32902956907268E-16));
#34074=CARTESIAN_POINT('Origin',(0.,0.42,0.));
#34075=CARTESIAN_POINT('Origin',(0.,0.4575,0.));
#34076=CARTESIAN_POINT('',(-1.085235,0.4575,-1.32902956907268E-16));
#34077=CARTESIAN_POINT('Origin',(1.119765,-0.42,0.));
#34078=CARTESIAN_POINT('',(-1.119765,-0.42,-1.37131662304724E-16));
#34079=CARTESIAN_POINT('Origin',(0.,-0.42,0.));
#34080=CARTESIAN_POINT('',(-1.085235,-0.42,-1.32902956907268E-16));
#34081=CARTESIAN_POINT('Origin',(0.,-0.42,0.));
#34082=CARTESIAN_POINT('Origin',(0.,-0.4575,0.));
#34083=CARTESIAN_POINT('',(-1.119765,-0.495,-1.37131662304724E-16));
#34084=CARTESIAN_POINT('Origin',(0.,-0.495,0.));
#34085=CARTESIAN_POINT('',(-1.119765,-0.4575,-1.37131662304724E-16));
#34086=CARTESIAN_POINT('Origin',(1.085235,-0.495,0.));
#34087=CARTESIAN_POINT('',(-1.085235,-0.495,-1.32902956907268E-16));
#34088=CARTESIAN_POINT('Origin',(0.,-0.495,0.));
#34089=CARTESIAN_POINT('Origin',(0.,-0.4575,0.));
#34090=CARTESIAN_POINT('',(-1.085235,-0.4575,-1.32902956907268E-16));
#34091=CARTESIAN_POINT('',(0.,0.,0.));
#34092=CARTESIAN_POINT('',(0.,0.,0.));
#34093=CARTESIAN_POINT('',(0.,0.,0.));
#34094=CARTESIAN_POINT('',(0.,0.,0.));
#34095=CARTESIAN_POINT('',(0.,0.,0.));
#34096=CARTESIAN_POINT('',(0.,0.,0.));
#34097=CARTESIAN_POINT('',(0.,0.,0.));
#34098=CARTESIAN_POINT('Origin',(0.,0.,0.));
#34099=CARTESIAN_POINT('',(-1.63531,-0.410863395882378,-2.00267715711366E-16));
#34100=CARTESIAN_POINT('',(-2.00267715711366E-16,-0.410863395882378,1.63531));
#34101=CARTESIAN_POINT('Origin',(0.,-0.410863395882378,0.));
#34102=CARTESIAN_POINT('Origin',(0.,-0.410863395882378,0.));
#34103=CARTESIAN_POINT('',(-2.00267715711366E-16,0.410863395882378,1.63531));
#34104=CARTESIAN_POINT('Origin',(-2.05128338857182E-16,0.,1.675));
#34105=CARTESIAN_POINT('',(-1.63531,0.410863395882378,2.00267715711366E-16));
#34106=CARTESIAN_POINT('Origin',(0.,0.410863395882378,0.));
#34107=CARTESIAN_POINT('Origin',(0.,0.410863395882378,0.));
#34108=CARTESIAN_POINT('Origin',(0.,0.,0.));
#34109=CARTESIAN_POINT('',(-1.63531,0.7,-2.00267715711366E-16));
#34110=CARTESIAN_POINT('',(-1.63531,0.,-2.00267715711366E-16));
#34111=CARTESIAN_POINT('Origin',(0.,0.7,0.));
#34112=CARTESIAN_POINT('Origin',(0.,0.,0.));
#34113=CARTESIAN_POINT('',(-1.,-0.6,-1.22464679914735E-16));
#34114=CARTESIAN_POINT('Origin',(0.,-0.6,0.));
#34115=CARTESIAN_POINT('',(-1.,0.6,-1.22464679914735E-16));
#34116=CARTESIAN_POINT('',(-1.,0.,-1.22464679914735E-16));
#34117=CARTESIAN_POINT('Origin',(0.,0.6,0.));
#34118=CARTESIAN_POINT('Origin',(0.,0.65,0.));
#34119=CARTESIAN_POINT('',(-1.1,0.7,-1.34711147906209E-16));
#34120=CARTESIAN_POINT('',(-1.05,0.65,-1.28587913910472E-16));
#34121=CARTESIAN_POINT('Origin',(0.,0.7,0.));
#34122=CARTESIAN_POINT('Origin',(1.63531,0.7,0.));
#34123=CARTESIAN_POINT('Origin',(0.,0.,0.));
#34124=CARTESIAN_POINT('',(-1.63531,-0.7,-2.00267715711366E-16));
#34125=CARTESIAN_POINT('Origin',(0.,-0.7,0.));
#34126=CARTESIAN_POINT('',(-1.63531,0.,-2.00267715711366E-16));
#34127=CARTESIAN_POINT('Origin',(1.1,-0.7,0.));
#34128=CARTESIAN_POINT('',(-1.1,-0.7,-1.34711147906209E-16));
#34129=CARTESIAN_POINT('Origin',(0.,-0.7,0.));
#34130=CARTESIAN_POINT('Origin',(0.,-0.65,0.));
#34131=CARTESIAN_POINT('',(-1.05,-0.65,-1.28587913910472E-16));
#34132=CARTESIAN_POINT('',(0.,0.,0.));
#34133=CARTESIAN_POINT('Origin',(0.,0.,0.));
#34134=CARTESIAN_POINT('',(-1.71469,0.410863395882378,-2.09988962002998E-16));
#34135=CARTESIAN_POINT('',(-2.09988962002998E-16,0.410863395882378,1.71469));
#34136=CARTESIAN_POINT('Origin',(0.,0.410863395882378,0.));
#34137=CARTESIAN_POINT('Origin',(0.,0.410863395882378,0.));
#34138=CARTESIAN_POINT('',(-2.09988962002998E-16,-0.410863395882378,1.71469));
#34139=CARTESIAN_POINT('Origin',(-2.05128338857182E-16,0.,1.675));
#34140=CARTESIAN_POINT('',(-1.71469,-0.410863395882378,2.09988962002998E-16));
#34141=CARTESIAN_POINT('Origin',(0.,-0.410863395882378,0.));
#34142=CARTESIAN_POINT('Origin',(0.,-0.410863395882378,0.));
#34143=CARTESIAN_POINT('Origin',(0.,0.,0.));
#34144=CARTESIAN_POINT('',(-1.71469,-0.7,-2.09988962002998E-16));
#34145=CARTESIAN_POINT('Origin',(0.,-0.7,0.));
#34146=CARTESIAN_POINT('',(-1.71469,0.,-2.09988962002998E-16));
#34147=CARTESIAN_POINT('Origin',(2.25,0.7,0.));
#34148=CARTESIAN_POINT('',(-2.25,0.7,-2.75545529808154E-16));
#34149=CARTESIAN_POINT('Origin',(0.,0.7,0.));
#34150=CARTESIAN_POINT('',(-1.71469,0.7,-2.09988962002998E-16));
#34151=CARTESIAN_POINT('Origin',(0.,0.7,0.));
#34152=CARTESIAN_POINT('Origin',(0.,0.65,0.));
#34153=CARTESIAN_POINT('',(-2.35,0.6,-2.87791997799628E-16));
#34154=CARTESIAN_POINT('Origin',(0.,0.6,0.));
#34155=CARTESIAN_POINT('',(-2.3,0.65,-2.81668763803891E-16));
#34156=CARTESIAN_POINT('Origin',(0.,0.,0.));
#34157=CARTESIAN_POINT('',(-2.35,-0.6,-2.87791997799628E-16));
#34158=CARTESIAN_POINT('Origin',(0.,-0.6,0.));
#34159=CARTESIAN_POINT('',(-2.35,0.,-2.87791997799628E-16));
#34160=CARTESIAN_POINT('Origin',(0.,-0.65,0.));
#34161=CARTESIAN_POINT('',(-2.25,-0.7,-2.75545529808154E-16));
#34162=CARTESIAN_POINT('Origin',(0.,-0.7,0.));
#34163=CARTESIAN_POINT('',(-2.3,-0.65,-2.81668763803891E-16));
#34164=CARTESIAN_POINT('Origin',(1.71469,-0.7,0.));
#34165=CARTESIAN_POINT('Origin',(0.,0.,0.));
#34166=CARTESIAN_POINT('',(-1.71469,0.,-2.09988962002998E-16));
#34167=CARTESIAN_POINT('',(0.,0.,0.));
#34168=CARTESIAN_POINT('Origin',(1.675,0.,0.));
#34169=CARTESIAN_POINT('',(1.675,-2.97627328869245E-33,0.3969));
#34170=CARTESIAN_POINT('',(1.675,-2.97627328869245E-33,-0.3969));
#34171=CARTESIAN_POINT('Origin',(1.675,0.,0.));
#34172=CARTESIAN_POINT('Origin',(1.18440385848747,0.,-1.18440385848747));
#34173=CARTESIAN_POINT('',(1.46505453994041,3.1867025333467E-33,-0.903753177034526));
#34174=CARTESIAN_POINT('',(0.903753177034527,-9.13924911073161E-33,-1.46505453994041));
#34175=CARTESIAN_POINT('Origin',(1.18440385848747,0.,-1.18440385848747));
#34176=CARTESIAN_POINT('Origin',(1.02564169428591E-16,0.,-1.675));
#34177=CARTESIAN_POINT('',(0.3969,-2.97627328869246E-33,-1.675));
#34178=CARTESIAN_POINT('',(-0.3969,-2.97627328869245E-33,-1.675));
#34179=CARTESIAN_POINT('Origin',(1.02564169428591E-16,0.,-1.675));
#34180=CARTESIAN_POINT('Origin',(-1.18440385848747,0.,-1.18440385848747));
#34181=CARTESIAN_POINT('',(-0.903753177034526,3.1867025333467E-33,-1.46505453994041));
#34182=CARTESIAN_POINT('',(-1.46505453994041,-9.13924911073161E-33,-0.903753177034527));
#34183=CARTESIAN_POINT('Origin',(-1.18440385848747,0.,-1.18440385848747));
#34184=CARTESIAN_POINT('Origin',(-1.675,0.,-2.05128338857182E-16));
#34185=CARTESIAN_POINT('',(-1.675,-2.97627328869246E-33,-0.3969));
#34186=CARTESIAN_POINT('',(-1.675,-2.97627328869245E-33,0.3969));
#34187=CARTESIAN_POINT('Origin',(-1.675,0.,-2.05128338857182E-16));
#34188=CARTESIAN_POINT('Origin',(-1.18440385848747,0.,1.18440385848747));
#34189=CARTESIAN_POINT('',(-1.46505453994041,6.26819044436628E-33,0.903753177034526));
#34190=CARTESIAN_POINT('',(-0.903753177034527,-1.22207370217512E-32,1.46505453994041));
#34191=CARTESIAN_POINT('Origin',(-1.18440385848747,0.,1.18440385848747));
#34192=CARTESIAN_POINT('Origin',(-3.07692508285772E-16,0.,1.675));
#34193=CARTESIAN_POINT('',(-0.3969,-2.97627328869246E-33,1.675));
#34194=CARTESIAN_POINT('',(0.396899999999999,-2.97627328869245E-33,1.675));
#34195=CARTESIAN_POINT('Origin',(-3.07692508285772E-16,0.,1.675));
#34196=CARTESIAN_POINT('Origin',(1.18440385848747,0.,1.18440385848747));
#34197=CARTESIAN_POINT('',(0.903753177034526,9.34967835538585E-33,1.46505453994041));
#34198=CARTESIAN_POINT('',(1.46505453994041,-1.53022249327708E-32,0.903753177034527));
#34199=CARTESIAN_POINT('Origin',(1.18440385848747,0.,1.18440385848747));
#34200=CARTESIAN_POINT('',(0.,0.,0.));
#34201=CARTESIAN_POINT('Origin',(1.18440385848747,0.,1.18440385848747));
#34202=CARTESIAN_POINT('',(0.846804978391753,-0.07938,1.40825612658882));
#34203=CARTESIAN_POINT('',(1.40825612658882,-0.07938,0.846804978391754));
#34204=CARTESIAN_POINT('Ctrl Pts',(0.846804978391752,-0.0793800000000001,
1.40825612658882));
#34205=CARTESIAN_POINT('Ctrl Pts',(0.854205272175554,-0.123401821157026,
1.40380622184538));
#34206=CARTESIAN_POINT('Ctrl Pts',(0.867957148219441,-0.166543350814306,
1.39550172959303));
#34207=CARTESIAN_POINT('Ctrl Pts',(0.902193646979982,-0.237231147975234,
1.3735491215176));
#34208=CARTESIAN_POINT('Ctrl Pts',(0.920778333482564,-0.266264900654909,
1.36127834356734));
#34209=CARTESIAN_POINT('Ctrl Pts',(0.962485392528369,-0.317195968905306,
1.33211611256184));
#34210=CARTESIAN_POINT('Ctrl Pts',(0.985600426557816,-0.33909093068465,
1.31521005565926));
#34211=CARTESIAN_POINT('Ctrl Pts',(1.03253285680459,-0.373586846396559,
1.27866649102984));
#34212=CARTESIAN_POINT('Ctrl Pts',(1.05871835910697,-0.388086240756494,
1.25722555095714));
#34213=CARTESIAN_POINT('Ctrl Pts',(1.11153475808518,-0.407068917407805,
1.2107812086231));
#34214=CARTESIAN_POINT('Ctrl Pts',(1.13814686046673,-0.411552957311693,
1.18575674747573));
#34215=CARTESIAN_POINT('Ctrl Pts',(1.18575674747573,-0.411552957311693,
1.13814686046673));
#34216=CARTESIAN_POINT('Ctrl Pts',(1.2107812086231,-0.407068917407805,1.11153475808518));
#34217=CARTESIAN_POINT('Ctrl Pts',(1.25722555095713,-0.388086240756494,
1.05871835910697));
#34218=CARTESIAN_POINT('Ctrl Pts',(1.27866649102984,-0.373586846396559,
1.03253285680459));
#34219=CARTESIAN_POINT('Ctrl Pts',(1.31521005565926,-0.33909093068465,0.985600426557816));
#34220=CARTESIAN_POINT('Ctrl Pts',(1.33211611256184,-0.317195968905306,
0.962485392528369));
#34221=CARTESIAN_POINT('Ctrl Pts',(1.36127834356734,-0.266264900654909,
0.920778333482565));
#34222=CARTESIAN_POINT('Ctrl Pts',(1.3735491215176,-0.237231147975234,0.902193646979983));
#34223=CARTESIAN_POINT('Ctrl Pts',(1.39550172959303,-0.166543350814306,
0.867957148219442));
#34224=CARTESIAN_POINT('Ctrl Pts',(1.40380622184538,-0.123401821157026,
0.854205272175555));
#34225=CARTESIAN_POINT('Ctrl Pts',(1.40825612658882,-0.0793800000000001,
0.846804978391753));
#34226=CARTESIAN_POINT('',(0.886256117232623,-0.07938,1.45861320581289));
#34227=CARTESIAN_POINT('Origin',(1.18440385848747,-0.07938,1.18440385848747));
#34228=CARTESIAN_POINT('',(1.45861320581289,-0.07938,0.886256117232624));
#34229=CARTESIAN_POINT('Ctrl Pts',(1.45861320581289,-0.0793800000000001,
0.886256117232623));
#34230=CARTESIAN_POINT('Ctrl Pts',(1.45630208793976,-0.101649918886749,
0.890059788636852));
#34231=CARTESIAN_POINT('Ctrl Pts',(1.45296717977858,-0.123823518623746,
0.895520212222107));
#34232=CARTESIAN_POINT('Ctrl Pts',(1.43904931717599,-0.192480977588836,
0.917859913453975));
#34233=CARTESIAN_POINT('Ctrl Pts',(1.4243271592157,-0.236152929235938,0.940896403863072));
#34234=CARTESIAN_POINT('Ctrl Pts',(1.39055359345152,-0.303141259068212,
0.990027513266106));
#34235=CARTESIAN_POINT('Ctrl Pts',(1.36743459453896,-0.335108247315849,
1.02199477007745));
#34236=CARTESIAN_POINT('Ctrl Pts',(1.32643091652006,-0.373243761060364,
1.07446535104584));
#34237=CARTESIAN_POINT('Ctrl Pts',(1.30441816675528,-0.387888272594439,
1.10126842659597));
#34238=CARTESIAN_POINT('Ctrl Pts',(1.25681160160691,-0.407041111792943,
1.15530234155453));
#34239=CARTESIAN_POINT('Ctrl Pts',(1.23119764287622,-0.411552957311693,
1.18251418313119));
#34240=CARTESIAN_POINT('Ctrl Pts',(1.18251418313119,-0.411552957311693,
1.23119764287622));
#34241=CARTESIAN_POINT('Ctrl Pts',(1.15530234155453,-0.407041111792943,
1.25681160160691));
#34242=CARTESIAN_POINT('Ctrl Pts',(1.10126842659597,-0.387888272594439,
1.30441816675528));
#34243=CARTESIAN_POINT('Ctrl Pts',(1.07446535104584,-0.373243761060364,
1.32643091652006));
#34244=CARTESIAN_POINT('Ctrl Pts',(1.02199477007745,-0.335108247315848,
1.36743459453896));
#34245=CARTESIAN_POINT('Ctrl Pts',(0.990027513266105,-0.303141259068211,
1.39055359345152));
#34246=CARTESIAN_POINT('Ctrl Pts',(0.940896403863071,-0.236152929235937,
1.42432715921571));
#34247=CARTESIAN_POINT('Ctrl Pts',(0.917859913453974,-0.192480977588835,
1.43904931717599));
#34248=CARTESIAN_POINT('Ctrl Pts',(0.895520212222106,-0.123823518623745,
1.45296717977858));
#34249=CARTESIAN_POINT('Ctrl Pts',(0.890059788636851,-0.101649918886749,
1.45630208793976));
#34250=CARTESIAN_POINT('Ctrl Pts',(0.886256117232622,-0.0793800000000001,
1.45861320581289));
#34251=CARTESIAN_POINT('Origin',(1.18440385848747,-0.07938,1.18440385848747));
#34252=CARTESIAN_POINT('Origin',(0.,-0.27783,0.));
#34253=CARTESIAN_POINT('',(0.404717578595295,-0.07938,1.65807299932179));
#34254=CARTESIAN_POINT('Origin',(0.,-0.07938,0.));
#34255=CARTESIAN_POINT('',(-0.404717578595296,-0.07938,1.65807299932179));
#34256=CARTESIAN_POINT('Ctrl Pts',(0.404717578595296,-0.0793800000000001,
1.65807299932179));
#34257=CARTESIAN_POINT('Ctrl Pts',(0.400393769631747,-0.101649918886749,
1.65912839404491));
#34258=CARTESIAN_POINT('Ctrl Pts',(0.394174530911058,-0.123823518623745,
1.66063136041479));
#34259=CARTESIAN_POINT('Ctrl Pts',(0.368536561654407,-0.192480977588835,
1.66658649961961));
#34260=CARTESIAN_POINT('Ctrl Pts',(0.341837165343982,-0.236152929235937,
1.67246562047521));
#34261=CARTESIAN_POINT('Ctrl Pts',(0.283214707341173,-0.303141259068211,
1.68332504372461));
#34262=CARTESIAN_POINT('Ctrl Pts',(0.244262842368623,-0.335108247315849,
1.68958170688653));
#34263=CARTESIAN_POINT('Ctrl Pts',(0.178166559972324,-0.373243761060364,
1.69769003172132));
#34264=CARTESIAN_POINT('Ctrl Pts',(0.143648558862931,-0.387888272594439,
1.70107730356824));
#34265=CARTESIAN_POINT('Ctrl Pts',(0.0717778861362652,-0.407041111792943,
1.70562212620408));
#34266=CARTESIAN_POINT('Ctrl Pts',(0.0344244045173309,-0.411552957311693,
1.706752));
#34267=CARTESIAN_POINT('Ctrl Pts',(-0.0344244045173315,-0.411552957311693,
1.706752));
#34268=CARTESIAN_POINT('Ctrl Pts',(-0.0717778861362658,-0.407041111792943,
1.70562212620408));
#34269=CARTESIAN_POINT('Ctrl Pts',(-0.143648558862932,-0.387888272594439,
1.70107730356824));
#34270=CARTESIAN_POINT('Ctrl Pts',(-0.178166559972325,-0.373243761060364,
1.69769003172132));
#34271=CARTESIAN_POINT('Ctrl Pts',(-0.244262842368624,-0.335108247315849,
1.68958170688653));
#34272=CARTESIAN_POINT('Ctrl Pts',(-0.283214707341173,-0.303141259068212,
1.68332504372461));
#34273=CARTESIAN_POINT('Ctrl Pts',(-0.341837165343982,-0.236152929235937,
1.67246562047521));
#34274=CARTESIAN_POINT('Ctrl Pts',(-0.368536561654408,-0.192480977588835,
1.66658649961961));
#34275=CARTESIAN_POINT('Ctrl Pts',(-0.394174530911059,-0.123823518623745,
1.66063136041479));
#34276=CARTESIAN_POINT('Ctrl Pts',(-0.400393769631748,-0.101649918886749,
1.65912839404491));
#34277=CARTESIAN_POINT('Ctrl Pts',(-0.404717578595297,-0.0793800000000001,
1.65807299932179));
#34278=CARTESIAN_POINT('',(-0.886256117232624,-0.07938,1.45861320581289));
#34279=CARTESIAN_POINT('Origin',(0.,-0.07938,0.));
#34280=CARTESIAN_POINT('',(-1.45861320581289,-0.07938,0.886256117232623));
#34281=CARTESIAN_POINT('Ctrl Pts',(-0.886256117232623,-0.0793800000000001,
1.45861320581289));
#34282=CARTESIAN_POINT('Ctrl Pts',(-0.890059788636852,-0.101649918886749,
1.45630208793976));
#34283=CARTESIAN_POINT('Ctrl Pts',(-0.895520212222106,-0.123823518623745,
1.45296717977858));
#34284=CARTESIAN_POINT('Ctrl Pts',(-0.917859913453974,-0.192480977588835,
1.43904931717599));
#34285=CARTESIAN_POINT('Ctrl Pts',(-0.940896403863071,-0.236152929235937,
1.4243271592157));
#34286=CARTESIAN_POINT('Ctrl Pts',(-0.990027513266105,-0.303141259068211,
1.39055359345152));
#34287=CARTESIAN_POINT('Ctrl Pts',(-1.02199477007745,-0.335108247315848,
1.36743459453896));
#34288=CARTESIAN_POINT('Ctrl Pts',(-1.07446535104584,-0.373243761060364,
1.32643091652006));
#34289=CARTESIAN_POINT('Ctrl Pts',(-1.10126842659597,-0.387888272594439,
1.30441816675528));
#34290=CARTESIAN_POINT('Ctrl Pts',(-1.15530234155453,-0.407041111792943,
1.25681160160691));
#34291=CARTESIAN_POINT('Ctrl Pts',(-1.18251418313119,-0.411552957311693,
1.23119764287622));
#34292=CARTESIAN_POINT('Ctrl Pts',(-1.23119764287622,-0.411552957311693,
1.18251418313119));
#34293=CARTESIAN_POINT('Ctrl Pts',(-1.25681160160691,-0.407041111792943,
1.15530234155453));
#34294=CARTESIAN_POINT('Ctrl Pts',(-1.30441816675528,-0.387888272594439,
1.10126842659597));
#34295=CARTESIAN_POINT('Ctrl Pts',(-1.32643091652006,-0.373243761060365,
1.07446535104584));
#34296=CARTESIAN_POINT('Ctrl Pts',(-1.36743459453896,-0.335108247315849,
1.02199477007745));
#34297=CARTESIAN_POINT('Ctrl Pts',(-1.39055359345152,-0.303141259068212,
0.990027513266106));
#34298=CARTESIAN_POINT('Ctrl Pts',(-1.4243271592157,-0.236152929235938,
0.940896403863071));
#34299=CARTESIAN_POINT('Ctrl Pts',(-1.43904931717599,-0.192480977588836,
0.917859913453974));
#34300=CARTESIAN_POINT('Ctrl Pts',(-1.45296717977858,-0.123823518623746,
0.895520212222106));
#34301=CARTESIAN_POINT('Ctrl Pts',(-1.45630208793976,-0.101649918886749,
0.890059788636852));
#34302=CARTESIAN_POINT('Ctrl Pts',(-1.45861320581289,-0.0793800000000001,
0.886256117232623));
#34303=CARTESIAN_POINT('',(-1.65807299932179,-0.07938,0.404717578595295));
#34304=CARTESIAN_POINT('Origin',(0.,-0.07938,0.));
#34305=CARTESIAN_POINT('',(-1.706752,-0.411552957311693,2.08591827245526E-16));
#34306=CARTESIAN_POINT('Ctrl Pts',(-1.65807299932179,-0.0793800000000001,
0.404717578595296));
#34307=CARTESIAN_POINT('Ctrl Pts',(-1.65912839404491,-0.101649918886749,
0.400393769631747));
#34308=CARTESIAN_POINT('Ctrl Pts',(-1.66063136041479,-0.123823518623745,
0.394174530911058));
#34309=CARTESIAN_POINT('Ctrl Pts',(-1.66658649961961,-0.192480977588835,
0.368536561654407));
#34310=CARTESIAN_POINT('Ctrl Pts',(-1.67246562047521,-0.236152929235937,
0.341837165343982));
#34311=CARTESIAN_POINT('Ctrl Pts',(-1.68332504372461,-0.303141259068211,
0.283214707341173));
#34312=CARTESIAN_POINT('Ctrl Pts',(-1.68958170688653,-0.335108247315848,
0.244262842368623));
#34313=CARTESIAN_POINT('Ctrl Pts',(-1.69769003172132,-0.373243761060364,
0.178166559972324));
#34314=CARTESIAN_POINT('Ctrl Pts',(-1.70107730356824,-0.387888272594439,
0.143648558862931));
#34315=CARTESIAN_POINT('Ctrl Pts',(-1.70562212620408,-0.407041111792943,
0.0717778861362656));
#34316=CARTESIAN_POINT('Ctrl Pts',(-1.706752,-0.411552957311693,0.0344244045173313));
#34317=CARTESIAN_POINT('Ctrl Pts',(-1.706752,-0.411552957311693,2.08166817117217E-16));
#34318=CARTESIAN_POINT('',(-1.706752,-0.47628,2.09016837373834E-16));
#34319=CARTESIAN_POINT('',(-1.706752,-0.27783,2.09016837373834E-16));
#34320=CARTESIAN_POINT('Origin',(0.,-0.47628,0.));
#34321=CARTESIAN_POINT('',(-1.65807299932179,-0.07938,-0.404717578595296));
#34322=CARTESIAN_POINT('Ctrl Pts',(-1.706752,-0.411552957311693,2.0122792321331E-16));
#34323=CARTESIAN_POINT('Ctrl Pts',(-1.706752,-0.411552957311693,-0.0344244045173309));
#34324=CARTESIAN_POINT('Ctrl Pts',(-1.70562212620408,-0.407041111792943,
-0.0717778861362652));
#34325=CARTESIAN_POINT('Ctrl Pts',(-1.70107730356824,-0.387888272594439,
-0.143648558862931));
#34326=CARTESIAN_POINT('Ctrl Pts',(-1.69769003172132,-0.373243761060365,
-0.178166559972324));
#34327=CARTESIAN_POINT('Ctrl Pts',(-1.68958170688653,-0.335108247315849,
-0.244262842368623));
#34328=CARTESIAN_POINT('Ctrl Pts',(-1.68332504372461,-0.303141259068212,
-0.283214707341173));
#34329=CARTESIAN_POINT('Ctrl Pts',(-1.67246562047521,-0.236152929235938,
-0.341837165343982));
#34330=CARTESIAN_POINT('Ctrl Pts',(-1.66658649961961,-0.192480977588836,
-0.368536561654407));
#34331=CARTESIAN_POINT('Ctrl Pts',(-1.66063136041479,-0.123823518623745,
-0.394174530911059));
#34332=CARTESIAN_POINT('Ctrl Pts',(-1.65912839404491,-0.101649918886749,
-0.400393769631748));
#34333=CARTESIAN_POINT('Ctrl Pts',(-1.65807299932179,-0.0793800000000001,
-0.404717578595296));
#34334=CARTESIAN_POINT('',(-1.45861320581289,-0.07938,-0.886256117232623));
#34335=CARTESIAN_POINT('Origin',(0.,-0.07938,0.));
#34336=CARTESIAN_POINT('',(-0.886256117232623,-0.07938,-1.45861320581289));
#34337=CARTESIAN_POINT('Ctrl Pts',(-1.45861320581289,-0.0793800000000001,
-0.886256117232623));
#34338=CARTESIAN_POINT('Ctrl Pts',(-1.45630208793976,-0.101649918886749,
-0.890059788636852));
#34339=CARTESIAN_POINT('Ctrl Pts',(-1.45296717977858,-0.123823518623745,
-0.895520212222106));
#34340=CARTESIAN_POINT('Ctrl Pts',(-1.43904931717599,-0.192480977588835,
-0.917859913453974));
#34341=CARTESIAN_POINT('Ctrl Pts',(-1.4243271592157,-0.236152929235937,
-0.940896403863072));
#34342=CARTESIAN_POINT('Ctrl Pts',(-1.39055359345152,-0.303141259068212,
-0.990027513266106));
#34343=CARTESIAN_POINT('Ctrl Pts',(-1.36743459453896,-0.335108247315849,
-1.02199477007745));
#34344=CARTESIAN_POINT('Ctrl Pts',(-1.32643091652006,-0.373243761060364,
-1.07446535104584));
#34345=CARTESIAN_POINT('Ctrl Pts',(-1.30441816675528,-0.387888272594439,
-1.10126842659597));
#34346=CARTESIAN_POINT('Ctrl Pts',(-1.25681160160691,-0.407041111792943,
-1.15530234155453));
#34347=CARTESIAN_POINT('Ctrl Pts',(-1.23119764287622,-0.411552957311693,
-1.18251418313119));
#34348=CARTESIAN_POINT('Ctrl Pts',(-1.18251418313119,-0.411552957311693,
-1.23119764287622));
#34349=CARTESIAN_POINT('Ctrl Pts',(-1.15530234155453,-0.407041111792943,
-1.25681160160691));
#34350=CARTESIAN_POINT('Ctrl Pts',(-1.10126842659597,-0.387888272594439,
-1.30441816675528));
#34351=CARTESIAN_POINT('Ctrl Pts',(-1.07446535104584,-0.373243761060364,
-1.32643091652006));
#34352=CARTESIAN_POINT('Ctrl Pts',(-1.02199477007745,-0.335108247315848,
-1.36743459453896));
#34353=CARTESIAN_POINT('Ctrl Pts',(-0.990027513266105,-0.303141259068211,
-1.39055359345152));
#34354=CARTESIAN_POINT('Ctrl Pts',(-0.940896403863071,-0.236152929235936,
-1.42432715921571));
#34355=CARTESIAN_POINT('Ctrl Pts',(-0.917859913453974,-0.192480977588835,
-1.43904931717599));
#34356=CARTESIAN_POINT('Ctrl Pts',(-0.895520212222106,-0.123823518623745,
-1.45296717977858));
#34357=CARTESIAN_POINT('Ctrl Pts',(-0.890059788636851,-0.101649918886749,
-1.45630208793976));
#34358=CARTESIAN_POINT('Ctrl Pts',(-0.886256117232623,-0.0793800000000001,
-1.45861320581289));
#34359=CARTESIAN_POINT('',(-0.404717578595295,-0.07938,-1.65807299932179));
#34360=CARTESIAN_POINT('Origin',(0.,-0.07938,0.));
#34361=CARTESIAN_POINT('',(0.404717578595296,-0.07938,-1.65807299932179));
#34362=CARTESIAN_POINT('Ctrl Pts',(-0.404717578595296,-0.0793800000000001,
-1.65807299932179));
#34363=CARTESIAN_POINT('Ctrl Pts',(-0.400393769631747,-0.101649918886749,
-1.65912839404491));
#34364=CARTESIAN_POINT('Ctrl Pts',(-0.394174530911058,-0.123823518623746,
-1.66063136041479));
#34365=CARTESIAN_POINT('Ctrl Pts',(-0.368536561654407,-0.192480977588836,
-1.66658649961961));
#34366=CARTESIAN_POINT('Ctrl Pts',(-0.341837165343982,-0.236152929235938,
-1.67246562047521));
#34367=CARTESIAN_POINT('Ctrl Pts',(-0.283214707341173,-0.303141259068212,
-1.68332504372461));
#34368=CARTESIAN_POINT('Ctrl Pts',(-0.244262842368623,-0.335108247315849,
-1.68958170688653));
#34369=CARTESIAN_POINT('Ctrl Pts',(-0.178166559972324,-0.373243761060364,
-1.69769003172132));
#34370=CARTESIAN_POINT('Ctrl Pts',(-0.143648558862931,-0.387888272594439,
-1.70107730356824));
#34371=CARTESIAN_POINT('Ctrl Pts',(-0.0717778861362653,-0.407041111792943,
-1.70562212620408));
#34372=CARTESIAN_POINT('Ctrl Pts',(-0.034424404517331,-0.411552957311693,
-1.706752));
#34373=CARTESIAN_POINT('Ctrl Pts',(0.0344244045173312,-0.411552957311693,
-1.706752));
#34374=CARTESIAN_POINT('Ctrl Pts',(0.0717778861362655,-0.407041111792943,
-1.70562212620408));
#34375=CARTESIAN_POINT('Ctrl Pts',(0.143648558862931,-0.387888272594439,
-1.70107730356824));
#34376=CARTESIAN_POINT('Ctrl Pts',(0.178166559972324,-0.373243761060364,
-1.69769003172132));
#34377=CARTESIAN_POINT('Ctrl Pts',(0.244262842368623,-0.335108247315849,
-1.68958170688653));
#34378=CARTESIAN_POINT('Ctrl Pts',(0.283214707341173,-0.303141259068212,
-1.68332504372461));
#34379=CARTESIAN_POINT('Ctrl Pts',(0.341837165343982,-0.236152929235937,
-1.67246562047521));
#34380=CARTESIAN_POINT('Ctrl Pts',(0.368536561654407,-0.192480977588835,
-1.66658649961961));
#34381=CARTESIAN_POINT('Ctrl Pts',(0.394174530911059,-0.123823518623745,
-1.66063136041479));
#34382=CARTESIAN_POINT('Ctrl Pts',(0.400393769631748,-0.101649918886749,
-1.65912839404491));
#34383=CARTESIAN_POINT('Ctrl Pts',(0.404717578595296,-0.0793800000000001,
-1.65807299932179));
#34384=CARTESIAN_POINT('',(0.886256117232623,-0.07938,-1.45861320581289));
#34385=CARTESIAN_POINT('Origin',(0.,-0.07938,0.));
#34386=CARTESIAN_POINT('',(1.45861320581289,-0.07938,-0.886256117232623));
#34387=CARTESIAN_POINT('Ctrl Pts',(0.886256117232623,-0.0793800000000001,
-1.45861320581289));
#34388=CARTESIAN_POINT('Ctrl Pts',(0.890059788636852,-0.101649918886749,
-1.45630208793976));
#34389=CARTESIAN_POINT('Ctrl Pts',(0.895520212222106,-0.123823518623745,
-1.45296717977858));
#34390=CARTESIAN_POINT('Ctrl Pts',(0.917859913453974,-0.192480977588835,
-1.43904931717599));
#34391=CARTESIAN_POINT('Ctrl Pts',(0.940896403863072,-0.236152929235937,
-1.4243271592157));
#34392=CARTESIAN_POINT('Ctrl Pts',(0.990027513266106,-0.303141259068211,
-1.39055359345152));
#34393=CARTESIAN_POINT('Ctrl Pts',(1.02199477007745,-0.335108247315849,
-1.36743459453896));
#34394=CARTESIAN_POINT('Ctrl Pts',(1.07446535104584,-0.373243761060364,
-1.32643091652006));
#34395=CARTESIAN_POINT('Ctrl Pts',(1.10126842659597,-0.387888272594439,
-1.30441816675528));
#34396=CARTESIAN_POINT('Ctrl Pts',(1.15530234155453,-0.407041111792943,
-1.25681160160691));
#34397=CARTESIAN_POINT('Ctrl Pts',(1.18251418313119,-0.411552957311693,
-1.23119764287622));
#34398=CARTESIAN_POINT('Ctrl Pts',(1.23119764287622,-0.411552957311693,
-1.18251418313119));
#34399=CARTESIAN_POINT('Ctrl Pts',(1.25681160160691,-0.407041111792943,
-1.15530234155453));
#34400=CARTESIAN_POINT('Ctrl Pts',(1.30441816675528,-0.387888272594439,
-1.10126842659597));
#34401=CARTESIAN_POINT('Ctrl Pts',(1.32643091652006,-0.373243761060364,
-1.07446535104584));
#34402=CARTESIAN_POINT('Ctrl Pts',(1.36743459453896,-0.335108247315849,
-1.02199477007745));
#34403=CARTESIAN_POINT('Ctrl Pts',(1.39055359345152,-0.303141259068212,
-0.990027513266105));
#34404=CARTESIAN_POINT('Ctrl Pts',(1.4243271592157,-0.236152929235937,-0.940896403863071));
#34405=CARTESIAN_POINT('Ctrl Pts',(1.43904931717599,-0.192480977588835,
-0.917859913453974));
#34406=CARTESIAN_POINT('Ctrl Pts',(1.45296717977858,-0.123823518623745,
-0.895520212222106));
#34407=CARTESIAN_POINT('Ctrl Pts',(1.45630208793976,-0.101649918886749,
-0.890059788636852));
#34408=CARTESIAN_POINT('Ctrl Pts',(1.45861320581289,-0.0793800000000001,
-0.886256117232623));
#34409=CARTESIAN_POINT('',(1.65807299932179,-0.07938,-0.404717578595296));
#34410=CARTESIAN_POINT('Origin',(0.,-0.07938,0.));
#34411=CARTESIAN_POINT('',(1.65807299932179,-0.07938,0.404717578595296));
#34412=CARTESIAN_POINT('Ctrl Pts',(1.65807299932179,-0.0793800000000001,
-0.404717578595296));
#34413=CARTESIAN_POINT('Ctrl Pts',(1.65912839404491,-0.101649918886749,
-0.400393769631747));
#34414=CARTESIAN_POINT('Ctrl Pts',(1.66063136041479,-0.123823518623745,
-0.394174530911058));
#34415=CARTESIAN_POINT('Ctrl Pts',(1.66658649961961,-0.192480977588835,
-0.368536561654407));
#34416=CARTESIAN_POINT('Ctrl Pts',(1.67246562047521,-0.236152929235937,
-0.341837165343982));
#34417=CARTESIAN_POINT('Ctrl Pts',(1.68332504372461,-0.303141259068212,
-0.283214707341173));
#34418=CARTESIAN_POINT('Ctrl Pts',(1.68958170688653,-0.335108247315849,
-0.244262842368623));
#34419=CARTESIAN_POINT('Ctrl Pts',(1.69769003172132,-0.373243761060364,
-0.178166559972324));
#34420=CARTESIAN_POINT('Ctrl Pts',(1.70107730356824,-0.387888272594439,
-0.143648558862931));
#34421=CARTESIAN_POINT('Ctrl Pts',(1.70562212620408,-0.407041111792943,
-0.0717778861362655));
#34422=CARTESIAN_POINT('Ctrl Pts',(1.706752,-0.411552957311693,-0.0344244045173312));
#34423=CARTESIAN_POINT('Ctrl Pts',(1.706752,-0.411552957311693,0.0344244045173312));
#34424=CARTESIAN_POINT('Ctrl Pts',(1.70562212620408,-0.407041111792943,
0.0717778861362655));
#34425=CARTESIAN_POINT('Ctrl Pts',(1.70107730356824,-0.387888272594439,
0.143648558862931));
#34426=CARTESIAN_POINT('Ctrl Pts',(1.69769003172132,-0.373243761060364,
0.178166559972324));
#34427=CARTESIAN_POINT('Ctrl Pts',(1.68958170688653,-0.335108247315849,
0.244262842368623));
#34428=CARTESIAN_POINT('Ctrl Pts',(1.68332504372461,-0.303141259068212,
0.283214707341173));
#34429=CARTESIAN_POINT('Ctrl Pts',(1.67246562047521,-0.236152929235937,
0.341837165343982));
#34430=CARTESIAN_POINT('Ctrl Pts',(1.66658649961961,-0.192480977588835,
0.368536561654407));
#34431=CARTESIAN_POINT('Ctrl Pts',(1.66063136041479,-0.123823518623745,
0.394174530911058));
#34432=CARTESIAN_POINT('Ctrl Pts',(1.65912839404491,-0.101649918886749,
0.400393769631747));
#34433=CARTESIAN_POINT('Ctrl Pts',(1.65807299932179,-0.0793800000000001,
0.404717578595296));
#34434=CARTESIAN_POINT('Origin',(0.,-0.07938,0.));
#34435=CARTESIAN_POINT('Origin',(0.,-0.07938,0.));
#34436=CARTESIAN_POINT('',(0.397005914195118,-0.07938,1.59456899932179));
#34437=CARTESIAN_POINT('Origin',(0.,-0.07938,0.));
#34438=CARTESIAN_POINT('Origin',(-3.33066907387547E-16,-0.07938,1.675));
#34439=CARTESIAN_POINT('Origin',(-3.33066907387547E-16,0.,1.675));
#34440=CARTESIAN_POINT('',(-0.397005914195118,-0.07938,1.59456899932179));
#34441=CARTESIAN_POINT('Ctrl Pts',(-0.397005914195119,-0.0793800000000001,
1.59456899932179));
#34442=CARTESIAN_POINT('Ctrl Pts',(-0.3886265584581,-0.123401821157026,
1.59665523941937));
#34443=CARTESIAN_POINT('Ctrl Pts',(-0.373030350867485,-0.166543350814306,
1.60050712143809));
#34444=CARTESIAN_POINT('Ctrl Pts',(-0.333298652394954,-0.237231147975234,
1.60919314384089));
#34445=CARTESIAN_POINT('Ctrl Pts',(-0.311480544243687,-0.266264900654909,
1.61365775139403));
#34446=CARTESIAN_POINT('Ctrl Pts',(-0.261368388670537,-0.317195968905306,
1.62252828437015));
#34447=CARTESIAN_POINT('Ctrl Pts',(-0.233069203882014,-0.33909093068465,
1.62691869420078));
#34448=CARTESIAN_POINT('Ctrl Pts',(-0.174042761838764,-0.373586846396559,
1.63426473152765));
#34449=CARTESIAN_POINT('Ctrl Pts',(-0.14036578147155,-0.388086240756494,
1.63761964365402));
#34450=CARTESIAN_POINT('Ctrl Pts',(-0.0701778381840615,-0.407068917407805,
1.64212536811722));
#34451=CARTESIAN_POINT('Ctrl Pts',(-0.0336652739555918,-0.411552957311693,
1.643248));
#34452=CARTESIAN_POINT('Ctrl Pts',(0.0336652739555913,-0.411552957311693,
1.643248));
#34453=CARTESIAN_POINT('Ctrl Pts',(0.070177838184061,-0.407068917407805,
1.64212536811722));
#34454=CARTESIAN_POINT('Ctrl Pts',(0.140365781471549,-0.388086240756494,
1.63761964365402));
#34455=CARTESIAN_POINT('Ctrl Pts',(0.174042761838763,-0.373586846396559,
1.63426473152765));
#34456=CARTESIAN_POINT('Ctrl Pts',(0.233069203882014,-0.33909093068465,
1.62691869420078));
#34457=CARTESIAN_POINT('Ctrl Pts',(0.261368388670536,-0.317195968905306,
1.62252828437015));
#34458=CARTESIAN_POINT('Ctrl Pts',(0.311480544243686,-0.266264900654908,
1.61365775139403));
#34459=CARTESIAN_POINT('Ctrl Pts',(0.333298652394954,-0.237231147975234,
1.60919314384089));
#34460=CARTESIAN_POINT('Ctrl Pts',(0.373030350867484,-0.166543350814306,
1.60050712143809));
#34461=CARTESIAN_POINT('Ctrl Pts',(0.388626558458099,-0.123401821157026,
1.59665523941937));
#34462=CARTESIAN_POINT('Ctrl Pts',(0.397005914195118,-0.07938,1.59456899932179));
#34463=CARTESIAN_POINT('Origin',(-3.33066907387547E-16,-0.07938,1.675));
#34464=CARTESIAN_POINT('Origin',(0.,-0.07938,0.));
#34465=CARTESIAN_POINT('',(-0.846804978391754,-0.07938,1.40825612658882));
#34466=CARTESIAN_POINT('Origin',(0.,-0.07938,0.));
#34467=CARTESIAN_POINT('Origin',(-1.18440385848747,-0.07938,1.18440385848747));
#34468=CARTESIAN_POINT('Origin',(-1.18440385848747,0.,1.18440385848747));
#34469=CARTESIAN_POINT('',(-1.40825612658882,-0.07938,0.846804978391753));
#34470=CARTESIAN_POINT('Ctrl Pts',(-1.40825612658882,-0.0793800000000001,
0.846804978391753));
#34471=CARTESIAN_POINT('Ctrl Pts',(-1.40380622184538,-0.123401821157026,
0.854205272175555));
#34472=CARTESIAN_POINT('Ctrl Pts',(-1.39550172959303,-0.166543350814306,
0.867957148219442));
#34473=CARTESIAN_POINT('Ctrl Pts',(-1.3735491215176,-0.237231147975235,
0.902193646979983));
#34474=CARTESIAN_POINT('Ctrl Pts',(-1.36127834356734,-0.266264900654909,
0.920778333482565));
#34475=CARTESIAN_POINT('Ctrl Pts',(-1.33211611256184,-0.317195968905306,
0.962485392528369));
#34476=CARTESIAN_POINT('Ctrl Pts',(-1.31521005565926,-0.339090930684651,
0.985600426557816));
#34477=CARTESIAN_POINT('Ctrl Pts',(-1.27866649102984,-0.373586846396559,
1.03253285680459));
#34478=CARTESIAN_POINT('Ctrl Pts',(-1.25722555095714,-0.388086240756494,
1.05871835910697));
#34479=CARTESIAN_POINT('Ctrl Pts',(-1.2107812086231,-0.407068917407805,
1.11153475808518));
#34480=CARTESIAN_POINT('Ctrl Pts',(-1.18575674747573,-0.411552957311693,
1.13814686046673));
#34481=CARTESIAN_POINT('Ctrl Pts',(-1.13814686046673,-0.411552957311693,
1.18575674747573));
#34482=CARTESIAN_POINT('Ctrl Pts',(-1.11153475808518,-0.407068917407805,
1.2107812086231));
#34483=CARTESIAN_POINT('Ctrl Pts',(-1.05871835910697,-0.388086240756494,
1.25722555095714));
#34484=CARTESIAN_POINT('Ctrl Pts',(-1.03253285680459,-0.373586846396559,
1.27866649102984));
#34485=CARTESIAN_POINT('Ctrl Pts',(-0.985600426557816,-0.33909093068465,
1.31521005565926));
#34486=CARTESIAN_POINT('Ctrl Pts',(-0.962485392528369,-0.317195968905306,
1.33211611256184));
#34487=CARTESIAN_POINT('Ctrl Pts',(-0.920778333482565,-0.266264900654908,
1.36127834356734));
#34488=CARTESIAN_POINT('Ctrl Pts',(-0.902193646979983,-0.237231147975234,
1.3735491215176));
#34489=CARTESIAN_POINT('Ctrl Pts',(-0.867957148219442,-0.166543350814306,
1.39550172959303));
#34490=CARTESIAN_POINT('Ctrl Pts',(-0.854205272175555,-0.123401821157026,
1.40380622184538));
#34491=CARTESIAN_POINT('Ctrl Pts',(-0.846804978391753,-0.0793800000000001,
1.40825612658882));
#34492=CARTESIAN_POINT('Origin',(-1.18440385848747,-0.07938,1.18440385848747));
#34493=CARTESIAN_POINT('Origin',(0.,-0.07938,0.));
#34494=CARTESIAN_POINT('',(-1.59456899932179,-0.07938,0.397005914195118));
#34495=CARTESIAN_POINT('Origin',(0.,-0.07938,0.));
#34496=CARTESIAN_POINT('Origin',(-1.675,-0.07938,-2.22044604925031E-16));
#34497=CARTESIAN_POINT('Origin',(-1.675,0.,-2.22044604925031E-16));
#34498=CARTESIAN_POINT('',(-1.59456899932179,-0.07938,-0.397005914195118));
#34499=CARTESIAN_POINT('',(-1.643248,-0.411552957311693,3.47540551556327E-18));
#34500=CARTESIAN_POINT('Ctrl Pts',(-1.59456899932179,-0.0793800000000001,
-0.397005914195119));
#34501=CARTESIAN_POINT('Ctrl Pts',(-1.59665523941937,-0.123401821157026,
-0.388626558458099));
#34502=CARTESIAN_POINT('Ctrl Pts',(-1.60050712143809,-0.166543350814306,
-0.373030350867485));
#34503=CARTESIAN_POINT('Ctrl Pts',(-1.60919314384089,-0.237231147975234,
-0.333298652394954));
#34504=CARTESIAN_POINT('Ctrl Pts',(-1.61365775139403,-0.266264900654909,
-0.311480544243686));
#34505=CARTESIAN_POINT('Ctrl Pts',(-1.62252828437015,-0.317195968905306,
-0.261368388670537));
#34506=CARTESIAN_POINT('Ctrl Pts',(-1.62691869420078,-0.33909093068465,
-0.233069203882014));
#34507=CARTESIAN_POINT('Ctrl Pts',(-1.63426473152765,-0.373586846396559,
-0.174042761838764));
#34508=CARTESIAN_POINT('Ctrl Pts',(-1.63761964365402,-0.388086240756494,
-0.140365781471549));
#34509=CARTESIAN_POINT('Ctrl Pts',(-1.64212536811722,-0.407068917407805,
-0.0701778381840614));
#34510=CARTESIAN_POINT('Ctrl Pts',(-1.643248,-0.411552957311693,-0.0336652739555917));
#34511=CARTESIAN_POINT('Ctrl Pts',(-1.643248,-0.411552957311693,-2.0122792321331E-16));
#34512=CARTESIAN_POINT('Origin',(-1.675,-0.07938,-2.22044604925031E-16));
#34513=CARTESIAN_POINT('Ctrl Pts',(-1.643248,-0.411552957311693,-1.94289029309402E-16));
#34514=CARTESIAN_POINT('Ctrl Pts',(-1.643248,-0.411552957311693,0.0336652739555913));
#34515=CARTESIAN_POINT('Ctrl Pts',(-1.64212536811722,-0.407068917407805,
0.0701778381840609));
#34516=CARTESIAN_POINT('Ctrl Pts',(-1.63761964365402,-0.388086240756494,
0.140365781471549));
#34517=CARTESIAN_POINT('Ctrl Pts',(-1.63426473152765,-0.373586846396559,
0.174042761838763));
#34518=CARTESIAN_POINT('Ctrl Pts',(-1.62691869420078,-0.33909093068465,
0.233069203882014));
#34519=CARTESIAN_POINT('Ctrl Pts',(-1.62252828437015,-0.317195968905306,
0.261368388670536));
#34520=CARTESIAN_POINT('Ctrl Pts',(-1.61365775139403,-0.266264900654909,
0.311480544243686));
#34521=CARTESIAN_POINT('Ctrl Pts',(-1.60919314384089,-0.237231147975235,
0.333298652394954));
#34522=CARTESIAN_POINT('Ctrl Pts',(-1.60050712143809,-0.166543350814306,
0.373030350867484));
#34523=CARTESIAN_POINT('Ctrl Pts',(-1.59665523941937,-0.123401821157026,
0.388626558458099));
#34524=CARTESIAN_POINT('Ctrl Pts',(-1.59456899932179,-0.0793800000000001,
0.397005914195118));
#34525=CARTESIAN_POINT('Origin',(0.,-0.07938,0.));
#34526=CARTESIAN_POINT('',(-1.40825612658882,-0.07938,-0.846804978391753));
#34527=CARTESIAN_POINT('Origin',(0.,-0.07938,0.));
#34528=CARTESIAN_POINT('Origin',(-1.18440385848747,-0.07938,-1.18440385848747));
#34529=CARTESIAN_POINT('Origin',(-1.18440385848747,0.,-1.18440385848747));
#34530=CARTESIAN_POINT('',(-0.846804978391753,-0.07938,-1.40825612658882));
#34531=CARTESIAN_POINT('Ctrl Pts',(-0.846804978391753,-0.0793800000000001,
-1.40825612658882));
#34532=CARTESIAN_POINT('Ctrl Pts',(-0.854205272175555,-0.123401821157026,
-1.40380622184538));
#34533=CARTESIAN_POINT('Ctrl Pts',(-0.867957148219442,-0.166543350814306,
-1.39550172959303));
#34534=CARTESIAN_POINT('Ctrl Pts',(-0.902193646979982,-0.237231147975234,
-1.3735491215176));
#34535=CARTESIAN_POINT('Ctrl Pts',(-0.920778333482564,-0.266264900654908,
-1.36127834356734));
#34536=CARTESIAN_POINT('Ctrl Pts',(-0.962485392528368,-0.317195968905306,
-1.33211611256184));
#34537=CARTESIAN_POINT('Ctrl Pts',(-0.985600426557816,-0.33909093068465,
-1.31521005565926));
#34538=CARTESIAN_POINT('Ctrl Pts',(-1.03253285680459,-0.373586846396559,
-1.27866649102984));
#34539=CARTESIAN_POINT('Ctrl Pts',(-1.05871835910697,-0.388086240756494,
-1.25722555095714));
#34540=CARTESIAN_POINT('Ctrl Pts',(-1.11153475808518,-0.407068917407805,
-1.2107812086231));
#34541=CARTESIAN_POINT('Ctrl Pts',(-1.13814686046673,-0.411552957311693,
-1.18575674747573));
#34542=CARTESIAN_POINT('Ctrl Pts',(-1.18575674747573,-0.411552957311693,
-1.13814686046673));
#34543=CARTESIAN_POINT('Ctrl Pts',(-1.2107812086231,-0.407068917407805,
-1.11153475808518));
#34544=CARTESIAN_POINT('Ctrl Pts',(-1.25722555095714,-0.388086240756494,
-1.05871835910697));
#34545=CARTESIAN_POINT('Ctrl Pts',(-1.27866649102984,-0.373586846396559,
-1.03253285680459));
#34546=CARTESIAN_POINT('Ctrl Pts',(-1.31521005565926,-0.33909093068465,
-0.985600426557816));
#34547=CARTESIAN_POINT('Ctrl Pts',(-1.33211611256184,-0.317195968905306,
-0.962485392528369));
#34548=CARTESIAN_POINT('Ctrl Pts',(-1.36127834356734,-0.266264900654909,
-0.920778333482565));
#34549=CARTESIAN_POINT('Ctrl Pts',(-1.3735491215176,-0.237231147975234,
-0.902193646979983));
#34550=CARTESIAN_POINT('Ctrl Pts',(-1.39550172959303,-0.166543350814306,
-0.867957148219442));
#34551=CARTESIAN_POINT('Ctrl Pts',(-1.40380622184538,-0.123401821157026,
-0.854205272175555));
#34552=CARTESIAN_POINT('Ctrl Pts',(-1.40825612658882,-0.07938,-0.846804978391753));
#34553=CARTESIAN_POINT('Origin',(-1.18440385848747,-0.07938,-1.18440385848747));
#34554=CARTESIAN_POINT('Origin',(0.,-0.07938,0.));
#34555=CARTESIAN_POINT('',(-0.397005914195118,-0.07938,-1.59456899932179));
#34556=CARTESIAN_POINT('Origin',(0.,-0.07938,0.));
#34557=CARTESIAN_POINT('Origin',(1.11022302462516E-16,-0.07938,-1.675));
#34558=CARTESIAN_POINT('Origin',(1.11022302462516E-16,0.,-1.675));
#34559=CARTESIAN_POINT('',(0.397005914195118,-0.07938,-1.59456899932179));
#34560=CARTESIAN_POINT('Ctrl Pts',(0.397005914195119,-0.0793800000000001,
-1.59456899932179));
#34561=CARTESIAN_POINT('Ctrl Pts',(0.388626558458099,-0.123401821157026,
-1.59665523941937));
#34562=CARTESIAN_POINT('Ctrl Pts',(0.373030350867485,-0.166543350814306,
-1.60050712143809));
#34563=CARTESIAN_POINT('Ctrl Pts',(0.333298652394954,-0.237231147975234,
-1.60919314384089));
#34564=CARTESIAN_POINT('Ctrl Pts',(0.311480544243686,-0.266264900654909,
-1.61365775139403));
#34565=CARTESIAN_POINT('Ctrl Pts',(0.261368388670537,-0.317195968905306,
-1.62252828437015));
#34566=CARTESIAN_POINT('Ctrl Pts',(0.233069203882014,-0.33909093068465,
-1.62691869420078));
#34567=CARTESIAN_POINT('Ctrl Pts',(0.174042761838763,-0.373586846396559,
-1.63426473152765));
#34568=CARTESIAN_POINT('Ctrl Pts',(0.140365781471549,-0.388086240756494,
-1.63761964365402));
#34569=CARTESIAN_POINT('Ctrl Pts',(0.0701778381840612,-0.407068917407805,
-1.64212536811722));
#34570=CARTESIAN_POINT('Ctrl Pts',(0.0336652739555916,-0.411552957311693,
-1.643248));
#34571=CARTESIAN_POINT('Ctrl Pts',(-0.0336652739555915,-0.411552957311693,
-1.643248));
#34572=CARTESIAN_POINT('Ctrl Pts',(-0.0701778381840612,-0.407068917407805,
-1.64212536811722));
#34573=CARTESIAN_POINT('Ctrl Pts',(-0.140365781471549,-0.388086240756494,
-1.63761964365402));
#34574=CARTESIAN_POINT('Ctrl Pts',(-0.174042761838764,-0.373586846396559,
-1.63426473152765));
#34575=CARTESIAN_POINT('Ctrl Pts',(-0.233069203882014,-0.33909093068465,
-1.62691869420078));
#34576=CARTESIAN_POINT('Ctrl Pts',(-0.261368388670536,-0.317195968905306,
-1.62252828437015));
#34577=CARTESIAN_POINT('Ctrl Pts',(-0.311480544243686,-0.266264900654908,
-1.61365775139403));
#34578=CARTESIAN_POINT('Ctrl Pts',(-0.333298652394954,-0.237231147975234,
-1.60919314384089));
#34579=CARTESIAN_POINT('Ctrl Pts',(-0.373030350867485,-0.166543350814306,
-1.60050712143809));
#34580=CARTESIAN_POINT('Ctrl Pts',(-0.388626558458099,-0.123401821157026,
-1.59665523941937));
#34581=CARTESIAN_POINT('Ctrl Pts',(-0.397005914195118,-0.07938,-1.59456899932179));
#34582=CARTESIAN_POINT('Origin',(1.11022302462516E-16,-0.07938,-1.675));
#34583=CARTESIAN_POINT('Origin',(0.,-0.07938,0.));
#34584=CARTESIAN_POINT('',(0.846804978391753,-0.07938,-1.40825612658882));
#34585=CARTESIAN_POINT('Origin',(0.,-0.07938,0.));
#34586=CARTESIAN_POINT('Origin',(1.18440385848747,-0.07938,-1.18440385848747));
#34587=CARTESIAN_POINT('Origin',(1.18440385848747,0.,-1.18440385848747));
#34588=CARTESIAN_POINT('',(1.40825612658882,-0.07938,-0.846804978391753));
#34589=CARTESIAN_POINT('Ctrl Pts',(1.40825612658882,-0.0793800000000001,
-0.846804978391753));
#34590=CARTESIAN_POINT('Ctrl Pts',(1.40380622184538,-0.123401821157026,
-0.854205272175555));
#34591=CARTESIAN_POINT('Ctrl Pts',(1.39550172959303,-0.166543350814306,
-0.867957148219442));
#34592=CARTESIAN_POINT('Ctrl Pts',(1.3735491215176,-0.237231147975234,-0.902193646979983));
#34593=CARTESIAN_POINT('Ctrl Pts',(1.36127834356734,-0.266264900654908,
-0.920778333482565));
#34594=CARTESIAN_POINT('Ctrl Pts',(1.33211611256184,-0.317195968905306,
-0.962485392528369));
#34595=CARTESIAN_POINT('Ctrl Pts',(1.31521005565926,-0.33909093068465,-0.985600426557816));
#34596=CARTESIAN_POINT('Ctrl Pts',(1.27866649102984,-0.373586846396559,
-1.03253285680459));
#34597=CARTESIAN_POINT('Ctrl Pts',(1.25722555095714,-0.388086240756494,
-1.05871835910697));
#34598=CARTESIAN_POINT('Ctrl Pts',(1.2107812086231,-0.407068917407805,-1.11153475808518));
#34599=CARTESIAN_POINT('Ctrl Pts',(1.18575674747573,-0.411552957311693,
-1.13814686046673));
#34600=CARTESIAN_POINT('Ctrl Pts',(1.13814686046673,-0.411552957311693,
-1.18575674747573));
#34601=CARTESIAN_POINT('Ctrl Pts',(1.11153475808518,-0.407068917407805,
-1.2107812086231));
#34602=CARTESIAN_POINT('Ctrl Pts',(1.05871835910697,-0.388086240756494,
-1.25722555095714));
#34603=CARTESIAN_POINT('Ctrl Pts',(1.03253285680459,-0.373586846396559,
-1.27866649102984));
#34604=CARTESIAN_POINT('Ctrl Pts',(0.985600426557816,-0.33909093068465,
-1.31521005565926));
#34605=CARTESIAN_POINT('Ctrl Pts',(0.962485392528369,-0.317195968905306,
-1.33211611256184));
#34606=CARTESIAN_POINT('Ctrl Pts',(0.920778333482565,-0.266264900654909,
-1.36127834356734));
#34607=CARTESIAN_POINT('Ctrl Pts',(0.902193646979983,-0.237231147975234,
-1.3735491215176));
#34608=CARTESIAN_POINT('Ctrl Pts',(0.867957148219442,-0.166543350814306,
-1.39550172959303));
#34609=CARTESIAN_POINT('Ctrl Pts',(0.854205272175555,-0.123401821157026,
-1.40380622184538));
#34610=CARTESIAN_POINT('Ctrl Pts',(0.846804978391753,-0.0793800000000001,
-1.40825612658882));
#34611=CARTESIAN_POINT('Origin',(1.18440385848747,-0.07938,-1.18440385848747));
#34612=CARTESIAN_POINT('Origin',(0.,-0.27783,0.));
#34613=CARTESIAN_POINT('',(-1.643248,-0.47628,2.01239840340529E-16));
#34614=CARTESIAN_POINT('Origin',(0.,-0.47628,0.));
#34615=CARTESIAN_POINT('',(-1.643248,-0.27783,2.01239840340529E-16));
#34616=CARTESIAN_POINT('',(1.59456899932179,-0.07938,0.397005914195118));
#34617=CARTESIAN_POINT('Origin',(0.,-0.07938,0.));
#34618=CARTESIAN_POINT('',(1.59456899932179,-0.07938,-0.397005914195118));
#34619=CARTESIAN_POINT('Ctrl Pts',(1.59456899932179,-0.0793800000000001,
0.397005914195118));
#34620=CARTESIAN_POINT('Ctrl Pts',(1.59665523941937,-0.123401821157026,
0.388626558458099));
#34621=CARTESIAN_POINT('Ctrl Pts',(1.60050712143809,-0.166543350814306,
0.373030350867485));
#34622=CARTESIAN_POINT('Ctrl Pts',(1.60919314384089,-0.237231147975234,
0.333298652394954));
#34623=CARTESIAN_POINT('Ctrl Pts',(1.61365775139403,-0.266264900654909,
0.311480544243686));
#34624=CARTESIAN_POINT('Ctrl Pts',(1.62252828437015,-0.317195968905306,
0.261368388670537));
#34625=CARTESIAN_POINT('Ctrl Pts',(1.62691869420078,-0.33909093068465,0.233069203882014));
#34626=CARTESIAN_POINT('Ctrl Pts',(1.63426473152765,-0.373586846396559,
0.174042761838764));
#34627=CARTESIAN_POINT('Ctrl Pts',(1.63761964365402,-0.388086240756494,
0.140365781471549));
#34628=CARTESIAN_POINT('Ctrl Pts',(1.64212536811722,-0.407068917407805,
0.0701778381840612));
#34629=CARTESIAN_POINT('Ctrl Pts',(1.643248,-0.411552957311693,0.0336652739555916));
#34630=CARTESIAN_POINT('Ctrl Pts',(1.643248,-0.411552957311693,-0.0336652739555916));
#34631=CARTESIAN_POINT('Ctrl Pts',(1.64212536811722,-0.407068917407805,
-0.0701778381840612));
#34632=CARTESIAN_POINT('Ctrl Pts',(1.63761964365402,-0.388086240756494,
-0.140365781471549));
#34633=CARTESIAN_POINT('Ctrl Pts',(1.63426473152765,-0.373586846396559,
-0.174042761838764));
#34634=CARTESIAN_POINT('Ctrl Pts',(1.62691869420078,-0.33909093068465,-0.233069203882014));
#34635=CARTESIAN_POINT('Ctrl Pts',(1.62252828437015,-0.317195968905306,
-0.261368388670537));
#34636=CARTESIAN_POINT('Ctrl Pts',(1.61365775139403,-0.266264900654909,
-0.311480544243686));
#34637=CARTESIAN_POINT('Ctrl Pts',(1.60919314384089,-0.237231147975234,
-0.333298652394954));
#34638=CARTESIAN_POINT('Ctrl Pts',(1.60050712143809,-0.166543350814306,
-0.373030350867485));
#34639=CARTESIAN_POINT('Ctrl Pts',(1.59665523941937,-0.123401821157026,
-0.388626558458099));
#34640=CARTESIAN_POINT('Ctrl Pts',(1.59456899932179,-0.07938,-0.397005914195118));
#34641=CARTESIAN_POINT('Origin',(0.,-0.07938,0.));
#34642=CARTESIAN_POINT('Origin',(0.,-0.07938,0.));
#34643=CARTESIAN_POINT('Origin',(1.675,-0.07938,0.));
#34644=CARTESIAN_POINT('Origin',(1.675,0.,0.));
#34645=CARTESIAN_POINT('Origin',(1.675,-0.07938,0.));
#34646=CARTESIAN_POINT('Origin',(0.,-0.47628,0.));
#34647=CARTESIAN_POINT('Origin',(0.,-0.07938,0.));
#34648=CARTESIAN_POINT('',(0.,0.,0.));
#34649=CARTESIAN_POINT('Origin',(1.70469,0.695,0.));
#34650=CARTESIAN_POINT('',(-1.70469,0.695,-2.0876431520385E-16));
#34651=CARTESIAN_POINT('Origin',(0.,0.695,0.));
#34652=CARTESIAN_POINT('',(-1.65031,0.695,-2.02104685910087E-16));
#34653=CARTESIAN_POINT('Origin',(0.,0.695,0.));
#34654=CARTESIAN_POINT('Origin',(0.,0.6575,0.));
#34655=CARTESIAN_POINT('',(-1.70469,0.62,-2.0876431520385E-16));
#34656=CARTESIAN_POINT('Origin',(0.,0.62,0.));
#34657=CARTESIAN_POINT('',(-1.70469,0.6575,-2.0876431520385E-16));
#34658=CARTESIAN_POINT('Origin',(1.65031,0.62,0.));
#34659=CARTESIAN_POINT('',(-1.65031,0.62,-2.02104685910087E-16));
#34660=CARTESIAN_POINT('Origin',(0.,0.62,0.));
#34661=CARTESIAN_POINT('Origin',(0.,0.6575,0.));
#34662=CARTESIAN_POINT('',(-1.65031,0.6575,-2.02104685910087E-16));
#34663=CARTESIAN_POINT('Origin',(1.70469,-0.62,0.));
#34664=CARTESIAN_POINT('',(-1.70469,-0.62,-2.0876431520385E-16));
#34665=CARTESIAN_POINT('Origin',(0.,-0.62,0.));
#34666=CARTESIAN_POINT('',(-1.65031,-0.62,-2.02104685910087E-16));
#34667=CARTESIAN_POINT('Origin',(0.,-0.62,0.));
#34668=CARTESIAN_POINT('Origin',(0.,-0.6575,0.));
#34669=CARTESIAN_POINT('',(-1.70469,-0.695,-2.0876431520385E-16));
#34670=CARTESIAN_POINT('Origin',(0.,-0.695,0.));
#34671=CARTESIAN_POINT('',(-1.70469,-0.6575,-2.0876431520385E-16));
#34672=CARTESIAN_POINT('Origin',(1.65031,-0.695,0.));
#34673=CARTESIAN_POINT('',(-1.65031,-0.695,-2.02104685910087E-16));
#34674=CARTESIAN_POINT('Origin',(0.,-0.695,0.));
#34675=CARTESIAN_POINT('Origin',(0.,-0.6575,0.));
#34676=CARTESIAN_POINT('',(-1.65031,-0.6575,-2.02104685910087E-16));
#34677=CARTESIAN_POINT('',(0.,0.,0.));
#34678=CARTESIAN_POINT('',(0.,0.,0.));
#34679=CARTESIAN_POINT('',(0.,0.,0.));
#34680=CARTESIAN_POINT('',(0.,0.,0.));
#34681=CARTESIAN_POINT('',(0.,0.,0.));
#34682=CARTESIAN_POINT('',(0.,0.,0.));
#34683=CARTESIAN_POINT('',(0.,0.,0.));
#34684=CARTESIAN_POINT('Origin',(15.,-7.9,5.1));
#34685=CARTESIAN_POINT('',(14.725,-7.9,5.2));
#34686=CARTESIAN_POINT('Origin',(15.,-7.9,5.2));
#34687=CARTESIAN_POINT('',(14.725,-7.9,6.));
#34688=CARTESIAN_POINT('',(14.725,-7.9,5.1));
#34689=CARTESIAN_POINT('Origin',(15.,-7.9,6.));
#34690=CARTESIAN_POINT('Origin',(12.,-4.1,5.1));
#34691=CARTESIAN_POINT('',(11.725,-4.1,5.2));
#34692=CARTESIAN_POINT('Origin',(12.,-4.1,5.2));
#34693=CARTESIAN_POINT('',(11.725,-4.1,6.));
#34694=CARTESIAN_POINT('',(11.725,-4.1,5.1));
#34695=CARTESIAN_POINT('Origin',(12.,-4.1,6.));
#34696=CARTESIAN_POINT('Origin',(12.,-7.9,5.1));
#34697=CARTESIAN_POINT('',(11.725,-7.9,5.2));
#34698=CARTESIAN_POINT('Origin',(12.,-7.9,5.2));
#34699=CARTESIAN_POINT('',(11.725,-7.9,6.));
#34700=CARTESIAN_POINT('',(11.725,-7.9,5.1));
#34701=CARTESIAN_POINT('Origin',(12.,-7.9,6.));
#34702=CARTESIAN_POINT('Origin',(15.,-4.1,5.1));
#34703=CARTESIAN_POINT('',(14.725,-4.1,5.2));
#34704=CARTESIAN_POINT('Origin',(15.,-4.1,5.2));
#34705=CARTESIAN_POINT('',(14.725,-4.1,6.));
#34706=CARTESIAN_POINT('',(14.725,-4.1,5.1));
#34707=CARTESIAN_POINT('Origin',(15.,-4.1,6.));
#34708=CARTESIAN_POINT('Origin',(16.6,-3.65,5.2));
#34709=CARTESIAN_POINT('',(16.6,-3.65,5.2));
#34710=CARTESIAN_POINT('',(10.4,-3.65,5.2));
#34711=CARTESIAN_POINT('',(16.6,-3.65,5.2));
#34712=CARTESIAN_POINT('',(10.4,-3.65,6.));
#34713=CARTESIAN_POINT('',(10.4,-3.65,5.2));
#34714=CARTESIAN_POINT('',(16.6,-3.65,6.));
#34715=CARTESIAN_POINT('',(16.6,-3.65,6.));
#34716=CARTESIAN_POINT('',(16.6,-3.65,5.2));
#34717=CARTESIAN_POINT('Origin',(16.6,-8.35,5.2));
#34718=CARTESIAN_POINT('',(16.6,-8.35,5.2));
#34719=CARTESIAN_POINT('',(16.6,-8.35,5.2));
#34720=CARTESIAN_POINT('',(16.6,-8.35,6.));
#34721=CARTESIAN_POINT('',(16.6,-8.35,6.));
#34722=CARTESIAN_POINT('',(16.6,-8.35,5.2));
#34723=CARTESIAN_POINT('Origin',(10.4,-8.35,5.2));
#34724=CARTESIAN_POINT('',(10.4,-8.35,5.2));
#34725=CARTESIAN_POINT('',(10.4,-8.35,5.2));
#34726=CARTESIAN_POINT('',(10.4,-8.35,6.));
#34727=CARTESIAN_POINT('',(10.4,-8.35,6.));
#34728=CARTESIAN_POINT('',(10.4,-8.35,5.2));
#34729=CARTESIAN_POINT('Origin',(10.4,-3.65,5.2));
#34730=CARTESIAN_POINT('',(10.4,-3.65,5.2));
#34731=CARTESIAN_POINT('',(10.4,-3.65,6.));
#34732=CARTESIAN_POINT('Origin',(13.5,-6.,6.));
#34733=CARTESIAN_POINT('Origin',(13.5,-6.,5.2));
#34734=CARTESIAN_POINT('',(0.,0.,0.));
#34735=CARTESIAN_POINT('Origin',(16.2,-9.,5.9));
#34736=CARTESIAN_POINT('',(15.99,-9.,6.));
#34737=CARTESIAN_POINT('Origin',(16.2,-9.,6.));
#34738=CARTESIAN_POINT('',(15.99,-9.,7.2));
#34739=CARTESIAN_POINT('',(15.99,-9.,5.9));
#34740=CARTESIAN_POINT('Origin',(16.2,-9.,7.2));
#34741=CARTESIAN_POINT('Origin',(10.8,1.,5.9));
#34742=CARTESIAN_POINT('',(10.59,1.,6.));
#34743=CARTESIAN_POINT('Origin',(10.8,1.,6.));
#34744=CARTESIAN_POINT('',(10.59,1.,7.2));
#34745=CARTESIAN_POINT('',(10.59,1.,5.9));
#34746=CARTESIAN_POINT('Origin',(10.8,1.,7.2));
#34747=CARTESIAN_POINT('Origin',(10.8,-9.,5.9));
#34748=CARTESIAN_POINT('',(10.59,-9.,6.));
#34749=CARTESIAN_POINT('Origin',(10.8,-9.,6.));
#34750=CARTESIAN_POINT('',(10.59,-9.,7.2));
#34751=CARTESIAN_POINT('',(10.59,-9.,5.9));
#34752=CARTESIAN_POINT('Origin',(10.8,-9.,7.2));
#34753=CARTESIAN_POINT('Origin',(16.2,1.,5.9));
#34754=CARTESIAN_POINT('',(15.99,1.,6.));
#34755=CARTESIAN_POINT('Origin',(16.2,1.,6.));
#34756=CARTESIAN_POINT('',(15.99,1.,7.2));
#34757=CARTESIAN_POINT('',(15.99,1.,5.9));
#34758=CARTESIAN_POINT('Origin',(16.2,1.,7.2));
#34759=CARTESIAN_POINT('Origin',(14.,-1.5,5.9));
#34760=CARTESIAN_POINT('',(13.725,-1.5,6.));
#34761=CARTESIAN_POINT('Origin',(14.,-1.5,6.));
#34762=CARTESIAN_POINT('',(13.725,-1.5,7.2));
#34763=CARTESIAN_POINT('',(13.725,-1.5,5.9));
#34764=CARTESIAN_POINT('Origin',(14.,-1.5,7.2));
#34765=CARTESIAN_POINT('Origin',(12.5,1.5,5.9));
#34766=CARTESIAN_POINT('',(12.225,1.5,6.));
#34767=CARTESIAN_POINT('Origin',(12.5,1.5,6.));
#34768=CARTESIAN_POINT('',(12.225,1.5,7.2));
#34769=CARTESIAN_POINT('',(12.225,1.5,5.9));
#34770=CARTESIAN_POINT('Origin',(12.5,1.5,7.2));
#34771=CARTESIAN_POINT('Origin',(12.5,-1.5,5.9));
#34772=CARTESIAN_POINT('',(12.225,-1.5,6.));
#34773=CARTESIAN_POINT('Origin',(12.5,-1.5,6.));
#34774=CARTESIAN_POINT('',(12.225,-1.5,7.2));
#34775=CARTESIAN_POINT('',(12.225,-1.5,5.9));
#34776=CARTESIAN_POINT('Origin',(12.5,-1.5,7.2));
#34777=CARTESIAN_POINT('Origin',(14.,1.5,5.9));
#34778=CARTESIAN_POINT('',(13.725,1.5,6.));
#34779=CARTESIAN_POINT('Origin',(14.,1.5,6.));
#34780=CARTESIAN_POINT('',(13.725,1.5,7.2));
#34781=CARTESIAN_POINT('',(13.725,1.5,5.9));
#34782=CARTESIAN_POINT('Origin',(14.,1.5,7.2));
#34783=CARTESIAN_POINT('Origin',(15.,-7.9,5.1));
#34784=CARTESIAN_POINT('',(14.725,-7.9,6.));
#34785=CARTESIAN_POINT('Origin',(15.,-7.9,6.));
#34786=CARTESIAN_POINT('',(14.725,-7.9,7.2));
#34787=CARTESIAN_POINT('',(14.725,-7.9,5.1));
#34788=CARTESIAN_POINT('Origin',(15.,-7.9,7.2));
#34789=CARTESIAN_POINT('Origin',(12.,-4.1,5.1));
#34790=CARTESIAN_POINT('',(11.725,-4.1,6.));
#34791=CARTESIAN_POINT('Origin',(12.,-4.1,6.));
#34792=CARTESIAN_POINT('',(11.725,-4.1,7.2));
#34793=CARTESIAN_POINT('',(11.725,-4.1,5.1));
#34794=CARTESIAN_POINT('Origin',(12.,-4.1,7.2));
#34795=CARTESIAN_POINT('Origin',(12.,-7.9,5.1));
#34796=CARTESIAN_POINT('',(11.725,-7.9,6.));
#34797=CARTESIAN_POINT('Origin',(12.,-7.9,6.));
#34798=CARTESIAN_POINT('',(11.725,-7.9,7.2));
#34799=CARTESIAN_POINT('',(11.725,-7.9,5.1));
#34800=CARTESIAN_POINT('Origin',(12.,-7.9,7.2));
#34801=CARTESIAN_POINT('Origin',(15.,-4.1,5.1));
#34802=CARTESIAN_POINT('',(14.725,-4.1,6.));
#34803=CARTESIAN_POINT('Origin',(15.,-4.1,6.));
#34804=CARTESIAN_POINT('',(14.725,-4.1,7.2));
#34805=CARTESIAN_POINT('',(14.725,-4.1,5.1));
#34806=CARTESIAN_POINT('Origin',(15.,-4.1,7.2));
#34807=CARTESIAN_POINT('Origin',(17.,2.5,6.));
#34808=CARTESIAN_POINT('',(17.,2.5,6.));
#34809=CARTESIAN_POINT('',(10.,2.5,6.));
#34810=CARTESIAN_POINT('',(17.,2.5,6.));
#34811=CARTESIAN_POINT('',(10.,2.5,7.2));
#34812=CARTESIAN_POINT('',(10.,2.5,6.));
#34813=CARTESIAN_POINT('',(17.,2.5,7.2));
#34814=CARTESIAN_POINT('',(17.,2.5,7.2));
#34815=CARTESIAN_POINT('',(17.,2.5,6.));
#34816=CARTESIAN_POINT('Origin',(17.,-10.,6.));
#34817=CARTESIAN_POINT('',(17.,-10.,6.));
#34818=CARTESIAN_POINT('',(17.,-10.,6.));
#34819=CARTESIAN_POINT('',(17.,-10.,7.2));
#34820=CARTESIAN_POINT('',(17.,-10.,7.2));
#34821=CARTESIAN_POINT('',(17.,-10.,6.));
#34822=CARTESIAN_POINT('Origin',(10.,-10.,6.));
#34823=CARTESIAN_POINT('',(10.,-10.,6.));
#34824=CARTESIAN_POINT('',(10.,-10.,6.));
#34825=CARTESIAN_POINT('',(10.,-10.,7.2));
#34826=CARTESIAN_POINT('',(10.,-10.,7.2));
#34827=CARTESIAN_POINT('',(10.,-10.,6.));
#34828=CARTESIAN_POINT('Origin',(10.,2.5,6.));
#34829=CARTESIAN_POINT('',(10.,2.5,6.));
#34830=CARTESIAN_POINT('',(10.,2.5,7.2));
#34831=CARTESIAN_POINT('Origin',(13.5,-3.75,7.2));
#34832=CARTESIAN_POINT('Origin',(13.5,-3.75,6.));
#34833=CARTESIAN_POINT('',(0.,0.,0.));
#34834=CARTESIAN_POINT('Origin',(14.,-1.5,5.1));
#34835=CARTESIAN_POINT('',(13.79,-1.5,5.1));
#34836=CARTESIAN_POINT('Origin',(14.,-1.5,5.1));
#34837=CARTESIAN_POINT('',(13.79,-1.5,6.));
#34838=CARTESIAN_POINT('',(13.79,-1.5,5.1));
#34839=CARTESIAN_POINT('Origin',(14.,-1.5,6.));
#34840=CARTESIAN_POINT('Origin',(14.,-1.5,5.1));
#34841=CARTESIAN_POINT('Origin',(12.5,1.5,5.1));
#34842=CARTESIAN_POINT('',(12.29,1.5,5.1));
#34843=CARTESIAN_POINT('Origin',(12.5,1.5,5.1));
#34844=CARTESIAN_POINT('',(12.29,1.5,6.));
#34845=CARTESIAN_POINT('',(12.29,1.5,5.1));
#34846=CARTESIAN_POINT('Origin',(12.5,1.5,6.));
#34847=CARTESIAN_POINT('Origin',(12.5,1.5,5.1));
#34848=CARTESIAN_POINT('Origin',(12.5,-1.5,5.1));
#34849=CARTESIAN_POINT('',(12.29,-1.5,5.1));
#34850=CARTESIAN_POINT('Origin',(12.5,-1.5,5.1));
#34851=CARTESIAN_POINT('',(12.29,-1.5,6.));
#34852=CARTESIAN_POINT('',(12.29,-1.5,5.1));
#34853=CARTESIAN_POINT('Origin',(12.5,-1.5,6.));
#34854=CARTESIAN_POINT('Origin',(12.5,-1.5,5.1));
#34855=CARTESIAN_POINT('Origin',(14.,1.5,5.1));
#34856=CARTESIAN_POINT('',(13.79,1.5,5.1));
#34857=CARTESIAN_POINT('Origin',(14.,1.5,5.1));
#34858=CARTESIAN_POINT('',(13.79,1.5,6.));
#34859=CARTESIAN_POINT('',(13.79,1.5,5.1));
#34860=CARTESIAN_POINT('Origin',(14.,1.5,6.));
#34861=CARTESIAN_POINT('Origin',(14.,1.5,5.1));
#34862=CARTESIAN_POINT('Origin',(12.9,-1.5,4.));
#34863=CARTESIAN_POINT('',(12.9,-1.5,4.165));
#34864=CARTESIAN_POINT('Origin',(12.9,-1.5,4.));
#34865=CARTESIAN_POINT('',(14.5,-1.5,4.165));
#34866=CARTESIAN_POINT('',(12.9,-1.5,4.165));
#34867=CARTESIAN_POINT('Origin',(14.5,-1.5,4.));
#34868=CARTESIAN_POINT('Origin',(12.9,-1.5,4.));
#34869=CARTESIAN_POINT('Origin',(12.9,1.5,4.));
#34870=CARTESIAN_POINT('',(12.9,1.5,4.165));
#34871=CARTESIAN_POINT('Origin',(12.9,1.5,4.));
#34872=CARTESIAN_POINT('',(14.5,1.5,4.165));
#34873=CARTESIAN_POINT('',(12.9,1.5,4.165));
#34874=CARTESIAN_POINT('Origin',(14.5,1.5,4.));
#34875=CARTESIAN_POINT('Origin',(12.9,1.5,4.));
#34876=CARTESIAN_POINT('Origin',(12.9,0.,5.5));
#34877=CARTESIAN_POINT('',(12.9,-2.02066721859313E-17,5.665));
#34878=CARTESIAN_POINT('Origin',(12.9,0.,5.5));
#34879=CARTESIAN_POINT('',(14.5,2.02066721859313E-17,5.665));
#34880=CARTESIAN_POINT('',(12.9,-2.02066721859313E-17,5.665));
#34881=CARTESIAN_POINT('Origin',(14.5,0.,5.5));
#34882=CARTESIAN_POINT('Origin',(12.9,0.,5.5));
#34883=CARTESIAN_POINT('Origin',(11.9,0.,4.));
#34884=CARTESIAN_POINT('',(12.,-1.35935794705356E-16,5.11));
#34885=CARTESIAN_POINT('Origin',(12.,0.,4.));
#34886=CARTESIAN_POINT('',(14.5,1.35935794705356E-16,5.11));
#34887=CARTESIAN_POINT('',(11.9,-1.35935794705356E-16,5.11));
#34888=CARTESIAN_POINT('Origin',(14.5,0.,4.));
#34889=CARTESIAN_POINT('Origin',(14.5,2.2,2.5));
#34890=CARTESIAN_POINT('',(14.5,2.2,2.5));
#34891=CARTESIAN_POINT('',(12.,2.2,2.5));
#34892=CARTESIAN_POINT('',(14.5,2.2,2.5));
#34893=CARTESIAN_POINT('',(12.,2.2,6.));
#34894=CARTESIAN_POINT('',(12.,2.2,2.5));
#34895=CARTESIAN_POINT('',(14.5,2.2,6.));
#34896=CARTESIAN_POINT('',(14.5,2.2,6.));
#34897=CARTESIAN_POINT('',(14.5,2.2,2.5));
#34898=CARTESIAN_POINT('Origin',(14.5,-2.2,2.5));
#34899=CARTESIAN_POINT('',(14.5,-2.2,2.5));
#34900=CARTESIAN_POINT('',(14.5,-2.2,2.5));
#34901=CARTESIAN_POINT('',(14.5,-2.2,6.));
#34902=CARTESIAN_POINT('',(14.5,-2.2,6.));
#34903=CARTESIAN_POINT('',(14.5,-2.2,2.5));
#34904=CARTESIAN_POINT('Origin',(12.,-2.2,2.5));
#34905=CARTESIAN_POINT('',(12.,-2.2,2.5));
#34906=CARTESIAN_POINT('',(12.,-2.2,2.5));
#34907=CARTESIAN_POINT('',(12.,-2.2,6.));
#34908=CARTESIAN_POINT('',(12.,-2.2,6.));
#34909=CARTESIAN_POINT('',(12.,-2.2,2.5));
#34910=CARTESIAN_POINT('Origin',(12.,2.2,2.5));
#34911=CARTESIAN_POINT('',(12.,2.2,2.5));
#34912=CARTESIAN_POINT('',(12.,2.2,6.));
#34913=CARTESIAN_POINT('Origin',(13.25,0.,6.));
#34914=CARTESIAN_POINT('Origin',(13.25,0.,2.5));
#34915=CARTESIAN_POINT('',(0.,0.,0.));
#34916=CARTESIAN_POINT('',(0.,0.,0.));
#34917=CARTESIAN_POINT('Origin',(1.5,-1.9,1.7));
#34918=CARTESIAN_POINT('',(1.56403124237433,-1.7,1.7));
#34919=CARTESIAN_POINT('',(1.43596875762567,-1.7,1.7));
#34920=CARTESIAN_POINT('',(0.75,-1.7,1.7));
#34921=CARTESIAN_POINT('Origin',(1.5,-1.9,1.7));
#34922=CARTESIAN_POINT('Origin',(1.5,-1.9,1.7));
#34923=CARTESIAN_POINT('',(1.56403124237433,-1.7,1.75));
#34924=CARTESIAN_POINT('',(1.56403124237433,-1.7,1.7));
#34925=CARTESIAN_POINT('',(1.29,-1.9,1.75));
#34926=CARTESIAN_POINT('Origin',(1.5,-1.9,1.75));
#34927=CARTESIAN_POINT('',(1.29,-1.9,2.4));
#34928=CARTESIAN_POINT('',(1.29,-1.9,1.7));
#34929=CARTESIAN_POINT('Origin',(1.5,-1.9,2.4));
#34930=CARTESIAN_POINT('',(1.43596875762567,-1.7,1.75));
#34931=CARTESIAN_POINT('Origin',(1.5,-1.9,1.75));
#34932=CARTESIAN_POINT('',(1.43596875762567,-1.7,1.7));
#34933=CARTESIAN_POINT('Origin',(-1.5,1.9,1.7));
#34934=CARTESIAN_POINT('',(-1.56403124237433,1.7,1.7));
#34935=CARTESIAN_POINT('',(-1.43596875762567,1.7,1.7));
#34936=CARTESIAN_POINT('',(-0.75,1.7,1.7));
#34937=CARTESIAN_POINT('Origin',(-1.5,1.9,1.7));
#34938=CARTESIAN_POINT('Origin',(-1.5,1.9,1.7));
#34939=CARTESIAN_POINT('',(-1.56403124237433,1.7,1.75));
#34940=CARTESIAN_POINT('',(-1.56403124237433,1.7,1.7));
#34941=CARTESIAN_POINT('',(-1.71,1.9,1.75));
#34942=CARTESIAN_POINT('Origin',(-1.5,1.9,1.75));
#34943=CARTESIAN_POINT('',(-1.71,1.9,2.4));
#34944=CARTESIAN_POINT('',(-1.71,1.9,1.7));
#34945=CARTESIAN_POINT('Origin',(-1.5,1.9,2.4));
#34946=CARTESIAN_POINT('',(-1.43596875762567,1.7,1.75));
#34947=CARTESIAN_POINT('Origin',(-1.5,1.9,1.75));
#34948=CARTESIAN_POINT('',(-1.43596875762567,1.7,1.7));
#34949=CARTESIAN_POINT('Origin',(-1.5,-1.9,1.7));
#34950=CARTESIAN_POINT('',(-1.43596875762567,-1.7,1.7));
#34951=CARTESIAN_POINT('',(-1.56403124237433,-1.7,1.7));
#34952=CARTESIAN_POINT('',(-0.75,-1.7,1.7));
#34953=CARTESIAN_POINT('Origin',(-1.5,-1.9,1.7));
#34954=CARTESIAN_POINT('Origin',(-1.5,-1.9,1.7));
#34955=CARTESIAN_POINT('',(-1.43596875762567,-1.7,1.75));
#34956=CARTESIAN_POINT('',(-1.43596875762567,-1.7,1.7));
#34957=CARTESIAN_POINT('',(-1.71,-1.9,1.75));
#34958=CARTESIAN_POINT('Origin',(-1.5,-1.9,1.75));
#34959=CARTESIAN_POINT('',(-1.71,-1.9,2.4));
#34960=CARTESIAN_POINT('',(-1.71,-1.9,1.7));
#34961=CARTESIAN_POINT('Origin',(-1.5,-1.9,2.4));
#34962=CARTESIAN_POINT('',(-1.56403124237433,-1.7,1.75));
#34963=CARTESIAN_POINT('Origin',(-1.5,-1.9,1.75));
#34964=CARTESIAN_POINT('',(-1.56403124237433,-1.7,1.7));
#34965=CARTESIAN_POINT('Origin',(1.5,1.9,1.7));
#34966=CARTESIAN_POINT('',(1.43596875762567,1.7,1.7));
#34967=CARTESIAN_POINT('',(1.56403124237433,1.7,1.7));
#34968=CARTESIAN_POINT('',(0.75,1.7,1.7));
#34969=CARTESIAN_POINT('Origin',(1.5,1.9,1.7));
#34970=CARTESIAN_POINT('Origin',(1.5,1.9,1.7));
#34971=CARTESIAN_POINT('',(1.43596875762567,1.7,1.75));
#34972=CARTESIAN_POINT('',(1.43596875762567,1.7,1.7));
#34973=CARTESIAN_POINT('',(1.29,1.9,1.75));
#34974=CARTESIAN_POINT('Origin',(1.5,1.9,1.75));
#34975=CARTESIAN_POINT('',(1.29,1.9,2.4));
#34976=CARTESIAN_POINT('',(1.29,1.9,1.7));
#34977=CARTESIAN_POINT('Origin',(1.5,1.9,2.4));
#34978=CARTESIAN_POINT('',(1.56403124237433,1.7,1.75));
#34979=CARTESIAN_POINT('Origin',(1.5,1.9,1.75));
#34980=CARTESIAN_POINT('',(1.56403124237433,1.7,1.7));
#34981=CARTESIAN_POINT('Origin',(0.,-1.7,1.75));
#34982=CARTESIAN_POINT('',(0.,-1.7,1.75));
#34983=CARTESIAN_POINT('',(-1.97,-1.7,1.75));
#34984=CARTESIAN_POINT('',(0.,-1.7,1.75));
#34985=CARTESIAN_POINT('',(-1.97,-1.7,0.43));
#34986=CARTESIAN_POINT('',(-1.97,-1.7,1.75));
#34987=CARTESIAN_POINT('',(1.97,-1.7,0.43));
#34988=CARTESIAN_POINT('',(0.,-1.7,0.43));
#34989=CARTESIAN_POINT('',(1.97,-1.7,1.75));
#34990=CARTESIAN_POINT('',(1.97,-1.7,1.75));
#34991=CARTESIAN_POINT('',(0.,-1.7,1.75));
#34992=CARTESIAN_POINT('Origin',(0.,1.7,0.43));
#34993=CARTESIAN_POINT('',(0.,1.7,1.75));
#34994=CARTESIAN_POINT('',(1.97,1.7,1.75));
#34995=CARTESIAN_POINT('',(0.,1.7,1.75));
#34996=CARTESIAN_POINT('',(1.97,1.7,0.43));
#34997=CARTESIAN_POINT('',(1.97,1.7,0.43));
#34998=CARTESIAN_POINT('',(-1.97,1.7,0.43));
#34999=CARTESIAN_POINT('',(0.,1.7,0.43));
#35000=CARTESIAN_POINT('',(-1.97,1.7,1.75));
#35001=CARTESIAN_POINT('',(-1.97,1.7,0.43));
#35002=CARTESIAN_POINT('',(0.,1.7,1.75));
#35003=CARTESIAN_POINT('Origin',(-1.97,0.,1.415));
#35004=CARTESIAN_POINT('',(-1.97,-2.35,1.75));
#35005=CARTESIAN_POINT('',(-1.97,-2.35,1.75));
#35006=CARTESIAN_POINT('',(-1.97,-2.35,2.4));
#35007=CARTESIAN_POINT('',(-1.97,-2.35,2.4));
#35008=CARTESIAN_POINT('',(-1.97,2.35,2.4));
#35009=CARTESIAN_POINT('',(-1.97,2.35,2.4));
#35010=CARTESIAN_POINT('',(-1.97,2.35,1.75));
#35011=CARTESIAN_POINT('',(-1.97,2.35,1.75));
#35012=CARTESIAN_POINT('',(-1.97,1.7,1.75));
#35013=CARTESIAN_POINT('',(-1.97,0.78,0.43));
#35014=CARTESIAN_POINT('',(-1.97,0.78,0.43));
#35015=CARTESIAN_POINT('',(-1.97,0.78,1.55));
#35016=CARTESIAN_POINT('',(-1.97,0.78,1.55));
#35017=CARTESIAN_POINT('',(-1.97,-0.78,1.55));
#35018=CARTESIAN_POINT('',(-1.97,-0.78,1.55));
#35019=CARTESIAN_POINT('',(-1.97,-0.78,0.43));
#35020=CARTESIAN_POINT('',(-1.97,-0.78,0.43));
#35021=CARTESIAN_POINT('',(-1.97,-1.7,0.43));
#35022=CARTESIAN_POINT('Origin',(0.,-2.35,1.75));
#35023=CARTESIAN_POINT('',(1.97,-2.35,1.75));
#35024=CARTESIAN_POINT('',(1.97,-2.35,1.75));
#35025=CARTESIAN_POINT('',(0.,-2.35,1.75));
#35026=CARTESIAN_POINT('Origin',(0.,-2.35,2.4));
#35027=CARTESIAN_POINT('',(1.97,-2.35,2.4));
#35028=CARTESIAN_POINT('',(1.97,-2.35,2.4));
#35029=CARTESIAN_POINT('',(0.,-2.35,2.4));
#35030=CARTESIAN_POINT('Origin',(0.,2.35,2.4));
#35031=CARTESIAN_POINT('',(1.97,2.35,2.4));
#35032=CARTESIAN_POINT('',(1.97,2.35,2.4));
#35033=CARTESIAN_POINT('',(0.,2.35,2.4));
#35034=CARTESIAN_POINT('Origin',(0.,2.35,1.75));
#35035=CARTESIAN_POINT('',(1.97,2.35,1.75));
#35036=CARTESIAN_POINT('',(1.97,2.35,1.75));
#35037=CARTESIAN_POINT('',(0.,2.35,1.75));
#35038=CARTESIAN_POINT('Origin',(0.,1.7,1.75));
#35039=CARTESIAN_POINT('',(1.97,1.7,1.75));
#35040=CARTESIAN_POINT('Origin',(0.,0.78,0.43));
#35041=CARTESIAN_POINT('',(1.97,0.78,0.43));
#35042=CARTESIAN_POINT('',(1.97,0.78,0.43));
#35043=CARTESIAN_POINT('',(0.,0.78,0.43));
#35044=CARTESIAN_POINT('Origin',(0.,0.78,1.55));
#35045=CARTESIAN_POINT('',(1.97,0.78,1.55));
#35046=CARTESIAN_POINT('',(1.97,0.78,1.55));
#35047=CARTESIAN_POINT('',(0.,0.78,1.55));
#35048=CARTESIAN_POINT('Origin',(0.,-0.78,1.55));
#35049=CARTESIAN_POINT('',(1.97,-0.78,1.55));
#35050=CARTESIAN_POINT('',(1.97,-0.78,1.55));
#35051=CARTESIAN_POINT('',(0.,-0.78,1.55));
#35052=CARTESIAN_POINT('Origin',(0.,-0.78,0.43));
#35053=CARTESIAN_POINT('',(1.97,-0.78,0.43));
#35054=CARTESIAN_POINT('',(1.97,-0.78,0.43));
#35055=CARTESIAN_POINT('',(0.,-0.78,0.43));
#35056=CARTESIAN_POINT('Origin',(0.,-1.7,0.43));
#35057=CARTESIAN_POINT('',(1.97,-1.7,0.43));
#35058=CARTESIAN_POINT('Origin',(1.97,0.,1.415));
#35059=CARTESIAN_POINT('',(0.,0.,0.));
#35060=CARTESIAN_POINT('Origin',(1.97,1.7,2.3));
#35061=CARTESIAN_POINT('',(1.97,1.7,2.3));
#35062=CARTESIAN_POINT('',(1.97,-1.7,2.3));
#35063=CARTESIAN_POINT('',(1.97,1.7,2.3));
#35064=CARTESIAN_POINT('',(3.07,-1.7,2.3));
#35065=CARTESIAN_POINT('',(1.97,-1.7,2.3));
#35066=CARTESIAN_POINT('',(3.07,1.7,2.3));
#35067=CARTESIAN_POINT('',(3.07,1.7,2.3));
#35068=CARTESIAN_POINT('',(1.97,1.7,2.3));
#35069=CARTESIAN_POINT('Origin',(1.97,1.7,0.46));
#35070=CARTESIAN_POINT('',(1.97,1.7,0.46));
#35071=CARTESIAN_POINT('',(1.97,1.7,0.46));
#35072=CARTESIAN_POINT('',(3.07,1.7,0.46));
#35073=CARTESIAN_POINT('',(3.07,1.7,0.46));
#35074=CARTESIAN_POINT('',(1.97,1.7,0.46));
#35075=CARTESIAN_POINT('Origin',(1.97,0.78,0.46));
#35076=CARTESIAN_POINT('',(1.97,0.78,0.46));
#35077=CARTESIAN_POINT('',(1.97,0.78,0.46));
#35078=CARTESIAN_POINT('',(3.07,0.78,0.46));
#35079=CARTESIAN_POINT('',(3.07,0.78,0.46));
#35080=CARTESIAN_POINT('',(1.97,0.78,0.46));
#35081=CARTESIAN_POINT('Origin',(1.97,0.78,1.55));
#35082=CARTESIAN_POINT('',(1.97,0.78,1.55));
#35083=CARTESIAN_POINT('',(1.97,0.78,1.55));
#35084=CARTESIAN_POINT('',(3.07,0.78,1.55));
#35085=CARTESIAN_POINT('',(3.07,0.78,1.55));
#35086=CARTESIAN_POINT('',(1.97,0.78,1.55));
#35087=CARTESIAN_POINT('Origin',(1.97,-0.78,1.55));
#35088=CARTESIAN_POINT('',(1.97,-0.78,1.55));
#35089=CARTESIAN_POINT('',(1.97,-0.78,1.55));
#35090=CARTESIAN_POINT('',(3.07,-0.78,1.55));
#35091=CARTESIAN_POINT('',(3.07,-0.78,1.55));
#35092=CARTESIAN_POINT('',(1.97,-0.78,1.55));
#35093=CARTESIAN_POINT('Origin',(1.97,-0.78,0.46));
#35094=CARTESIAN_POINT('',(1.97,-0.78,0.46));
#35095=CARTESIAN_POINT('',(1.97,-0.78,0.46));
#35096=CARTESIAN_POINT('',(3.07,-0.78,0.46));
#35097=CARTESIAN_POINT('',(3.07,-0.78,0.46));
#35098=CARTESIAN_POINT('',(1.97,-0.78,0.46));
#35099=CARTESIAN_POINT('Origin',(1.97,-1.7,0.46));
#35100=CARTESIAN_POINT('',(1.97,-1.7,0.46));
#35101=CARTESIAN_POINT('',(1.97,-1.7,0.46));
#35102=CARTESIAN_POINT('',(3.07,-1.7,0.46));
#35103=CARTESIAN_POINT('',(3.07,-1.7,0.46));
#35104=CARTESIAN_POINT('',(1.97,-1.7,0.46));
#35105=CARTESIAN_POINT('Origin',(1.97,-1.7,2.3));
#35106=CARTESIAN_POINT('',(1.97,-1.7,2.3));
#35107=CARTESIAN_POINT('',(3.07,-1.7,2.3));
#35108=CARTESIAN_POINT('Origin',(3.07,0.,1.38));
#35109=CARTESIAN_POINT('Origin',(1.97,0.,1.38));
#35110=CARTESIAN_POINT('',(0.,0.,0.));
#35111=CARTESIAN_POINT('Origin',(-1.97,-0.78,0.46));
#35112=CARTESIAN_POINT('',(-1.97,-1.7,0.46));
#35113=CARTESIAN_POINT('',(-1.97,-0.78,0.46));
#35114=CARTESIAN_POINT('',(-1.97,-1.7,0.46));
#35115=CARTESIAN_POINT('',(-3.07,-1.7,0.46));
#35116=CARTESIAN_POINT('',(-1.97,-1.7,0.46));
#35117=CARTESIAN_POINT('',(-3.07,-0.78,0.46));
#35118=CARTESIAN_POINT('',(-3.07,-1.7,0.46));
#35119=CARTESIAN_POINT('',(-1.97,-0.78,0.46));
#35120=CARTESIAN_POINT('Origin',(-1.97,-0.78,1.55));
#35121=CARTESIAN_POINT('',(-1.97,-0.78,1.55));
#35122=CARTESIAN_POINT('',(-1.97,-0.78,0.46));
#35123=CARTESIAN_POINT('',(-3.07,-0.78,1.55));
#35124=CARTESIAN_POINT('',(-3.07,-0.78,0.46));
#35125=CARTESIAN_POINT('',(-1.97,-0.78,1.55));
#35126=CARTESIAN_POINT('Origin',(-1.97,0.78,1.55));
#35127=CARTESIAN_POINT('',(-1.97,0.78,1.55));
#35128=CARTESIAN_POINT('',(-1.97,-0.78,1.55));
#35129=CARTESIAN_POINT('',(-3.07,0.78,1.55));
#35130=CARTESIAN_POINT('',(-3.07,-0.78,1.55));
#35131=CARTESIAN_POINT('',(-1.97,0.78,1.55));
#35132=CARTESIAN_POINT('Origin',(-1.97,0.78,0.46));
#35133=CARTESIAN_POINT('',(-1.97,0.78,0.46));
#35134=CARTESIAN_POINT('',(-1.97,0.78,1.55));
#35135=CARTESIAN_POINT('',(-3.07,0.78,0.46));
#35136=CARTESIAN_POINT('',(-3.07,0.78,1.55));
#35137=CARTESIAN_POINT('',(-1.97,0.78,0.46));
#35138=CARTESIAN_POINT('Origin',(-1.97,1.7,0.46));
#35139=CARTESIAN_POINT('',(-1.97,1.7,0.46));
#35140=CARTESIAN_POINT('',(-1.97,0.78,0.46));
#35141=CARTESIAN_POINT('',(-3.07,1.7,0.46));
#35142=CARTESIAN_POINT('',(-3.07,0.78,0.46));
#35143=CARTESIAN_POINT('',(-1.97,1.7,0.46));
#35144=CARTESIAN_POINT('Origin',(-1.97,1.7,2.3));
#35145=CARTESIAN_POINT('',(-1.97,1.7,2.3));
#35146=CARTESIAN_POINT('',(-1.97,1.7,0.46));
#35147=CARTESIAN_POINT('',(-3.07,1.7,2.3));
#35148=CARTESIAN_POINT('',(-3.07,1.7,0.46));
#35149=CARTESIAN_POINT('',(-1.97,1.7,2.3));
#35150=CARTESIAN_POINT('Origin',(-1.97,-1.7,2.3));
#35151=CARTESIAN_POINT('',(-1.97,-1.7,2.3));
#35152=CARTESIAN_POINT('',(-1.97,1.7,2.3));
#35153=CARTESIAN_POINT('',(-3.07,-1.7,2.3));
#35154=CARTESIAN_POINT('',(-3.07,1.7,2.3));
#35155=CARTESIAN_POINT('',(-1.97,-1.7,2.3));
#35156=CARTESIAN_POINT('Origin',(-1.97,-1.7,0.46));
#35157=CARTESIAN_POINT('',(-1.97,-1.7,2.3));
#35158=CARTESIAN_POINT('',(-3.07,-1.7,2.3));
#35159=CARTESIAN_POINT('Origin',(-1.97,0.,1.38));
#35160=CARTESIAN_POINT('Origin',(-3.07,0.,1.38));
#35161=CARTESIAN_POINT('',(0.,0.,0.));
#35162=CARTESIAN_POINT('',(0.,0.,0.));
#35163=CARTESIAN_POINT('',(0.,0.,0.));
#35164=CARTESIAN_POINT('',(0.,0.,0.));
#35165=CARTESIAN_POINT('Origin',(0.,0.09,0.));
#35166=CARTESIAN_POINT('',(-0.285,0.1,3.49024337756996E-17));
#35167=CARTESIAN_POINT('Origin',(0.,0.1,0.));
#35168=CARTESIAN_POINT('',(-0.265,0.08,-3.24531401774049E-17));
#35169=CARTESIAN_POINT('',(-0.275,0.09,3.36777869765522E-17));
#35170=CARTESIAN_POINT('Origin',(0.,0.08,0.));
#35171=CARTESIAN_POINT('Origin',(0.,0.,0.));
#35172=CARTESIAN_POINT('',(-0.265,0.,3.24531401774049E-17));
#35173=CARTESIAN_POINT('',(-0.265,0.,3.24531401774049E-17));
#35174=CARTESIAN_POINT('Origin',(0.,0.,0.));
#35175=CARTESIAN_POINT('Origin',(0.,0.1,0.));
#35176=CARTESIAN_POINT('',(-0.5,0.1,6.12323399573677E-17));
#35177=CARTESIAN_POINT('Origin',(0.,0.1,0.));
#35178=CARTESIAN_POINT('Origin',(0.,0.,0.));
#35179=CARTESIAN_POINT('',(-0.5,0.,6.12323399573677E-17));
#35180=CARTESIAN_POINT('',(-0.5,0.,6.12323399573677E-17));
#35181=CARTESIAN_POINT('Origin',(0.,0.,0.));
#35182=CARTESIAN_POINT('Origin',(0.,0.,0.));
#35183=CARTESIAN_POINT('',(0.,0.,0.));
#35184=CARTESIAN_POINT('Origin',(0.115470053837925,-0.5,-0.2));
#35185=CARTESIAN_POINT('',(0.23094010767585,-0.5,0.));
#35186=CARTESIAN_POINT('',(0.115470053837925,-0.5,-0.2));
#35187=CARTESIAN_POINT('',(0.23094010767585,-0.5,0.));
#35188=CARTESIAN_POINT('',(0.115470053837925,-0.8,-0.2));
#35189=CARTESIAN_POINT('',(0.115470053837925,-0.5,-0.2));
#35190=CARTESIAN_POINT('',(0.23094010767585,-0.8,0.));
#35191=CARTESIAN_POINT('',(0.23094010767585,-0.8,0.));
#35192=CARTESIAN_POINT('',(0.23094010767585,-0.5,0.));
#35193=CARTESIAN_POINT('Origin',(-0.115470053837925,-0.5,-0.2));
#35194=CARTESIAN_POINT('',(-0.115470053837925,-0.5,-0.2));
#35195=CARTESIAN_POINT('',(0.115470053837925,-0.5,-0.2));
#35196=CARTESIAN_POINT('',(-0.115470053837925,-0.8,-0.2));
#35197=CARTESIAN_POINT('',(-0.115470053837925,-0.5,-0.2));
#35198=CARTESIAN_POINT('',(0.115470053837925,-0.8,-0.2));
#35199=CARTESIAN_POINT('Origin',(-0.23094010767585,-0.5,-2.77555756156289E-17));
#35200=CARTESIAN_POINT('',(-0.23094010767585,-0.5,-2.82820063659975E-17));
#35201=CARTESIAN_POINT('',(-0.115470053837925,-0.5,-0.2));
#35202=CARTESIAN_POINT('',(-0.23094010767585,-0.8,-2.77555756156289E-17));
#35203=CARTESIAN_POINT('',(-0.23094010767585,-0.5,-2.82820063659975E-17));
#35204=CARTESIAN_POINT('',(-0.115470053837925,-0.8,-0.2));
#35205=CARTESIAN_POINT('Origin',(-0.115470053837925,-0.5,0.2));
#35206=CARTESIAN_POINT('',(-0.115470053837925,-0.5,0.2));
#35207=CARTESIAN_POINT('',(-0.23094010767585,-0.5,-2.82820063659975E-17));
#35208=CARTESIAN_POINT('',(-0.115470053837925,-0.8,0.2));
#35209=CARTESIAN_POINT('',(-0.115470053837925,-0.5,0.2));
#35210=CARTESIAN_POINT('',(-0.23094010767585,-0.8,-2.82820063659975E-17));
#35211=CARTESIAN_POINT('Origin',(0.115470053837925,-0.5,0.2));
#35212=CARTESIAN_POINT('',(0.115470053837925,-0.5,0.2));
#35213=CARTESIAN_POINT('',(-0.115470053837925,-0.5,0.2));
#35214=CARTESIAN_POINT('',(0.115470053837925,-0.8,0.2));
#35215=CARTESIAN_POINT('',(0.115470053837925,-0.5,0.2));
#35216=CARTESIAN_POINT('',(-0.115470053837925,-0.8,0.2));
#35217=CARTESIAN_POINT('Origin',(0.23094010767585,-0.5,0.));
#35218=CARTESIAN_POINT('',(0.115470053837925,-0.5,0.2));
#35219=CARTESIAN_POINT('',(0.115470053837925,-0.8,0.2));
#35220=CARTESIAN_POINT('Origin',(0.,-0.5,0.));
#35221=CARTESIAN_POINT('Origin',(0.,-0.8,0.));
#35222=CARTESIAN_POINT('Origin',(0.,-1.9,0.));
#35223=CARTESIAN_POINT('',(-0.25,-1.9,3.06161699786838E-17));
#35224=CARTESIAN_POINT('Origin',(0.,-1.9,0.));
#35225=CARTESIAN_POINT('',(-0.24505,-1.9,3.00099698131059E-17));
#35226=CARTESIAN_POINT('Origin',(0.,-1.9,0.));
#35227=CARTESIAN_POINT('Origin',(0.,-3.,0.));
#35228=CARTESIAN_POINT('',(-0.25,-3.,3.06161699786838E-17));
#35229=CARTESIAN_POINT('',(-0.25,-3.,3.06161699786838E-17));
#35230=CARTESIAN_POINT('Origin',(0.,-3.,0.));
#35231=CARTESIAN_POINT('Origin',(0.,-3.,0.));
#35232=CARTESIAN_POINT('Origin',(0.375,0.5,0.));
#35233=CARTESIAN_POINT('',(-0.375,0.5,-4.59242549680257E-17));
#35234=CARTESIAN_POINT('Origin',(0.,0.5,0.));
#35235=CARTESIAN_POINT('Origin',(0.,0.475,0.));
#35236=CARTESIAN_POINT('',(-0.425,0.45,-5.20474889637625E-17));
#35237=CARTESIAN_POINT('Origin',(0.,0.45,0.));
#35238=CARTESIAN_POINT('',(-0.4,0.475,-4.89858719658941E-17));
#35239=CARTESIAN_POINT('Origin',(0.,0.24,0.));
#35240=CARTESIAN_POINT('',(-0.425,0.0299999999999998,-5.20474889637625E-17));
#35241=CARTESIAN_POINT('Origin',(0.,0.0299999999999998,0.));
#35242=CARTESIAN_POINT('',(-0.425,0.24,-5.20474889637625E-17));
#35243=CARTESIAN_POINT('Origin',(0.,0.0150000000000001,0.));
#35244=CARTESIAN_POINT('',(-0.395,4.85722573273506E-17,-4.83735485663204E-17));
#35245=CARTESIAN_POINT('Origin',(0.,0.,0.));
#35246=CARTESIAN_POINT('',(-0.41,0.0150000000000001,-5.02105187650415E-17));
#35247=CARTESIAN_POINT('Origin',(0.27,0.,0.));
#35248=CARTESIAN_POINT('',(-0.27,0.,-3.30654635769785E-17));
#35249=CARTESIAN_POINT('Origin',(0.,0.,0.));
#35250=CARTESIAN_POINT('Origin',(0.,-0.02,0.));
#35251=CARTESIAN_POINT('',(-0.24505,-0.0498999999999999,3.00099698131059E-17));
#35252=CARTESIAN_POINT('Origin',(0.,-0.0498999999999999,0.));
#35253=CARTESIAN_POINT('',(-0.26,-0.02,-3.18408167778312E-17));
#35254=CARTESIAN_POINT('Origin',(0.,-0.995,0.));
#35255=CARTESIAN_POINT('',(-0.24505,-0.995,-3.00099698131059E-17));
#35256=CARTESIAN_POINT('',(0.,0.,0.));
#35257=CARTESIAN_POINT('Origin',(12.5,0.,4.));
#35258=CARTESIAN_POINT('',(12.7800042915148,-1.13874042544416E-5,4.45787212683272));
#35259=CARTESIAN_POINT('',(12.6699957084852,1.09516003635735E-5,4.45788309353564));
#35260=CARTESIAN_POINT('',(12.5,-5.60735153159594E-17,4.457875));
#35261=CARTESIAN_POINT('',(12.5,-0.186196943290586,3.58169363627331));
#35262=CARTESIAN_POINT('Ctrl Pts',(12.6699957084852,1.09516003635735E-5,
4.45788309353564));
#35263=CARTESIAN_POINT('Ctrl Pts',(12.6684300766731,0.0150239422001319,
4.45789815019349));
#35264=CARTESIAN_POINT('Ctrl Pts',(12.6668644448611,0.0300354905662504,
4.45717403092565));
#35265=CARTESIAN_POINT('Ctrl Pts',(12.6652988130491,0.0449730203321769,
4.45569984746698));
#35266=CARTESIAN_POINT('Ctrl Pts',(12.6574274409991,0.120072959788606,4.44828824124903));
#35267=CARTESIAN_POINT('Ctrl Pts',(12.6495560689492,0.193301947984492,4.42191743369942));
#35268=CARTESIAN_POINT('Ctrl Pts',(12.6416846968992,0.255884660534875,4.37974732787395));
#35269=CARTESIAN_POINT('Ctrl Pts',(12.6338133248492,0.318467373085258,4.33757722204849));
#35270=CARTESIAN_POINT('Ctrl Pts',(12.6259419527993,0.370403809990138,4.27960781794716));
#35271=CARTESIAN_POINT('Ctrl Pts',(12.6180705807493,0.405471379329245,4.2127856577826));
#35272=CARTESIAN_POINT('Ctrl Pts',(12.6101992086994,0.440538948668352,4.14596349761803));
#35273=CARTESIAN_POINT('Ctrl Pts',(12.6023278366494,0.458737650441686,4.07028858139023));
#35274=CARTESIAN_POINT('Ctrl Pts',(12.5944564645995,0.457884906392306,3.99482861029462));
#35275=CARTESIAN_POINT('Ctrl Pts',(12.5865850925495,0.457032162342926,3.91936863919901));
#35276=CARTESIAN_POINT('Ctrl Pts',(12.5787137204996,0.437127972470831,3.84412361323559));
#35277=CARTESIAN_POINT('Ctrl Pts',(12.5708423484496,0.400561475243013,3.77811083326841));
#35278=CARTESIAN_POINT('Ctrl Pts',(12.5629709763996,0.363994978015195,3.71209805330123));
#35279=CARTESIAN_POINT('Ctrl Pts',(12.5550996043497,0.310766173431653,3.6553175193303));
#35280=CARTESIAN_POINT('Ctrl Pts',(12.5472282322997,0.247245050961511,3.61457214242492));
#35281=CARTESIAN_POINT('Ctrl Pts',(12.5393568602498,0.183723928491369,3.57382676551955));
#35282=CARTESIAN_POINT('Ctrl Pts',(12.5314854881998,0.109910488134627,3.54911654567973));
#35283=CARTESIAN_POINT('Ctrl Pts',(12.5236141161499,0.034670519197381,3.5434092666393));
#35284=CARTESIAN_POINT('Ctrl Pts',(12.5157427440999,-0.0405694497398647,
3.53770198759887));
#35285=CARTESIAN_POINT('Ctrl Pts',(12.50787137205,-0.117235947257613,3.55099764935784));
#35286=CARTESIAN_POINT('Ctrl Pts',(12.5,-0.186196943290592,3.58169363627332));
#35287=CARTESIAN_POINT('',(12.5,-0.186217277007329,4.41832740439831));
#35288=CARTESIAN_POINT('Origin',(12.5,0.,4.));
#35289=CARTESIAN_POINT('Ctrl Pts',(12.5,-0.186217277007329,4.41832740439831));
#35290=CARTESIAN_POINT('Ctrl Pts',(12.5008157411716,-0.193365324225124,
4.41515241707318));
#35291=CARTESIAN_POINT('Ctrl Pts',(12.5016314823431,-0.200430783441492,
4.4117927098014));
#35292=CARTESIAN_POINT('Ctrl Pts',(12.5024472235147,-0.207403505574881,
4.40825058102053));
#35293=CARTESIAN_POINT('Ctrl Pts',(12.5103185955646,-0.274685741688951,
4.37407134077235));
#35294=CARTESIAN_POINT('Ctrl Pts',(12.5181899676146,-0.333333232193243,
4.32290684204764));
#35295=CARTESIAN_POINT('Ctrl Pts',(12.5260613396645,-0.376326743005614,
4.26088786252735));
#35296=CARTESIAN_POINT('Ctrl Pts',(12.5339327117145,-0.419320253817985,
4.19886888300706));
#35297=CARTESIAN_POINT('Ctrl Pts',(12.5418040837645,-0.446659784938435,
4.12599542269119));
#35298=CARTESIAN_POINT('Ctrl Pts',(12.5496754558144,-0.455065168373522,
4.05100019606997));
#35299=CARTESIAN_POINT('Ctrl Pts',(12.5575468278644,-0.463470551808608,
3.97600496944875));
#35300=CARTESIAN_POINT('Ctrl Pts',(12.5654181999143,-0.452941787558331,
3.89888797652218));
#35301=CARTESIAN_POINT('Ctrl Pts',(12.5732895719643,-0.424742400952558,
3.82888990513641));
#35302=CARTESIAN_POINT('Ctrl Pts',(12.5811609440142,-0.396543014346786,
3.75889183375065));
#35303=CARTESIAN_POINT('Ctrl Pts',(12.5890323160642,-0.350673005385519,
3.69601268390568));
#35304=CARTESIAN_POINT('Ctrl Pts',(12.5969036881141,-0.292628022669152,
3.64778723809593));
#35305=CARTESIAN_POINT('Ctrl Pts',(12.6047750601641,-0.234583039952784,
3.59956179228618));
#35306=CARTESIAN_POINT('Ctrl Pts',(12.6126464322141,-0.164363083481316,
3.56599005051166));
#35307=CARTESIAN_POINT('Ctrl Pts',(12.620517804264,-0.0903829156297007,
3.55109483330951));
#35308=CARTESIAN_POINT('Ctrl Pts',(12.628389176314,-0.0164027477780855,
3.53619961610736));
#35309=CARTESIAN_POINT('Ctrl Pts',(12.6362605483639,0.0613376314536766,
3.53998092347757));
#35310=CARTESIAN_POINT('Ctrl Pts',(12.6441319204139,0.13352290298843,3.56198566164487));
#35311=CARTESIAN_POINT('Ctrl Pts',(12.6520032924638,0.205708174523184,3.58399039981218));
#35312=CARTESIAN_POINT('Ctrl Pts',(12.6598746645138,0.272338338360929,3.62421856877658));
#35313=CARTESIAN_POINT('Ctrl Pts',(12.6677460365637,0.325429113408527,3.67784968145944));
#35314=CARTESIAN_POINT('Ctrl Pts',(12.6756174086137,0.378519888456125,3.7314807941423));
#35315=CARTESIAN_POINT('Ctrl Pts',(12.6834887806637,0.418071274713577,3.79851485054363));
#35316=CARTESIAN_POINT('Ctrl Pts',(12.6913601527136,0.439343931585728,3.87091926467948));
#35317=CARTESIAN_POINT('Ctrl Pts',(12.6992315247636,0.460616588457879,3.94332367881533));
#35318=CARTESIAN_POINT('Ctrl Pts',(12.7071028968135,0.46361051594473,4.02109845068571));
#35319=CARTESIAN_POINT('Ctrl Pts',(12.7149742688635,0.447966936692366,4.09492394607626));
#35320=CARTESIAN_POINT('Ctrl Pts',(12.7228456409134,0.432323357440003,4.16874944146681));
#35321=CARTESIAN_POINT('Ctrl Pts',(12.7307170129634,0.398042271448426,4.23862566037754));
#35322=CARTESIAN_POINT('Ctrl Pts',(12.7385883850133,0.349231538304918,4.29617944234672));
#35323=CARTESIAN_POINT('Ctrl Pts',(12.7464597570633,0.300420805161409,4.35373322431589));
#35324=CARTESIAN_POINT('Ctrl Pts',(12.7543311291133,0.237080424865968,4.39896456934351));
#35325=CARTESIAN_POINT('Ctrl Pts',(12.7622025011632,0.166800374688878,4.42645347375649));
#35326=CARTESIAN_POINT('Ctrl Pts',(12.7681364312804,0.113818899065861,4.4471763206439));
#35327=CARTESIAN_POINT('Ctrl Pts',(12.7740703613976,0.056893551674301,4.45781599184163));
#35328=CARTESIAN_POINT('Ctrl Pts',(12.7800042915148,-1.13874042544416E-5,
4.45787212683272));
#35329=CARTESIAN_POINT('Origin',(12.5,0.,4.));
#35330=CARTESIAN_POINT('',(13.0800042915148,2.8196954984682E-6,4.45783894202495));
#35331=CARTESIAN_POINT('',(12.9699957084852,-6.90274666573233E-6,4.45790451736119));
#35332=CARTESIAN_POINT('',(12.5,-5.60735153159594E-17,4.457875));
#35333=CARTESIAN_POINT('Ctrl Pts',(12.9699957084852,-6.90274666573233E-6,
4.45790451736119));
#35334=CARTESIAN_POINT('Ctrl Pts',(12.9628865412726,0.0681543496286777,
4.45785453236543));
#35335=CARTESIAN_POINT('Ctrl Pts',(12.95577737406,0.136337475731944,4.44242789501186));
#35336=CARTESIAN_POINT('Ctrl Pts',(12.9486682068475,0.197807532932104,4.41298560914613));
#35337=CARTESIAN_POINT('Ctrl Pts',(12.9407968347975,0.265868063186489,4.38038668734267));
#35338=CARTESIAN_POINT('Ctrl Pts',(12.9329254627476,0.325698883531032,4.33060565060516));
#35339=CARTESIAN_POINT('Ctrl Pts',(12.9250540906976,0.370130557623211,4.26960768492436));
#35340=CARTESIAN_POINT('Ctrl Pts',(12.9171827186476,0.41456223171539,4.20860971924356));
#35341=CARTESIAN_POINT('Ctrl Pts',(12.9093113465977,0.443594759555206,4.13639482461947));
#35342=CARTESIAN_POINT('Ctrl Pts',(12.9014399745477,0.453749217534713,4.06161640217293));
#35343=CARTESIAN_POINT('Ctrl Pts',(12.8935686024978,0.463903675514219,3.9868379797264));
#35344=CARTESIAN_POINT('Ctrl Pts',(12.8856972304478,0.455180063633418,3.90949602945742));
#35345=CARTESIAN_POINT('Ctrl Pts',(12.8778258583979,0.428623718850503,3.83885831972366));
#35346=CARTESIAN_POINT('Ctrl Pts',(12.8699544863479,0.402067374067587,3.7682206099899));
#35347=CARTESIAN_POINT('Ctrl Pts',(12.862083114298,0.357678296382559,3.70428714079136));
#35348=CARTESIAN_POINT('Ctrl Pts',(12.854211742248,0.300775561959983,3.65471896268111));
#35349=CARTESIAN_POINT('Ctrl Pts',(12.846340370198,0.243872827537407,3.60515078457087));
#35350=CARTESIAN_POINT('Ctrl Pts',(12.8384689981481,0.174456436377283,3.56994789754891));
#35351=CARTESIAN_POINT('Ctrl Pts',(12.8305976260981,0.100844448250471,3.55332860992135));
#35352=CARTESIAN_POINT('Ctrl Pts',(12.8227262540482,0.0272324601236582,
3.53670932229378));
#35353=CARTESIAN_POINT('Ctrl Pts',(12.8148548819982,-0.0505751249698428,
3.53867363406062));
#35354=CARTESIAN_POINT('Ctrl Pts',(12.8069835099483,-0.123254740362562,
3.558986165072));
#35355=CARTESIAN_POINT('Ctrl Pts',(12.7991121378983,-0.195934355755281,
3.57929869608338));
#35356=CARTESIAN_POINT('Ctrl Pts',(12.7912407658484,-0.263486001447217,
3.6179594463393));
#35357=CARTESIAN_POINT('Ctrl Pts',(12.7833693937984,-0.317815070570116,
3.67033575613656));
#35358=CARTESIAN_POINT('Ctrl Pts',(12.7754980217484,-0.372144139693014,
3.72271206593382));
#35359=CARTESIAN_POINT('Ctrl Pts',(12.7676266496985,-0.413250632246875,
3.78880393527241));
#35360=CARTESIAN_POINT('Ctrl Pts',(12.7597552776485,-0.43620881068128,3.86069167744737));
#35361=CARTESIAN_POINT('Ctrl Pts',(12.7518839055986,-0.459166989115684,
3.93257941962233));
#35362=CARTESIAN_POINT('Ctrl Pts',(12.7440125335486,-0.463976853430633,
4.01026303463365));
#35363=CARTESIAN_POINT('Ctrl Pts',(12.7361411614987,-0.450062064178823,
4.08443380953254));
#35364=CARTESIAN_POINT('Ctrl Pts',(12.7282697894487,-0.436147274927012,
4.15860458443143));
#35365=CARTESIAN_POINT('Ctrl Pts',(12.7203984173988,-0.403507832108441,
4.22926251921788));
#35366=CARTESIAN_POINT('Ctrl Pts',(12.7125270453488,-0.356054829243877,
4.28794078818664));
#35367=CARTESIAN_POINT('Ctrl Pts',(12.7046556732988,-0.308601826379312,
4.3466190571554));
#35368=CARTESIAN_POINT('Ctrl Pts',(12.6967843012489,-0.246335263468753,
4.39331766030646));
#35369=CARTESIAN_POINT('Ctrl Pts',(12.6889129291989,-0.176716536654988,
4.42244075943884));
#35370=CARTESIAN_POINT('Ctrl Pts',(12.682607188961,-0.120945115332726,4.44577121528397));
#35371=CARTESIAN_POINT('Ctrl Pts',(12.6763014487231,-0.0604553842193124,
4.45782245132557));
#35372=CARTESIAN_POINT('Ctrl Pts',(12.6699957084852,1.09516003635735E-5,
4.45788309353564));
#35373=CARTESIAN_POINT('Ctrl Pts',(12.7800042915148,-1.13874042544416E-5,
4.45787212683272));
#35374=CARTESIAN_POINT('Ctrl Pts',(12.7819417334476,-0.0185909818676029,
4.45789045503738));
#35375=CARTESIAN_POINT('Ctrl Pts',(12.7838791753803,-0.0371684007279871,
4.45678053845584));
#35376=CARTESIAN_POINT('Ctrl Pts',(12.7858166173131,-0.0556056617636943,
4.45452496135198));
#35377=CARTESIAN_POINT('Ctrl Pts',(12.793687989363,-0.130511927980435,4.44536108073615));
#35378=CARTESIAN_POINT('Ctrl Pts',(12.801559361413,-0.203104740355178,4.41728685570614));
#35379=CARTESIAN_POINT('Ctrl Pts',(12.8094307334629,-0.264685413403174,
4.37366637792357));
#35380=CARTESIAN_POINT('Ctrl Pts',(12.8173021055129,-0.32626608645117,4.33004590014099));
#35381=CARTESIAN_POINT('Ctrl Pts',(12.8251734775629,-0.37683462017242,4.27087916960585));
#35382=CARTESIAN_POINT('Ctrl Pts',(12.8330448496128,-0.410331463567461,
4.20325604577686));
#35383=CARTESIAN_POINT('Ctrl Pts',(12.8409162216628,-0.443828306962503,
4.13563292194788));
#35384=CARTESIAN_POINT('Ctrl Pts',(12.8487875937127,-0.460253460031337,
4.05955340482505));
#35385=CARTESIAN_POINT('Ctrl Pts',(12.8566589657627,-0.457638721839564,
3.98413398734005));
#35386=CARTESIAN_POINT('Ctrl Pts',(12.8645303378126,-0.45502398364779,3.90871456985506));
#35387=CARTESIAN_POINT('Ctrl Pts',(12.8724017098626,-0.433369354195409,
3.8339552520079));
#35388=CARTESIAN_POINT('Ctrl Pts',(12.8802730819125,-0.395269674734573,
3.76881432927916));
#35389=CARTESIAN_POINT('Ctrl Pts',(12.8881444539625,-0.357169995273737,
3.70367340655041));
#35390=CARTESIAN_POINT('Ctrl Pts',(12.8960158260125,-0.302625265804445,
3.64815087894007));
#35391=CARTESIAN_POINT('Ctrl Pts',(12.9038871980624,-0.238171498431664,
3.6088999265713));
#35392=CARTESIAN_POINT('Ctrl Pts',(12.9117585701124,-0.173717731058884,
3.56964897420252));
#35393=CARTESIAN_POINT('Ctrl Pts',(12.9196299421623,-0.0993549257826154,
3.5466695970753));
#35394=CARTESIAN_POINT('Ctrl Pts',(12.9275013142123,-0.023993864556795,
3.54271537903906));
#35395=CARTESIAN_POINT('Ctrl Pts',(12.9353726862622,0.0513671966690251,
3.53876116100282));
#35396=CARTESIAN_POINT('Ctrl Pts',(12.9432440583122,0.127726513844396,3.55383210205756));
#35397=CARTESIAN_POINT('Ctrl Pts',(12.9511154303621,0.195934065997641,3.58612227423372));
#35398=CARTESIAN_POINT('Ctrl Pts',(12.9589868024121,0.264141618150887,3.61841244640988));
#35399=CARTESIAN_POINT('Ctrl Pts',(12.9668581744621,0.324197405282005,3.66792184970745));
#35400=CARTESIAN_POINT('Ctrl Pts',(12.974729546512,0.368905033668178,3.72871784755079));
#35401=CARTESIAN_POINT('Ctrl Pts',(12.982600918562,0.41361266205435,3.78951384539413));
#35402=CARTESIAN_POINT('Ctrl Pts',(12.9904722906119,0.442972131695578,3.86159643778324));
#35403=CARTESIAN_POINT('Ctrl Pts',(12.9983436626619,0.453465341949404,3.93632807718928));
#35404=CARTESIAN_POINT('Ctrl Pts',(13.0062150347118,0.46395855220323,4.01105971659532));
#35405=CARTESIAN_POINT('Ctrl Pts',(13.0140864067618,0.455585503069655,4.0884404030183));
#35406=CARTESIAN_POINT('Ctrl Pts',(13.0219577788117,0.429349524305901,4.15919772637108));
#35407=CARTESIAN_POINT('Ctrl Pts',(13.0298291508617,0.403113545542148,4.22995504972387));
#35408=CARTESIAN_POINT('Ctrl Pts',(13.0377005229117,0.359014637148215,4.29408901000646));
#35409=CARTESIAN_POINT('Ctrl Pts',(13.0455718949616,0.302337104315659,4.34391453219887));
#35410=CARTESIAN_POINT('Ctrl Pts',(13.0534432670116,0.245659571483104,4.39374005439127));
#35411=CARTESIAN_POINT('Ctrl Pts',(13.0613146390615,0.176403414211925,4.4292571384935));
#35412=CARTESIAN_POINT('Ctrl Pts',(13.0691860111115,0.102867492605122,4.44620982627979));
#35413=CARTESIAN_POINT('Ctrl Pts',(13.0727921045793,0.0691786509558273,
4.45397632191734));
#35414=CARTESIAN_POINT('Ctrl Pts',(13.076398198047,0.0345915681853763,4.45784650391406));
#35415=CARTESIAN_POINT('Ctrl Pts',(13.0800042915148,2.8196954984682E-6,
4.45783894202495));
#35416=CARTESIAN_POINT('Origin',(12.5,0.,4.));
#35417=CARTESIAN_POINT('',(13.3800042915148,1.00338821889499E-5,4.45789143379912));
#35418=CARTESIAN_POINT('',(13.2699957084852,-6.83105689078257E-6,4.45784477598907));
#35419=CARTESIAN_POINT('',(12.5,-5.60735153159594E-17,4.457875));
#35420=CARTESIAN_POINT('Ctrl Pts',(13.2699957084852,-6.83105689078257E-6,
4.45784477598907));
#35421=CARTESIAN_POINT('Ctrl Pts',(13.265214377922,0.0458528260712244,4.45782008288951));
#35422=CARTESIAN_POINT('Ctrl Pts',(13.2604330473589,0.091719698604501,4.45096974854549));
#35423=CARTESIAN_POINT('Ctrl Pts',(13.2556517167957,0.135506404234727,4.43740478719402));
#35424=CARTESIAN_POINT('Ctrl Pts',(13.2477803447458,0.207591244700251,4.41507316710824));
#35425=CARTESIAN_POINT('Ctrl Pts',(13.2399089726958,0.274038390871736,4.37454348113122));
#35426=CARTESIAN_POINT('Ctrl Pts',(13.2320376006459,0.326885582178656,4.32067233995558));
#35427=CARTESIAN_POINT('Ctrl Pts',(13.2241662285959,0.379732773485576,4.26680119877995));
#35428=CARTESIAN_POINT('Ctrl Pts',(13.2162948565459,0.418980009927931,4.19958860240569));
#35429=CARTESIAN_POINT('Ctrl Pts',(13.208423484496,0.439924354792367,4.12708853413817));
#35430=CARTESIAN_POINT('Ctrl Pts',(13.200552112446,0.460868699656804,4.05458846587065));
#35431=CARTESIAN_POINT('Ctrl Pts',(13.1926807403961,0.463510152943321,3.97680092570987));
#35432=CARTESIAN_POINT('Ctrl Pts',(13.1848093683461,0.447532193317848,3.90304707640827));
#35433=CARTESIAN_POINT('Ctrl Pts',(13.1769379962962,0.431554233692375,3.82929322710668));
#35434=CARTESIAN_POINT('Ctrl Pts',(13.1690666242462,0.396956861154912,3.75957306866428));
#35435=CARTESIAN_POINT('Ctrl Pts',(13.1611952521963,0.347885826291745,3.70224106173923));
#35436=CARTESIAN_POINT('Ctrl Pts',(13.1533238801463,0.298814791428577,3.64490905481418));
#35437=CARTESIAN_POINT('Ctrl Pts',(13.1454525080963,0.235270094239705,3.59996519940648));
#35438=CARTESIAN_POINT('Ctrl Pts',(13.1375811360464,0.164866199243897,3.57279504942506));
#35439=CARTESIAN_POINT('Ctrl Pts',(13.1297097639964,0.0944623042480882,
3.54562489944363));
#35440=CARTESIAN_POINT('Ctrl Pts',(13.1218383919465,0.0171992114453437,
3.53622845488849));
#35441=CARTESIAN_POINT('Ctrl Pts',(13.1139670198965,-0.0576647601420857,
3.54573167743434));
#35442=CARTESIAN_POINT('Ctrl Pts',(13.1060956478466,-0.132528731729515,
3.55523489998019));
#35443=CARTESIAN_POINT('Ctrl Pts',(13.0982242757966,-0.204993582101629,
3.58363778962703));
#35444=CARTESIAN_POINT('Ctrl Pts',(13.0903529037467,-0.266375958336211,
3.62753687126191));
#35445=CARTESIAN_POINT('Ctrl Pts',(13.0824815316967,-0.327758334570793,
3.67143595289679));
#35446=CARTESIAN_POINT('Ctrl Pts',(13.0746101596467,-0.378058236667844,
3.73083122651971));
#35447=CARTESIAN_POINT('Ctrl Pts',(13.0667387875968,-0.411248303781717,
3.79860544673343));
#35448=CARTESIAN_POINT('Ctrl Pts',(13.0588674155468,-0.444438370895591,
3.86637966694714));
#35449=CARTESIAN_POINT('Ctrl Pts',(13.0509960434969,-0.460518603026287,
3.94253283375165));
#35450=CARTESIAN_POINT('Ctrl Pts',(13.0431246714469,-0.457562130387816,
4.0179396288708));
#35451=CARTESIAN_POINT('Ctrl Pts',(13.035253299397,-0.454605657749345,4.09334642398995));
#35452=CARTESIAN_POINT('Ctrl Pts',(13.027381927347,-0.432612480341706,4.16800684742375));
#35453=CARTESIAN_POINT('Ctrl Pts',(13.0195105552971,-0.394218007200806,
4.23297445406563));
#35454=CARTESIAN_POINT('Ctrl Pts',(13.0116391832471,-0.355823534059905,
4.29794206070751));
#35455=CARTESIAN_POINT('Ctrl Pts',(13.0037678111972,-0.301027765185743,
4.35321685055749));
#35456=CARTESIAN_POINT('Ctrl Pts',(12.9958964391472,-0.236396794305188,
4.39217532952931));
#35457=CARTESIAN_POINT('Ctrl Pts',(12.9880250670972,-0.171765823424632,
4.43113380850113));
#35458=CARTESIAN_POINT('Ctrl Pts',(12.9801536950473,-0.0972996505376846,
4.45377597659478));
#35459=CARTESIAN_POINT('Ctrl Pts',(12.9722823229973,-0.0219214440120968,
4.4573886572069));
#35460=CARTESIAN_POINT('Ctrl Pts',(12.9715201181599,-0.014622381881285,
4.45773848219561));
#35461=CARTESIAN_POINT('Ctrl Pts',(12.9707579133226,-0.00731476803234869,
4.45790987647069));
#35462=CARTESIAN_POINT('Ctrl Pts',(12.9699957084852,-6.90274666573233E-6,
4.45790451736119));
#35463=CARTESIAN_POINT('Ctrl Pts',(13.0800042915148,2.8196954984682E-6,
4.45783894202495));
#35464=CARTESIAN_POINT('Ctrl Pts',(13.084269570097,-0.0409086678841046,
4.4578299978409));
#35465=CARTESIAN_POINT('Ctrl Pts',(13.0885348486792,-0.0818224858219862,
4.45239605085009));
#35466=CARTESIAN_POINT('Ctrl Pts',(13.0928001272613,-0.121255029803553,
4.44156782927524));
#35467=CARTESIAN_POINT('Ctrl Pts',(13.1006714993113,-0.194025944662995,
4.42158485301405));
#35468=CARTESIAN_POINT('Ctrl Pts',(13.1085428713613,-0.261752088439453,
4.3832306090213));
#35469=CARTESIAN_POINT('Ctrl Pts',(13.1164142434112,-0.31631794022257,4.33110102808186));
#35470=CARTESIAN_POINT('Ctrl Pts',(13.1242856154612,-0.370883792005687,
4.27897144714243));
#35471=CARTESIAN_POINT('Ctrl Pts',(13.1321569875111,-0.412289351795463,
4.21306652925631));
#35472=CARTESIAN_POINT('Ctrl Pts',(13.1400283595611,-0.435573054271055,
4.14128356060242));
#35473=CARTESIAN_POINT('Ctrl Pts',(13.147899731611,-0.458856756746647,4.06950059194853));
#35474=CARTESIAN_POINT('Ctrl Pts',(13.155771103661,-0.464018601908056,3.99183957252686));
#35475=CARTESIAN_POINT('Ctrl Pts',(13.1636424757109,-0.45044005369213,3.91760650430194));
#35476=CARTESIAN_POINT('Ctrl Pts',(13.1715138477609,-0.436861505476204,
3.84337343607703));
#35477=CARTESIAN_POINT('Ctrl Pts',(13.1793852198109,-0.404542563882944,
3.77256831904885));
#35478=CARTESIAN_POINT('Ctrl Pts',(13.1872565918608,-0.357355958580309,
3.7136756228145));
#35479=CARTESIAN_POINT('Ctrl Pts',(13.1951279639108,-0.310169353277673,
3.65478292658016));
#35480=CARTESIAN_POINT('Ctrl Pts',(13.2029993359607,-0.248115084265664,
3.60780265113964));
#35481=CARTESIAN_POINT('Ctrl Pts',(13.2108707080107,-0.178629020319019,
3.57836437152041));
#35482=CARTESIAN_POINT('Ctrl Pts',(13.2187420800606,-0.109142956372374,
3.54892609190117));
#35483=CARTESIAN_POINT('Ctrl Pts',(13.2266134521106,-0.0322250974910928,
3.53702980810322));
#35484=CARTESIAN_POINT('Ctrl Pts',(13.2344848241605,0.0429076061587562,
3.54410103373967));
#35485=CARTESIAN_POINT('Ctrl Pts',(13.2423561962105,0.118040309808605,3.55117225937612));
#35486=CARTESIAN_POINT('Ctrl Pts',(13.2502275682605,0.191387858227023,3.57721099444696));
#35487=CARTESIAN_POINT('Ctrl Pts',(13.2580989403104,0.254161126126225,3.61909705689013));
#35488=CARTESIAN_POINT('Ctrl Pts',(13.2659703123604,0.316934394025428,3.66098311933329));
#35489=CARTESIAN_POINT('Ctrl Pts',(13.2738416844103,0.369133381405416,3.71871650914877));
#35490=CARTESIAN_POINT('Ctrl Pts',(13.2817130564603,0.404503162915977,3.78537912195109));
#35491=CARTESIAN_POINT('Ctrl Pts',(13.2895844285102,0.43987294442654,3.85204173475342));
#35492=CARTESIAN_POINT('Ctrl Pts',(13.2974558005602,0.458413520067676,3.92763357054259));
#35493=CARTESIAN_POINT('Ctrl Pts',(13.3053271726101,0.457903200829578,4.00309657448501));
#35494=CARTESIAN_POINT('Ctrl Pts',(13.3131985446601,0.457392881591479,4.07855957842742));
#35495=CARTESIAN_POINT('Ctrl Pts',(13.3210699167101,0.437831667474148,4.15389375052308));
#35496=CARTESIAN_POINT('Ctrl Pts',(13.32894128876,0.401563549045306,4.22007191138728));
#35497=CARTESIAN_POINT('Ctrl Pts',(13.33681266081,0.365295430616463,4.28625007225149));
#35498=CARTESIAN_POINT('Ctrl Pts',(13.3446840328599,0.31232040787611,4.34327222188425));
#35499=CARTESIAN_POINT('Ctrl Pts',(13.3525554049099,0.248986397312635,4.38430548273058));
#35500=CARTESIAN_POINT('Ctrl Pts',(13.3604267769598,0.185652386749161,4.42533874357692));
#35501=CARTESIAN_POINT('Ctrl Pts',(13.3682981490098,0.111959388362564,4.45038311563682));
#35502=CARTESIAN_POINT('Ctrl Pts',(13.3761695210597,0.0367379221854645,
4.45643756985705));
#35503=CARTESIAN_POINT('Ctrl Pts',(13.3774477778781,0.024522472144774,4.45742077168506));
#35504=CARTESIAN_POINT('Ctrl Pts',(13.3787260346965,0.0122667140672706,
4.45790318029249));
#35505=CARTESIAN_POINT('Ctrl Pts',(13.3800042915148,1.00338821889499E-5,
4.45789143379912));
#35506=CARTESIAN_POINT('Origin',(12.5,0.,4.));
#35507=CARTESIAN_POINT('',(13.6800042915148,-8.85210990424201E-6,4.45789764648838));
#35508=CARTESIAN_POINT('',(13.5699957084852,1.03170790782398E-5,4.4578580083501));
#35509=CARTESIAN_POINT('',(12.5,-5.60735153159594E-17,4.457875));
#35510=CARTESIAN_POINT('Ctrl Pts',(13.5699957084852,1.03170790782398E-5,
4.4578580083501));
#35511=CARTESIAN_POINT('Ctrl Pts',(13.5675422145714,0.0235408097699949,
4.45787795556699));
#35512=CARTESIAN_POINT('Ctrl Pts',(13.5650887206577,0.0470683081483061,
4.45609516914004));
#35513=CARTESIAN_POINT('Ctrl Pts',(13.562635226744,0.0703115975725277,4.45248338388903));
#35514=CARTESIAN_POINT('Ctrl Pts',(13.554763854694,0.144881409096958,4.44089594716616));
#35515=CARTESIAN_POINT('Ctrl Pts',(13.5468924826441,0.21652593236894,4.41048310506186));
#35516=CARTESIAN_POINT('Ctrl Pts',(13.5390211105941,0.276660113016528,4.36488918223832));
#35517=CARTESIAN_POINT('Ctrl Pts',(13.5311497385442,0.336794293664116,4.31929525941478));
#35518=CARTESIAN_POINT('Ctrl Pts',(13.5232783664942,0.385418131687311,4.25852025587201));
#35519=CARTESIAN_POINT('Ctrl Pts',(13.5154069944443,0.416705106451492,4.18984674794718));
#35520=CARTESIAN_POINT('Ctrl Pts',(13.5075356223943,0.447992081215673,4.12117324002235));
#35521=CARTESIAN_POINT('Ctrl Pts',(13.4996642503443,0.461942192720839,4.04460122771548));
#35522=CARTESIAN_POINT('Ctrl Pts',(13.4917928782944,0.456883820300162,3.96930621892307));
#35523=CARTESIAN_POINT('Ctrl Pts',(13.4839215062444,0.451825447879485,3.89401121013066));
#35524=CARTESIAN_POINT('Ctrl Pts',(13.4760501341945,0.427758591532965,3.81999320485271));
#35525=CARTESIAN_POINT('Ctrl Pts',(13.4681787621445,0.387567146091087,3.75612166820384));
#35526=CARTESIAN_POINT('Ctrl Pts',(13.4603073900946,0.347375700649209,3.69225013155497));
#35527=CARTESIAN_POINT('Ctrl Pts',(13.4524360180446,0.291059666111973,3.63852506353517));
#35528=CARTESIAN_POINT('Ctrl Pts',(13.4445646459947,0.225367307335285,3.60138425741911));
#35529=CARTESIAN_POINT('Ctrl Pts',(13.4366932739447,0.159674948558598,3.56424345130305));
#35530=CARTESIAN_POINT('Ctrl Pts',(13.4288219018947,0.0846062655424597,
3.54368690709073));
#35531=CARTESIAN_POINT('Ctrl Pts',(13.4209505298448,0.00915662451852634,
3.54217788424291));
#35532=CARTESIAN_POINT('Ctrl Pts',(13.4130791577948,-0.0662930165054059,
3.54066886139509));
#35533=CARTESIAN_POINT('Ctrl Pts',(13.4052077857449,-0.142123615537132,
3.55820735991178));
#35534=CARTESIAN_POINT('Ctrl Pts',(13.3973364136949,-0.209248507106454,
3.5926917681625));
#35535=CARTESIAN_POINT('Ctrl Pts',(13.389465041645,-0.276373398675776,3.62717617641322));
#35536=CARTESIAN_POINT('Ctrl Pts',(13.381593669595,-0.334792582782693,3.67860649439798));
#35537=CARTESIAN_POINT('Ctrl Pts',(13.3737222975451,-0.377505777353741,
3.74081990525232));
#35538=CARTESIAN_POINT('Ctrl Pts',(13.3658509254951,-0.420218971924789,
3.80303331610666));
#35539=CARTESIAN_POINT('Ctrl Pts',(13.3579795534451,-0.44722617695997,3.87602981983059));
#35540=CARTESIAN_POINT('Ctrl Pts',(13.3501081813952,-0.455291160112798,
3.95106235628872));
#35541=CARTESIAN_POINT('Ctrl Pts',(13.3422368093452,-0.463356143265626,
4.02609489274685));
#35542=CARTESIAN_POINT('Ctrl Pts',(13.3343654372953,-0.452478904536101,
4.10316346193917));
#35543=CARTESIAN_POINT('Ctrl Pts',(13.3264940652453,-0.423962846915058,
4.17303305431203));
#35544=CARTESIAN_POINT('Ctrl Pts',(13.3186226931954,-0.395446789294015,
4.24290264668488));
#35545=CARTESIAN_POINT('Ctrl Pts',(13.3107513211454,-0.349291912781453,
4.30557326223827));
#35546=CARTESIAN_POINT('Ctrl Pts',(13.3028799490955,-0.291028886105345,
4.35353517632783));
#35547=CARTESIAN_POINT('Ctrl Pts',(13.2950085770455,-0.232765859429236,
4.4014970904174));
#35548=CARTESIAN_POINT('Ctrl Pts',(13.2871372049956,-0.162394682589579,
4.43475030304313));
#35549=CARTESIAN_POINT('Ctrl Pts',(13.2792658329456,-0.0883478267899694,
4.44931013225873));
#35550=CARTESIAN_POINT('Ctrl Pts',(13.2761757914588,-0.059279469337623,
4.4550258417985));
#35551=CARTESIAN_POINT('Ctrl Pts',(13.273085749972,-0.0296446570187532,
4.45786073445524));
#35552=CARTESIAN_POINT('Ctrl Pts',(13.2699957084852,-6.83105689078257E-6,
4.45784477598907));
#35553=CARTESIAN_POINT('Ctrl Pts',(13.3800042915148,1.00338821889499E-5,
4.45789143379912));
#35554=CARTESIAN_POINT('Ctrl Pts',(13.3865974067464,-0.0632086430349686,
4.45783084661254));
#35555=CARTESIAN_POINT('Ctrl Pts',(13.393190521978,-0.12645185159805,4.44462381290384));
#35556=CARTESIAN_POINT('Ctrl Pts',(13.3997836372096,-0.184315051738561,
4.41918121595096));
#35557=CARTESIAN_POINT('Ctrl Pts',(13.4076550092596,-0.253396625517876,
4.3888058714441));
#35558=CARTESIAN_POINT('Ctrl Pts',(13.4155263813095,-0.314809839108902,
4.34099064604983));
#35559=CARTESIAN_POINT('Ctrl Pts',(13.4233977533595,-0.361195640434018,
4.28146516557999));
#35560=CARTESIAN_POINT('Ctrl Pts',(13.4312691254094,-0.407581441759134,
4.22193968511016));
#35561=CARTESIAN_POINT('Ctrl Pts',(13.4391404974594,-0.438939830818339,
4.15070394956476));
#35562=CARTESIAN_POINT('Ctrl Pts',(13.4470118695093,-0.451513179494438,
4.07629402890356));
#35563=CARTESIAN_POINT('Ctrl Pts',(13.4548832415593,-0.464086528170537,
4.00188410824235));
#35564=CARTESIAN_POINT('Ctrl Pts',(13.4627546136093,-0.457874836463529,
3.92430000246534));
#35565=CARTESIAN_POINT('Ctrl Pts',(13.4706259856592,-0.433622441953051,
3.85283849709185));
#35566=CARTESIAN_POINT('Ctrl Pts',(13.4784973577092,-0.409370047442573,
3.78137699171835));
#35567=CARTESIAN_POINT('Ctrl Pts',(13.4863687297591,-0.367076950128625,
3.71603808674838));
#35568=CARTESIAN_POINT('Ctrl Pts',(13.4942401018091,-0.311811067605128,
3.66465124389307));
#35569=CARTESIAN_POINT('Ctrl Pts',(13.502111473859,-0.25654518508163,3.61326440103776));
#35570=CARTESIAN_POINT('Ctrl Pts',(13.509982845909,-0.188306517348584,3.5758296202971));
#35571=CARTESIAN_POINT('Ctrl Pts',(13.5178542179589,-0.115272000283325,
3.55683265457144));
#35572=CARTESIAN_POINT('Ctrl Pts',(13.5257255900089,-0.0422374832180674,
3.53783568884578));
#35573=CARTESIAN_POINT('Ctrl Pts',(13.5335969620589,0.035592883179403,3.53727653813511));
#35574=CARTESIAN_POINT('Ctrl Pts',(13.5414683341088,0.108892804353757,3.55522220461956));
#35575=CARTESIAN_POINT('Ctrl Pts',(13.5493397061588,0.182192725528112,3.573167871104));
#35576=CARTESIAN_POINT('Ctrl Pts',(13.5572110782087,0.250962201479351,3.60961835478357));
#35577=CARTESIAN_POINT('Ctrl Pts',(13.5650824502587,0.306960690387823,3.66020584957927));
#35578=CARTESIAN_POINT('Ctrl Pts',(13.5729538223086,0.362959179296295,3.71079334437498));
#35579=CARTESIAN_POINT('Ctrl Pts',(13.5808251943586,0.406186681162,3.77551785028682));
#35580=CARTESIAN_POINT('Ctrl Pts',(13.5886965664085,0.431463310113251,3.84662352810933));
#35581=CARTESIAN_POINT('Ctrl Pts',(13.5965679384585,0.456739939064502,3.91772920593184));
#35582=CARTESIAN_POINT('Ctrl Pts',(13.6044393105085,0.464065695101298,3.99521605566501));
#35583=CARTESIAN_POINT('Ctrl Pts',(13.6123106825584,0.452562744007997,4.06979894583348));
#35584=CARTESIAN_POINT('Ctrl Pts',(13.6201820546084,0.441059792914696,4.14438183600196));
#35585=CARTESIAN_POINT('Ctrl Pts',(13.6280534266583,0.410728134691299,4.21606076660573));
#35586=CARTESIAN_POINT('Ctrl Pts',(13.6359247987083,0.365202365858889,4.27624656029457));
#35587=CARTESIAN_POINT('Ctrl Pts',(13.6437961707582,0.319676597026479,4.33643235398341));
#35588=CARTESIAN_POINT('Ctrl Pts',(13.6516675428082,0.258956717585058,4.38512501075732));
#35589=CARTESIAN_POINT('Ctrl Pts',(13.6595389148581,0.190318698434502,4.41648976353532));
#35590=CARTESIAN_POINT('Ctrl Pts',(13.666360707077,0.130832969391341,4.44367229602021));
#35591=CARTESIAN_POINT('Ctrl Pts',(13.6731824992959,0.065399948454096,4.45783988979956));
#35592=CARTESIAN_POINT('Ctrl Pts',(13.6800042915148,-8.85210990424201E-6,
4.45789764648838));
#35593=CARTESIAN_POINT('Origin',(12.5,0.,4.));
#35594=CARTESIAN_POINT('',(13.9800042915148,-4.68615130337092E-6,4.45784092071359));
#35595=CARTESIAN_POINT('',(13.8699957084852,1.23414887176878E-6,4.4579133809027));
#35596=CARTESIAN_POINT('',(12.5,-5.60735153159594E-17,4.457875));
#35597=CARTESIAN_POINT('Ctrl Pts',(13.8699957084852,1.23414887176878E-6,
4.4579133809027));
#35598=CARTESIAN_POINT('Ctrl Pts',(13.8698700512209,0.00120594270822336,
4.45791357044259));
#35599=CARTESIAN_POINT('Ctrl Pts',(13.8697443939566,0.00241064979645091,
4.45790891401425));
#35600=CARTESIAN_POINT('Ctrl Pts',(13.8696187366923,0.00361531855258033,
4.45789940262096));
#35601=CARTESIAN_POINT('Ctrl Pts',(13.8617473646423,0.0790776965455978,
4.45730359373015));
#35602=CARTESIAN_POINT('Ctrl Pts',(13.8538759925924,0.154389660535011,4.43765704798318));
#35603=CARTESIAN_POINT('Ctrl Pts',(13.8460046205424,0.22052669229976,4.40131398110731));
#35604=CARTESIAN_POINT('Ctrl Pts',(13.8381332484924,0.286663724064511,4.36497091423144));
#35605=CARTESIAN_POINT('Ctrl Pts',(13.8302618764425,0.343625823604597,4.31193132622667));
#35606=CARTESIAN_POINT('Ctrl Pts',(13.8223905043925,0.384587309076409,4.24855087033892));
#35607=CARTESIAN_POINT('Ctrl Pts',(13.8145191323426,0.42554879454822,4.18517041445118));
#35608=CARTESIAN_POINT('Ctrl Pts',(13.8066477602926,0.450509665951756,4.11144909068046));
#35609=CARTESIAN_POINT('Ctrl Pts',(13.7987763882427,0.456478899990553,4.03622081324714));
#35610=CARTESIAN_POINT('Ctrl Pts',(13.7909050161927,0.46244813402935,3.96099253581381));
#35611=CARTESIAN_POINT('Ctrl Pts',(13.7830336441427,0.449425730703409,3.88425730471787));
#35612=CARTESIAN_POINT('Ctrl Pts',(13.7751622720928,0.418972144817937,3.81521018611534));
#35613=CARTESIAN_POINT('Ctrl Pts',(13.7672909000428,0.388518558932466,3.74616306751281));
#35614=CARTESIAN_POINT('Ctrl Pts',(13.7594195279929,0.340633790487464,3.68480406140369));
#35615=CARTESIAN_POINT('Ctrl Pts',(13.7515481559429,0.281055798532888,3.6384857242654));
#35616=CARTESIAN_POINT('Ctrl Pts',(13.743676783893,0.221477806578313,3.59216738712712));
#35617=CARTESIAN_POINT('Ctrl Pts',(13.735805411843,0.150206591114165,3.56088971895966));
#35618=CARTESIAN_POINT('Ctrl Pts',(13.7279340397931,0.0757824736049535,
3.54840067521841));
#35619=CARTESIAN_POINT('Ctrl Pts',(13.7200626677431,0.00135835609574232,
3.53591163147717));
#35620=CARTESIAN_POINT('Ctrl Pts',(13.7121912956931,-0.0762186634585312,
3.54221121216214));
#35621=CARTESIAN_POINT('Ctrl Pts',(13.7043199236432,-0.14765264866984,3.56654454809098));
#35622=CARTESIAN_POINT('Ctrl Pts',(13.6964485515932,-0.219086633881149,
3.59087788401983));
#35623=CARTESIAN_POINT('Ctrl Pts',(13.6885771795433,-0.284377584749494,
3.63324497519255));
#35624=CARTESIAN_POINT('Ctrl Pts',(13.6807058074933,-0.335701785830877,
3.68856903744356));
#35625=CARTESIAN_POINT('Ctrl Pts',(13.6728344354434,-0.38702598691226,3.74389309969457));
#35626=CARTESIAN_POINT('Ctrl Pts',(13.6649630633934,-0.424383438206683,
3.81217413302386));
#35627=CARTESIAN_POINT('Ctrl Pts',(13.6570916913435,-0.443297653083863,
3.88523012494906));
#35628=CARTESIAN_POINT('Ctrl Pts',(13.6492203192935,-0.462211867961044,
3.95828611687427));
#35629=CARTESIAN_POINT('Ctrl Pts',(13.6413489472436,-0.462682846420982,
4.03611706739538));
#35630=CARTESIAN_POINT('Ctrl Pts',(13.6334775751936,-0.444654151830396,
4.10939661196244));
#35631=CARTESIAN_POINT('Ctrl Pts',(13.6256062031436,-0.42662545723981,4.18267615652949));
#35632=CARTESIAN_POINT('Ctrl Pts',(13.6177348310937,-0.3900970895987,4.25140429514248));
#35633=CARTESIAN_POINT('Ctrl Pts',(13.6098634590437,-0.339446187702822,
4.3073454393722));
#35634=CARTESIAN_POINT('Ctrl Pts',(13.6019920869938,-0.288795285806945,
4.36328658360191));
#35635=CARTESIAN_POINT('Ctrl Pts',(13.5941207149438,-0.224021849656302,
4.40644073344835));
#35636=CARTESIAN_POINT('Ctrl Pts',(13.5862493428939,-0.152887581692542,
4.43163679270085));
#35637=CARTESIAN_POINT('Ctrl Pts',(13.5808314647576,-0.103925749791867,
4.44897928111035));
#35638=CARTESIAN_POINT('Ctrl Pts',(13.5754135866214,-0.0519504158054226,
4.45781396031326));
#35639=CARTESIAN_POINT('Ctrl Pts',(13.5699957084852,1.03170790782398E-5,
4.4578580083501));
#35640=CARTESIAN_POINT('Ctrl Pts',(13.6800042915148,-8.85210990424201E-6,
4.45789764648838));
#35641=CARTESIAN_POINT('Ctrl Pts',(13.6810538713459,-0.010072447664127,
4.45790653275371));
#35642=CARTESIAN_POINT('Ctrl Pts',(13.6821034511769,-0.0201354698749596,
4.45758141170421));
#35643=CARTESIAN_POINT('Ctrl Pts',(13.683153031008,-0.0301761699425476,
4.45691829561871));
#35644=CARTESIAN_POINT('Ctrl Pts',(13.691024403058,-0.105476860309351,4.45194522614199));
#35645=CARTESIAN_POINT('Ctrl Pts',(13.6988957751079,-0.179522082183268,
4.42796223840642));
#35646=CARTESIAN_POINT('Ctrl Pts',(13.7067671471579,-0.24343910912634,4.38784317739428));
#35647=CARTESIAN_POINT('Ctrl Pts',(13.7146385192078,-0.307356136069411,
4.34772411638213));
#35648=CARTESIAN_POINT('Ctrl Pts',(13.7225098912578,-0.361144968081636,
4.2914689820934));
#35649=CARTESIAN_POINT('Ctrl Pts',(13.7303812633077,-0.398360171146024,
4.22581874179975));
#35650=CARTESIAN_POINT('Ctrl Pts',(13.7382526353577,-0.435575374210412,
4.1601685015061));
#35651=CARTESIAN_POINT('Ctrl Pts',(13.7461240074077,-0.456216948326962,
4.08512315520753));
#35652=CARTESIAN_POINT('Ctrl Pts',(13.7539953794576,-0.457811445030669,
4.00967527273228));
#35653=CARTESIAN_POINT('Ctrl Pts',(13.7618667515076,-0.459405941734377,
3.93422739025703));
#35654=CARTESIAN_POINT('Ctrl Pts',(13.7697381235575,-0.441953361025241,
3.85837697160509));
#35655=CARTESIAN_POINT('Ctrl Pts',(13.7776094956075,-0.407545019133394,
3.79121305720166));
#35656=CARTESIAN_POINT('Ctrl Pts',(13.7854808676574,-0.373136677241547,
3.72404914279823));
#35657=CARTESIAN_POINT('Ctrl Pts',(13.7933522397074,-0.321772574166988,
3.6655717326433));
#35658=CARTESIAN_POINT('Ctrl Pts',(13.8012236117573,-0.259607592342073,
3.6227880859492));
#35659=CARTESIAN_POINT('Ctrl Pts',(13.8090949838073,-0.19744261051716,3.5800044392551));
#35660=CARTESIAN_POINT('Ctrl Pts',(13.8169663558573,-0.124476749941891,
3.55291455602183));
#35661=CARTESIAN_POINT('Ctrl Pts',(13.8248377279072,-0.0494533988297167,
3.54476457579874));
#35662=CARTESIAN_POINT('Ctrl Pts',(13.8327090999572,0.0255699522824598,
3.53661459557564));
#35663=CARTESIAN_POINT('Ctrl Pts',(13.8405804720071,0.102650793931542,3.54740451836272));
#35664=CARTESIAN_POINT('Ctrl Pts',(13.8484518440571,0.172552645974024,3.57584140410587));
#35665=CARTESIAN_POINT('Ctrl Pts',(13.856323216107,0.242454498016503,3.60427828984902));
#35666=CARTESIAN_POINT('Ctrl Pts',(13.864194588157,0.305177360452382,3.65036213854823));
#35667=CARTESIAN_POINT('Ctrl Pts',(13.8720659602069,0.353205247972751,3.70857079263049));
#35668=CARTESIAN_POINT('Ctrl Pts',(13.8799373322569,0.40123313549312,3.76677944671275));
#35669=CARTESIAN_POINT('Ctrl Pts',(13.8878087043068,0.434566048097978,3.83711290617806));
#35670=CARTESIAN_POINT('Ctrl Pts',(13.8956800763568,0.44920975351361,3.9111432194385));
#35671=CARTESIAN_POINT('Ctrl Pts',(13.9035514484068,0.463853458929242,3.98517353269893));
#35672=CARTESIAN_POINT('Ctrl Pts',(13.9114228204567,0.459807957155645,4.06290069975448));
#35673=CARTESIAN_POINT('Ctrl Pts',(13.9192941925067,0.437558014523894,4.13501079227018));
#35674=CARTESIAN_POINT('Ctrl Pts',(13.9271655645566,0.415308071892144,4.20712088478587));
#35675=CARTESIAN_POINT('Ctrl Pts',(13.9350369366066,0.374853688402242,4.27361390276169));
#35676=CARTESIAN_POINT('Ctrl Pts',(13.9429083086565,0.321042451364188,4.32652208887851));
#35677=CARTESIAN_POINT('Ctrl Pts',(13.9507796807065,0.267231214326134,4.37943027499533));
#35678=CARTESIAN_POINT('Ctrl Pts',(13.9586510527564,0.200063123739928,4.41875362925314));
#35679=CARTESIAN_POINT('Ctrl Pts',(13.9665224248064,0.127586829849962,4.43978009385641));
#35680=CARTESIAN_POINT('Ctrl Pts',(13.9710163803759,0.086208370984788,4.45178460807712));
#35681=CARTESIAN_POINT('Ctrl Pts',(13.9755103359454,0.0430996806131821,
4.45782517307841));
#35682=CARTESIAN_POINT('Ctrl Pts',(13.9800042915148,-4.68615130337092E-6,
4.45784092071359));
#35683=CARTESIAN_POINT('Origin',(12.5,0.,4.));
#35684=CARTESIAN_POINT('',(14.2800042915148,1.11332528513013E-5,4.45786561359635));
#35685=CARTESIAN_POINT('',(14.1699957084852,-1.10604184835328E-5,4.4578646218584));
#35686=CARTESIAN_POINT('',(12.5,-5.60735153159594E-17,4.457875));
#35687=CARTESIAN_POINT('Ctrl Pts',(14.1699957084852,-1.10604184835328E-5,
4.4578646218584));
#35688=CARTESIAN_POINT('Ctrl Pts',(14.1643265158203,0.0543576752587709,
4.45781404039958));
#35689=CARTESIAN_POINT('Ctrl Pts',(14.1586573231555,0.108743966382031,4.44812254260427));
#35690=CARTESIAN_POINT('Ctrl Pts',(14.1529881304907,0.159684023833442,4.42916890146099));
#35691=CARTESIAN_POINT('Ctrl Pts',(14.1451167584407,0.230411580321883,4.40285278028461));
#35692=CARTESIAN_POINT('Ctrl Pts',(14.1372453863907,0.294495541512382,4.358681244225));
#35693=CARTESIAN_POINT('Ctrl Pts',(14.1293740143408,0.344256823700223,4.30194730133701));
#35694=CARTESIAN_POINT('Ctrl Pts',(14.1215026422908,0.394018105888063,4.24521335844902));
#35695=CARTESIAN_POINT('Ctrl Pts',(14.1136312702409,0.429456709073245,4.17591700873265));
#35696=CARTESIAN_POINT('Ctrl Pts',(14.1057598981909,0.446326079279053,4.10236192849032));
#35697=CARTESIAN_POINT('Ctrl Pts',(14.097888526141,0.46319544948486,4.02880684824799));
#35698=CARTESIAN_POINT('Ctrl Pts',(14.090017154091,0.461495586711293,3.95099303747972));
#35699=CARTESIAN_POINT('Ctrl Pts',(14.0821457820411,0.441430182931853,3.87824480690492));
#35700=CARTESIAN_POINT('Ctrl Pts',(14.0742744099911,0.421364779152413,3.80549657633012));
#35701=CARTESIAN_POINT('Ctrl Pts',(14.0664030379411,0.3829338343671,3.73781392594881));
#35702=CARTESIAN_POINT('Ctrl Pts',(14.0585316658912,0.330742470300218,3.68330716492384));
#35703=CARTESIAN_POINT('Ctrl Pts',(14.0506602938412,0.278551106233337,3.62880040389886));
#35704=CARTESIAN_POINT('Ctrl Pts',(14.0427889217913,0.212599322884887,3.58746953223022));
#35705=CARTESIAN_POINT('Ctrl Pts',(14.0349175497413,0.140790022250932,3.5642671654747));
#35706=CARTESIAN_POINT('Ctrl Pts',(14.0270461776914,0.0689807216169763,
3.54106479871918));
#35707=CARTESIAN_POINT('Ctrl Pts',(14.0191748056414,-0.00868609630248519,
3.53599093687678));
#35708=CARTESIAN_POINT('Ctrl Pts',(14.0113034335915,-0.0829037347177578,
3.5496535731032));
#35709=CARTESIAN_POINT('Ctrl Pts',(14.0034320615415,-0.15712137313303,3.56331620932962));
#35710=CARTESIAN_POINT('Ctrl Pts',(13.9955606894916,-0.227889832044114,
3.59571534362485));
#35711=CARTESIAN_POINT('Ctrl Pts',(13.9876893174416,-0.286729034540398,
3.64296863695132));
#35712=CARTESIAN_POINT('Ctrl Pts',(13.9798179453916,-0.345568237036683,
3.69022193027778));
#35713=CARTESIAN_POINT('Ctrl Pts',(13.9719465733417,-0.392478183118168,
3.75232938263547));
#35714=CARTESIAN_POINT('Ctrl Pts',(13.9640752012917,-0.421837725217638,
3.82184875237013));
#35715=CARTESIAN_POINT('Ctrl Pts',(13.9562038292418,-0.451197267317109,
3.8913681221048));
#35716=CARTESIAN_POINT('Ctrl Pts',(13.9483324571918,-0.463006405434566,
3.96829940921644));
#35717=CARTESIAN_POINT('Ctrl Pts',(13.9404610851419,-0.455850068491383,
4.04342405445454));
#35718=CARTESIAN_POINT('Ctrl Pts',(13.9325897130919,-0.448693731548199,
4.11854869969265));
#35719=CARTESIAN_POINT('Ctrl Pts',(13.924718341042,-0.422571919544373,4.19186670305722));
#35720=CARTESIAN_POINT('Ctrl Pts',(13.916846968992,-0.38061476952465,4.25459247959939));
#35721=CARTESIAN_POINT('Ctrl Pts',(13.908975596942,-0.338657619504927,4.31731825614156));
#35722=CARTESIAN_POINT('Ctrl Pts',(13.9011042248921,-0.280865131469307,
4.36945180586132));
#35723=CARTESIAN_POINT('Ctrl Pts',(13.8932328528421,-0.214162491453186,
4.40474604470388));
#35724=CARTESIAN_POINT('Ctrl Pts',(13.8854871380565,-0.148524681204106,
4.43947685223224));
#35725=CARTESIAN_POINT('Ctrl Pts',(13.8777414232708,-0.0742589286223064,
4.45790169736071));
#35726=CARTESIAN_POINT('Ctrl Pts',(13.8699957084852,1.23414887176878E-6,
4.4579133809027));
#35727=CARTESIAN_POINT('Ctrl Pts',(13.9800042915148,-4.68615130337092E-6,
4.45784092071359));
#35728=CARTESIAN_POINT('Ctrl Pts',(13.9833817079953,-0.0323996211791616,
4.45785275579335));
#35729=CARTESIAN_POINT('Ctrl Pts',(13.9867591244758,-0.064792114138131,
4.45446164082457));
#35730=CARTESIAN_POINT('Ctrl Pts',(13.9901365409563,-0.0964458636128916,
4.44764173788363));
#35731=CARTESIAN_POINT('Ctrl Pts',(13.9980079130062,-0.170217765992045,
4.43174734235885));
#35732=CARTESIAN_POINT('Ctrl Pts',(14.0058792850562,-0.239977073556624,
4.39722897636055));
#35733=CARTESIAN_POINT('Ctrl Pts',(14.0137506571061,-0.297364634468633,
4.34822292324149));
#35734=CARTESIAN_POINT('Ctrl Pts',(14.0216220291561,-0.354752195380644,
4.29921687012243));
#35735=CARTESIAN_POINT('Ctrl Pts',(14.0294934012061,-0.399768009640084,
4.23572312988262));
#35736=CARTESIAN_POINT('Ctrl Pts',(14.037364773256,-0.427017900618165,4.16535006094698));
#35737=CARTESIAN_POINT('Ctrl Pts',(14.045236145306,-0.454267791596245,4.09497699201134));
#35738=CARTESIAN_POINT('Ctrl Pts',(14.0531075173559,-0.463751759292965,
4.01772459437987));
#35739=CARTESIAN_POINT('Ctrl Pts',(14.0609788894059,-0.45433335426851,3.94284990548881));
#35740=CARTESIAN_POINT('Ctrl Pts',(14.0688502614558,-0.444914949244056,
3.86797521659775));
#35741=CARTESIAN_POINT('Ctrl Pts',(14.0767216335058,-0.416594171498428,
3.7954782364471));
#35742=CARTESIAN_POINT('Ctrl Pts',(14.0845930055557,-0.372764656800254,
3.7340461680214));
#35743=CARTESIAN_POINT('Ctrl Pts',(14.0924643776057,-0.328935142102078,
3.67261409959569));
#35744=CARTESIAN_POINT('Ctrl Pts',(14.1003357496557,-0.269596890451354,
3.62224694289495));
#35745=CARTESIAN_POINT('Ctrl Pts',(14.1082071217056,-0.201860314388951,
3.58898011778223));
#35746=CARTESIAN_POINT('Ctrl Pts',(14.1160784937556,-0.134123738326549,
3.55571329266952));
#35747=CARTESIAN_POINT('Ctrl Pts',(14.1239498658055,-0.0579888378524715,
3.53954679914483));
#35748=CARTESIAN_POINT('Ctrl Pts',(14.1318212378555,0.0174212575835846,
3.54241784356498));
#35749=CARTESIAN_POINT('Ctrl Pts',(14.1396926099054,0.0928313530196406,
3.54528888798513));
#35750=CARTESIAN_POINT('Ctrl Pts',(14.1475639819554,0.167516643417675,3.56719747035013));
#35751=CARTESIAN_POINT('Ctrl Pts',(14.1554353540053,0.232527703900953,3.60551831852155));
#35752=CARTESIAN_POINT('Ctrl Pts',(14.1633067260553,0.297538764384231,3.64383916669297));
#35753=CARTESIAN_POINT('Ctrl Pts',(14.1711780981053,0.352875594952755,3.69857228067082));
#35754=CARTESIAN_POINT('Ctrl Pts',(14.1790494701552,0.391907267274456,3.76315907456484));
#35755=CARTESIAN_POINT('Ctrl Pts',(14.1869208422052,0.430938939596158,3.82774586845886));
#35756=CARTESIAN_POINT('Ctrl Pts',(14.1947922142551,0.453665453671035,3.90218634226906));
#35757=CARTESIAN_POINT('Ctrl Pts',(14.2026635863051,0.45736352584659,3.97756040711846));
#35758=CARTESIAN_POINT('Ctrl Pts',(14.210534958355,0.461061598022145,4.05293447196787));
#35759=CARTESIAN_POINT('Ctrl Pts',(14.218406330405,0.445731228298378,4.12924212785648));
#35760=CARTESIAN_POINT('Ctrl Pts',(14.2262777024549,0.413209431587385,4.19733954431574));
#35761=CARTESIAN_POINT('Ctrl Pts',(14.2341490745049,0.380687634876391,4.265436960775));
#35762=CARTESIAN_POINT('Ctrl Pts',(14.2420204465549,0.330974411178171,4.32532413780492));
#35763=CARTESIAN_POINT('Ctrl Pts',(14.2498918186048,0.270026820557645,4.36982488597043));
#35764=CARTESIAN_POINT('Ctrl Pts',(14.2577631906548,0.209079229937118,4.41432563413594));
#35765=CARTESIAN_POINT('Ctrl Pts',(14.2656345627047,0.136897272394287,4.44343995343705));
#35766=CARTESIAN_POINT('Ctrl Pts',(14.2735059347547,0.0621304022332317,
4.45367911922619));
#35767=CARTESIAN_POINT('Ctrl Pts',(14.2756720536747,0.0415553447945806,
4.4564968301158));
#35768=CARTESIAN_POINT('Ctrl Pts',(14.2778381725948,0.020784533837212,4.45788513960506));
#35769=CARTESIAN_POINT('Ctrl Pts',(14.2800042915148,1.11332528513013E-5,
4.45786561359635));
#35770=CARTESIAN_POINT('Origin',(12.5,0.,4.));
#35771=CARTESIAN_POINT('',(14.5800042915148,-1.58578451148518E-6,4.45791318879952));
#35772=CARTESIAN_POINT('',(14.4699957084852,4.96934848862042E-6,4.4578413260902));
#35773=CARTESIAN_POINT('',(12.5,-5.60735153159594E-17,4.457875));
#35774=CARTESIAN_POINT('Ctrl Pts',(14.4699957084852,4.96934848862042E-6,
4.4578413260902));
#35775=CARTESIAN_POINT('Ctrl Pts',(14.4666543524698,0.0320539454002899,
4.45785375637851));
#35776=CARTESIAN_POINT('Ctrl Pts',(14.4633129964543,0.0641003838712636,
4.45453523052653));
#35777=CARTESIAN_POINT('Ctrl Pts',(14.4599716404389,0.0954313752779353,
4.44785911407655));
#35778=CARTESIAN_POINT('Ctrl Pts',(14.452100268389,0.169239101517837,4.43213190746217));
#35779=CARTESIAN_POINT('Ctrl Pts',(14.444228896339,0.2390764403586,4.39777168651743));
#35780=CARTESIAN_POINT('Ctrl Pts',(14.4363575242891,0.296574889592956,4.34889578431359));
#35781=CARTESIAN_POINT('Ctrl Pts',(14.4284861522391,0.354073338827311,4.30001988210975));
#35782=CARTESIAN_POINT('Ctrl Pts',(14.4206147801891,0.39923289845526,4.2366282986468));
#35783=CARTESIAN_POINT('Ctrl Pts',(14.4127434081392,0.4266421670589,4.16631715105832));
#35784=CARTESIAN_POINT('Ctrl Pts',(14.4048720360892,0.454051435662541,4.09600600346984));
#35785=CARTESIAN_POINT('Ctrl Pts',(14.3970006640393,0.463710413241873,4.01877529175582));
#35786=CARTESIAN_POINT('Ctrl Pts',(14.3891292919893,0.454461679188747,3.94387945476197));
#35787=CARTESIAN_POINT('Ctrl Pts',(14.3812579199394,0.445212945135621,3.86898361776811));
#35788=CARTESIAN_POINT('Ctrl Pts',(14.3733865478894,0.417056499450037,3.79642265549441));
#35789=CARTESIAN_POINT('Ctrl Pts',(14.3655151758395,0.373366286239542,3.73489143780602));
#35790=CARTESIAN_POINT('Ctrl Pts',(14.3576438037895,0.329676073029047,3.67336022011762));
#35791=CARTESIAN_POINT('Ctrl Pts',(14.3497724317395,0.270452092293641,3.62285874701452));
#35792=CARTESIAN_POINT('Ctrl Pts',(14.3419010596896,0.202791063664024,3.58943853329022));
#35793=CARTESIAN_POINT('Ctrl Pts',(14.3340296876396,0.135130035034407,3.55601831956592));
#35794=CARTESIAN_POINT('Ctrl Pts',(14.3261583155897,0.0590319585105798,
3.53967936522043));
#35795=CARTESIAN_POINT('Ctrl Pts',(14.3182869435397,-0.0163844490157649,
3.54237954232867));
#35796=CARTESIAN_POINT('Ctrl Pts',(14.3104155714898,-0.0918008565421096,
3.54507971943691));
#35797=CARTESIAN_POINT('Ctrl Pts',(14.3025441994398,-0.166535595070972,
3.56681902799889));
#35798=CARTESIAN_POINT('Ctrl Pts',(14.2946728273899,-0.231633314431234,
3.60499247969884));
#35799=CARTESIAN_POINT('Ctrl Pts',(14.2868014553399,-0.296731033791496,
3.64316593139879));
#35800=CARTESIAN_POINT('Ctrl Pts',(14.2789300832899,-0.352191733983158,
3.6977735262367));
#35801=CARTESIAN_POINT('Ctrl Pts',(14.27105871124,-0.391369643565407,3.76227171909014));
#35802=CARTESIAN_POINT('Ctrl Pts',(14.26318733919,-0.430547553147657,3.82676991194359));
#35803=CARTESIAN_POINT('Ctrl Pts',(14.2553159671401,-0.453442672120494,
3.90115870281258));
#35804=CARTESIAN_POINT('Ctrl Pts',(14.2474445950901,-0.457311513162664,
3.97652419590847));
#35805=CARTESIAN_POINT('Ctrl Pts',(14.2395732230402,-0.461180354204834,
4.05188968900435));
#35806=CARTESIAN_POINT('Ctrl Pts',(14.2317018509902,-0.446022917316338,
4.12823188432714));
#35807=CARTESIAN_POINT('Ctrl Pts',(14.2238304789403,-0.413655495130362,
4.19640281260034));
#35808=CARTESIAN_POINT('Ctrl Pts',(14.2159591068903,-0.381288072944386,
4.26457374087354));
#35809=CARTESIAN_POINT('Ctrl Pts',(14.2080877348403,-0.33171066546093,4.32457340209717));
#35810=CARTESIAN_POINT('Ctrl Pts',(14.2002163627904,-0.270864058094251,
4.36921212802613));
#35811=CARTESIAN_POINT('Ctrl Pts',(14.1923449907404,-0.210017450727571,
4.41385085395509));
#35812=CARTESIAN_POINT('Ctrl Pts',(14.1844736186905,-0.137901643477669,
4.44312864458938));
#35813=CARTESIAN_POINT('Ctrl Pts',(14.1766022466405,-0.0631581639595259,
4.45353718675995));
#35814=CARTESIAN_POINT('Ctrl Pts',(14.1744000672554,-0.0422471272657682,
4.45644919204336));
#35815=CARTESIAN_POINT('Ctrl Pts',(14.1721978878703,-0.021130418320356,
4.45788427006097));
#35816=CARTESIAN_POINT('Ctrl Pts',(14.1699957084852,-1.10604184835328E-5,
4.4578646218584));
#35817=CARTESIAN_POINT('Ctrl Pts',(14.2800042915148,1.11332528513013E-5,
4.45786561359635));
#35818=CARTESIAN_POINT('Ctrl Pts',(14.2857095446447,-0.0547030874695854,
4.45781418483069));
#35819=CARTESIAN_POINT('Ctrl Pts',(14.2914147977746,-0.109435272994953,
4.44799629651036));
#35820=CARTESIAN_POINT('Ctrl Pts',(14.2971200509045,-0.16065599949712,4.42880599334559));
#35821=CARTESIAN_POINT('Ctrl Pts',(14.3049914229545,-0.231323748287136,
4.40232968939868));
#35822=CARTESIAN_POINT('Ctrl Pts',(14.3128627950045,-0.295307463087888,
4.35801306922771));
#35823=CARTESIAN_POINT('Ctrl Pts',(14.3207341670544,-0.344940072567234,
4.30116652609615));
#35824=CARTESIAN_POINT('Ctrl Pts',(14.3286055391044,-0.394572682046581,
4.24431998296459));
#35825=CARTESIAN_POINT('Ctrl Pts',(14.3364769111543,-0.429854186204522,
4.17494351687244));
#35826=CARTESIAN_POINT('Ctrl Pts',(14.3443482832043,-0.446556856002091,
4.10135040434572));
#35827=CARTESIAN_POINT('Ctrl Pts',(14.3522196552542,-0.46325952579966,4.027757291819));
#35828=CARTESIAN_POINT('Ctrl Pts',(14.3600910273042,-0.461383361236856,
3.9499475328577));
#35829=CARTESIAN_POINT('Ctrl Pts',(14.3679623993541,-0.441153180262727,
3.87724495265939));
#35830=CARTESIAN_POINT('Ctrl Pts',(14.3758337714041,-0.420922999288597,
3.80454237246108));
#35831=CARTESIAN_POINT('Ctrl Pts',(14.383705143454,-0.382338801903142,3.73694697102576));
#35832=CARTESIAN_POINT('Ctrl Pts',(14.391576515504,-0.330024073856894,3.68255860260764));
#35833=CARTESIAN_POINT('Ctrl Pts',(14.399447887554,-0.277709345810648,3.62817023418952));
#35834=CARTESIAN_POINT('Ctrl Pts',(14.4073192596039,-0.21166408710361,3.58698889878861));
#35835=CARTESIAN_POINT('Ctrl Pts',(14.4151906316539,-0.139802400742051,
3.56394929325792));
#35836=CARTESIAN_POINT('Ctrl Pts',(14.4230620037038,-0.0679407143804897,
3.54090968772722));
#35837=CARTESIAN_POINT('Ctrl Pts',(14.4309333757538,0.00973739963559066,
3.53601181206673));
#35838=CARTESIAN_POINT('Ctrl Pts',(14.4388047478037,0.0839238909224197,
3.54984257127538));
#35839=CARTESIAN_POINT('Ctrl Pts',(14.4466761198537,0.158110382209248,3.56367333048403));
#35840=CARTESIAN_POINT('Ctrl Pts',(14.4545474919037,0.228805250766822,3.59623272456181));
#35841=CARTESIAN_POINT('Ctrl Pts',(14.4624188639536,0.287537237904754,3.64361921078484));
#35842=CARTESIAN_POINT('Ctrl Pts',(14.4702902360036,0.346269225042686,3.69100569700788));
#35843=CARTESIAN_POINT('Ctrl Pts',(14.4781616080535,0.393038330760977,3.75321927537615));
#35844=CARTESIAN_POINT('Ctrl Pts',(14.4860329801035,0.422240284179214,3.8228049873169));
#35845=CARTESIAN_POINT('Ctrl Pts',(14.4939043521534,0.451442237597453,3.89239069925764));
#35846=CARTESIAN_POINT('Ctrl Pts',(14.5017757242034,0.463077038715637,3.96934854477086));
#35847=CARTESIAN_POINT('Ctrl Pts',(14.5096470962533,0.45575050699275,4.04445678215295));
#35848=CARTESIAN_POINT('Ctrl Pts',(14.5175184683033,0.448423975269863,4.11956501953505));
#35849=CARTESIAN_POINT('Ctrl Pts',(14.5253898403532,0.422136110705906,4.19282364878603));
#35850=CARTESIAN_POINT('Ctrl Pts',(14.5332612124032,0.380036948171907,4.2554541996672));
#35851=CARTESIAN_POINT('Ctrl Pts',(14.5411325844532,0.337937785637909,4.31808475054837));
#35852=CARTESIAN_POINT('Ctrl Pts',(14.5490039565031,0.28002732513387,4.37008722305972));
#35853=CARTESIAN_POINT('Ctrl Pts',(14.5568753285531,0.213244889156206,4.40523023992844));
#35854=CARTESIAN_POINT('Ctrl Pts',(14.5645849828737,0.147834501639678,4.43965124177167));
#35855=CARTESIAN_POINT('Ctrl Pts',(14.5722946371942,0.0739129441497101,
4.45789842831743));
#35856=CARTESIAN_POINT('Ctrl Pts',(14.5800042915148,-1.58578451148518E-6,
4.45791318879952));
#35857=CARTESIAN_POINT('Origin',(12.5,0.,4.));
#35858=CARTESIAN_POINT('',(14.8800042915148,-1.01702808208336E-5,4.45785711824254));
#35859=CARTESIAN_POINT('',(14.7699957084852,8.6346448269735E-6,4.45789857801605));
#35860=CARTESIAN_POINT('',(12.5,-5.60735153159594E-17,4.457875));
#35861=CARTESIAN_POINT('Ctrl Pts',(14.7699957084852,8.6346448269735E-6,
4.45789857801605));
#35862=CARTESIAN_POINT('Ctrl Pts',(14.7689821891192,0.00972641784825355,
4.45790700998655));
#35863=CARTESIAN_POINT('Ctrl Pts',(14.7679686697532,0.01944367562558,4.45760386164098));
#35864=CARTESIAN_POINT('Ctrl Pts',(14.7669551503872,0.0291408329004781,
4.45698549795522));
#35865=CARTESIAN_POINT('Ctrl Pts',(14.7590837783372,0.104452598317788,4.45218305332902));
#35866=CARTESIAN_POINT('Ctrl Pts',(14.7512124062873,0.178551969979598,4.4283678943965));
#35867=CARTESIAN_POINT('Ctrl Pts',(14.7433410342373,0.242559732875008,4.38839375563686));
#35868=CARTESIAN_POINT('Ctrl Pts',(14.7354696621874,0.30656749577042,4.34841961687722));
#35869=CARTESIAN_POINT('Ctrl Pts',(14.7275982901374,0.360483649899433,4.29228649829047));
#35870=CARTESIAN_POINT('Ctrl Pts',(14.7197269180875,0.397847504376097,4.22672074611392));
#35871=CARTESIAN_POINT('Ctrl Pts',(14.7118555460375,0.435211358852761,4.16115499393738));
#35872=CARTESIAN_POINT('Ctrl Pts',(14.7039841739875,0.456022913677073,4.08615660817103));
#35873=CARTESIAN_POINT('Ctrl Pts',(14.6961128019376,0.457788351878884,4.01071253147039));
#35874=CARTESIAN_POINT('Ctrl Pts',(14.6882414298876,0.459553790080695,3.93526845476975));
#35875=CARTESIAN_POINT('Ctrl Pts',(14.6803700578377,0.442273111660005,3.85937868713481));
#35876=CARTESIAN_POINT('Ctrl Pts',(14.6724986857877,0.408017034045316,3.79213698410258));
#35877=CARTESIAN_POINT('Ctrl Pts',(14.6646273137378,0.373760956430627,3.72489528107034));
#35878=CARTESIAN_POINT('Ctrl Pts',(14.6567559416878,0.32252947962194,3.6663016426408));
#35879=CARTESIAN_POINT('Ctrl Pts',(14.6488845696379,0.260461593653079,3.6233772554918));
#35880=CARTESIAN_POINT('Ctrl Pts',(14.6410131975879,0.198393707684219,3.5804528683428));
#35881=CARTESIAN_POINT('Ctrl Pts',(14.6331418255379,0.125489412555185,3.55319773247434));
#35882=CARTESIAN_POINT('Ctrl Pts',(14.625270453488,0.0504847191830214,3.54487778940425));
#35883=CARTESIAN_POINT('Ctrl Pts',(14.617399081438,-0.0245199741891427,
3.53655784633416));
#35884=CARTESIAN_POINT('Ctrl Pts',(14.6095277093881,-0.101625065804437,
3.54717309606245));
#35885=CARTESIAN_POINT('Ctrl Pts',(14.6016563373381,-0.171591169681571,
3.57545152934398));
#35886=CARTESIAN_POINT('Ctrl Pts',(14.5937849652882,-0.241557273558703,
3.6037299626255));
#35887=CARTESIAN_POINT('Ctrl Pts',(14.5859135932382,-0.304384389697674,
3.64967157946028));
#35888=CARTESIAN_POINT('Ctrl Pts',(14.5780422211883,-0.352544040227279,
3.70777126570269));
#35889=CARTESIAN_POINT('Ctrl Pts',(14.5701708491383,-0.400703690756885,
3.7658709519451));
#35890=CARTESIAN_POINT('Ctrl Pts',(14.5622994770883,-0.434195875677124,
3.83612870759516));
#35891=CARTESIAN_POINT('Ctrl Pts',(14.5544281050384,-0.449007277354457,
3.91012565253846));
#35892=CARTESIAN_POINT('Ctrl Pts',(14.5465567329884,-0.46381867903179,3.98412259748177));
#35893=CARTESIAN_POINT('Ctrl Pts',(14.5386853609385,-0.459949297466218,
4.06185873171832));
#35894=CARTESIAN_POINT('Ctrl Pts',(14.5308139888885,-0.437862794771992,
4.13401905238929));
#35895=CARTESIAN_POINT('Ctrl Pts',(14.5229426168386,-0.415776292077766,
4.20617937306026));
#35896=CARTESIAN_POINT('Ctrl Pts',(14.5150712447886,-0.375472668254887,
4.27276388016565));
#35897=CARTESIAN_POINT('Ctrl Pts',(14.5071998727387,-0.321781445311454,
4.32579385338299));
#35898=CARTESIAN_POINT('Ctrl Pts',(14.4993285006887,-0.26809022236802,4.37882382660034));
#35899=CARTESIAN_POINT('Ctrl Pts',(14.4914571286387,-0.201011400304033,
4.41829926592964));
#35900=CARTESIAN_POINT('Ctrl Pts',(14.4835857565888,-0.128582932452519,
4.43948988945229));
#35901=CARTESIAN_POINT('Ctrl Pts',(14.4790557405542,-0.0868999680795747,
4.45168520479633));
#35902=CARTESIAN_POINT('Ctrl Pts',(14.4745257245197,-0.0434451672832877,
4.45782447382869));
#35903=CARTESIAN_POINT('Ctrl Pts',(14.4699957084852,4.96934848862042E-6,
4.4578413260902));
#35904=CARTESIAN_POINT('Ctrl Pts',(14.5800042915148,-1.58578451148518E-6,
4.45791318879952));
#35905=CARTESIAN_POINT('Ctrl Pts',(14.5801660092442,-0.00155201715944126,
4.45791349841543));
#35906=CARTESIAN_POINT('Ctrl Pts',(14.5803277269736,-0.00310244544229786,
4.45790578589721));
#35907=CARTESIAN_POINT('Ctrl Pts',(14.5804894447029,-0.0046527920161852,
4.45789003224535));
#35908=CARTESIAN_POINT('Ctrl Pts',(14.5883608167529,-0.0801136257596197,
4.45712324646747));
#35909=CARTESIAN_POINT('Ctrl Pts',(14.5962321888029,-0.155380881795201,
4.43730611368561));
#35910=CARTESIAN_POINT('Ctrl Pts',(14.6041035608528,-0.22143539919095,4.4008132908088));
#35911=CARTESIAN_POINT('Ctrl Pts',(14.6119749329028,-0.287489916586699,
4.36432046793199));
#35912=CARTESIAN_POINT('Ctrl Pts',(14.6198463049527,-0.344331695342615,
4.31115195496024));
#35913=CARTESIAN_POINT('Ctrl Pts',(14.6277176770027,-0.38514947146564,4.24767885402976));
#35914=CARTESIAN_POINT('Ctrl Pts',(14.6355890490526,-0.425967247588666,
4.18420575309928));
#35915=CARTESIAN_POINT('Ctrl Pts',(14.6434604211026,-0.4507610210788,4.11042806421008));
#35916=CARTESIAN_POINT('Ctrl Pts',(14.6513317931525,-0.45655979174196,4.03518645571321));
#35917=CARTESIAN_POINT('Ctrl Pts',(14.6592031652025,-0.462358562405121,
3.95994484721634));
#35918=CARTESIAN_POINT('Ctrl Pts',(14.6670745372524,-0.449162330241309,
3.8832393191118));
#35919=CARTESIAN_POINT('Ctrl Pts',(14.6749459093024,-0.41855237967279,3.81426137832517));
#35920=CARTESIAN_POINT('Ctrl Pts',(14.6828172813524,-0.387942429104271,
3.74528343753854));
#35921=CARTESIAN_POINT('Ctrl Pts',(14.6906886534023,-0.339918760131043,
3.68403308406983));
#35922=CARTESIAN_POINT('Ctrl Pts',(14.6985600254523,-0.280235976103336,
3.63784985464301));
#35923=CARTESIAN_POINT('Ctrl Pts',(14.7064313975022,-0.220553192075631,
3.5916666252162));
#35924=CARTESIAN_POINT('Ctrl Pts',(14.7143027695522,-0.149211292993445,
3.5605505198313));
#35925=CARTESIAN_POINT('Ctrl Pts',(14.7221741416021,-0.0747590701011626,
3.54823013427646));
#35926=CARTESIAN_POINT('Ctrl Pts',(14.7300455136521,-0.000306847208877067,
3.53590974872161));
#35927=CARTESIAN_POINT('Ctrl Pts',(14.737916885702,0.0772556994935079,3.54238508299684));
#35928=CARTESIAN_POINT('Ctrl Pts',(14.745788257752,0.148634367597872,3.5668802073009));
#35929=CARTESIAN_POINT('Ctrl Pts',(14.753659629802,0.220013035702235,3.59137533160497));
#35930=CARTESIAN_POINT('Ctrl Pts',(14.7615310018519,0.285207825208577,3.63389024593787));
#35931=CARTESIAN_POINT('Ctrl Pts',(14.7694023739019,0.336406544142474,3.68933045342307));
#35932=CARTESIAN_POINT('Ctrl Pts',(14.7772737459518,0.387605263076371,3.74477066090827));
#35933=CARTESIAN_POINT('Ctrl Pts',(14.7851451180018,0.424807911437823,3.81313616154577));
#35934=CARTESIAN_POINT('Ctrl Pts',(14.7930164900517,0.443556551112275,3.88623481973509));
#35935=CARTESIAN_POINT('Ctrl Pts',(14.8008878621017,0.462305190786727,3.9593334779244));
#35936=CARTESIAN_POINT('Ctrl Pts',(14.8087592341516,0.462599821774179,4.03716529366552));
#35937=CARTESIAN_POINT('Ctrl Pts',(14.8166306062016,0.444405141642572,4.11040380200553));
#35938=CARTESIAN_POINT('Ctrl Pts',(14.8245019782516,0.426210461510966,4.18364231034555));
#35939=CARTESIAN_POINT('Ctrl Pts',(14.8323733503015,0.389526470260302,4.25228751128446));
#35940=CARTESIAN_POINT('Ctrl Pts',(14.8402447223515,0.338748948932789,4.3081137476731));
#35941=CARTESIAN_POINT('Ctrl Pts',(14.8481160944014,0.287971427605278,4.36393998406173));
#35942=CARTESIAN_POINT('Ctrl Pts',(14.8559874664514,0.22310037620092,4.40694725590009));
#35943=CARTESIAN_POINT('Ctrl Pts',(14.8638588385013,0.151909206873508,4.43198208217373));
#35944=CARTESIAN_POINT('Ctrl Pts',(14.8692406561725,0.103234351881841,4.44909890368578));
#35945=CARTESIAN_POINT('Ctrl Pts',(14.8746224738437,0.0516050086776526,
4.45781408155485));
#35946=CARTESIAN_POINT('Ctrl Pts',(14.8800042915148,-1.01702808208336E-5,
4.45785711824254));
#35947=CARTESIAN_POINT('Origin',(12.5,0.,4.));
#35948=CARTESIAN_POINT('',(15.1,-5.60735153159594E-17,4.457875));
#35949=CARTESIAN_POINT('',(15.0699957084852,-1.05870731373636E-5,4.45788944868556));
#35950=CARTESIAN_POINT('',(12.5,-5.60735153159594E-17,4.457875));
#35951=CARTESIAN_POINT('',(15.1,-0.269165465906718,4.37040446485999));
#35952=CARTESIAN_POINT('Origin',(15.1,0.,4.));
#35953=CARTESIAN_POINT('Ctrl Pts',(15.1,-0.269173508333955,4.37043259773194));
#35954=CARTESIAN_POINT('Ctrl Pts',(15.0991842588284,-0.262849866117432,
4.37503549456412));
#35955=CARTESIAN_POINT('Ctrl Pts',(15.0983685176569,-0.256407545646713,
4.37947450812006));
#35956=CARTESIAN_POINT('Ctrl Pts',(15.0975527764853,-0.249853611926923,
4.38374199825787));
#35957=CARTESIAN_POINT('Ctrl Pts',(15.0896814044354,-0.186612411779406,
4.42492050409441));
#35958=CARTESIAN_POINT('Ctrl Pts',(15.0818100323854,-0.112978907049287,
4.45012847221118));
#35959=CARTESIAN_POINT('Ctrl Pts',(15.0739386603355,-0.0377721395608013,
4.45635245505497));
#35960=CARTESIAN_POINT('Ctrl Pts',(15.072624343052,-0.0252145379490987,
4.45739170058566));
#35961=CARTESIAN_POINT('Ctrl Pts',(15.0713100257686,-0.0126130730861363,
4.45790166433459));
#35962=CARTESIAN_POINT('Ctrl Pts',(15.0699957084852,-1.05870731373636E-5,
4.45788944868556));
#35963=CARTESIAN_POINT('Origin',(11.8752146997001,0.,4.));
#35964=CARTESIAN_POINT('',(14.9247853002999,-1.38824472118437E-5,4.62497559137666));
#35965=CARTESIAN_POINT('',(15.0252146997001,-1.44513692928093E-5,4.62501972247551));
#35966=CARTESIAN_POINT('',(11.8752146997001,-1.68747709936658E-14,4.625));
#35967=CARTESIAN_POINT('',(15.1,-0.624993681275899,4.00281040303151));
#35968=CARTESIAN_POINT('Ctrl Pts',(15.0252146997001,-1.44513692928189E-5,
4.62501972247551));
#35969=CARTESIAN_POINT('Ctrl Pts',(15.0265290169835,-0.017216861979444,
4.62503639685311));
#35970=CARTESIAN_POINT('Ctrl Pts',(15.0357147063169,-0.137433797398843,
4.62017138475037));
#35971=CARTESIAN_POINT('Ctrl Pts',(15.0527717677003,-0.355236031271534,
4.54560815721762));
#35972=CARTESIAN_POINT('Ctrl Pts',(15.0763858838501,-0.571652475026301,
4.31158258982903));
#35973=CARTESIAN_POINT('Ctrl Pts',(15.09212862795,-0.624530364890795,4.10584538053252));
#35974=CARTESIAN_POINT('Ctrl Pts',(15.1,-0.624993681275899,4.00281040303152));
#35975=CARTESIAN_POINT('',(15.1,0.314930721058197,3.46014479632612));
#35976=CARTESIAN_POINT('Origin',(15.1,0.,4.));
#35977=CARTESIAN_POINT('Ctrl Pts',(14.9247853002999,-1.38824472118368E-5,
4.62497559137666));
#35978=CARTESIAN_POINT('Ctrl Pts',(14.9272748546787,-0.0326052931943186,
4.62500276606431));
#35979=CARTESIAN_POINT('Ctrl Pts',(14.9376357811074,-0.168225686180582,
4.61457389311938));
#35980=CARTESIAN_POINT('Ctrl Pts',(14.9558680795861,-0.394527586443172,
4.517903766532));
#35981=CARTESIAN_POINT('Ctrl Pts',(14.979482195736,-0.593077772790822,4.26857965265179));
#35982=CARTESIAN_POINT('Ctrl Pts',(15.0030963118859,-0.649493436571599,
3.95488773069898));
#35983=CARTESIAN_POINT('Ctrl Pts',(15.0267104280357,-0.550252000240565,
3.65200904506483));
#35984=CARTESIAN_POINT('Ctrl Pts',(15.0503245441856,-0.319142060764588,
3.43252503194012));
#35985=CARTESIAN_POINT('Ctrl Pts',(15.0739386603355,-0.0115409051696555,
3.34904846156061));
#35986=CARTESIAN_POINT('Ctrl Pts',(15.0904971456069,0.20608092381284,3.39989411918499));
#35987=CARTESIAN_POINT('Ctrl Pts',(15.0991842588284,0.305720220830039,3.45471854406458));
#35988=CARTESIAN_POINT('Ctrl Pts',(15.1,0.314937815442301,3.46010549098218));
#35989=CARTESIAN_POINT('Origin',(11.8752146997001,0.,4.));
#35990=CARTESIAN_POINT('',(14.6247853002999,-2.16459804047719E-6,4.62505212776347));
#35991=CARTESIAN_POINT('',(14.7252146997001,1.17863019661874E-5,4.62503218402409));
#35992=CARTESIAN_POINT('',(11.8752146997001,-1.68747709936658E-14,4.625));
#35993=CARTESIAN_POINT('Ctrl Pts',(14.7252146997001,1.17863019662174E-5,
4.62503218402409));
#35994=CARTESIAN_POINT('Ctrl Pts',(14.7320725523841,-0.0897427467603322,
4.62495430540108));
#35995=CARTESIAN_POINT('Ctrl Pts',(14.746801777118,-0.282587126126967,4.58296482291278));
#35996=CARTESIAN_POINT('Ctrl Pts',(14.7694023739019,-0.520130285395982,
4.39158760667368));
#35997=CARTESIAN_POINT('Ctrl Pts',(14.7930164900517,-0.64367318065081,4.09778141619902));
#35998=CARTESIAN_POINT('Ctrl Pts',(14.8166306062016,-0.612955311082805,
3.78054123783642));
#35999=CARTESIAN_POINT('Ctrl Pts',(14.8402447223515,-0.435338447621071,
3.51589585985611));
#36000=CARTESIAN_POINT('Ctrl Pts',(14.8638588385013,-0.153389665944836,
3.36726945127358));
#36001=CARTESIAN_POINT('Ctrl Pts',(14.8874729546512,0.165319955489652,3.37028123293502));
#36002=CARTESIAN_POINT('Ctrl Pts',(14.9110870708011,0.444409630539555,3.52420969451069));
#36003=CARTESIAN_POINT('Ctrl Pts',(14.9347011869509,0.616993161964042,3.79216419995926));
#36004=CARTESIAN_POINT('Ctrl Pts',(14.9583153031008,0.641710593195818,4.10992889087348));
#36005=CARTESIAN_POINT('Ctrl Pts',(14.9819294192507,0.512636325700993,4.40134645341462));
#36006=CARTESIAN_POINT('Ctrl Pts',(15.0042292181171,0.274729866520086,4.58571614948967));
#36007=CARTESIAN_POINT('Ctrl Pts',(15.0186576449336,0.0858074045169303,
4.62493653494651));
#36008=CARTESIAN_POINT('Ctrl Pts',(15.0252146997001,-1.44513692928189E-5,
4.62501972247551));
#36009=CARTESIAN_POINT('Ctrl Pts',(14.6247853002999,-2.16459804049194E-6,
4.62505212776347));
#36010=CARTESIAN_POINT('Ctrl Pts',(14.6249470180292,-0.00211850554115318,
4.62505255038961));
#36011=CARTESIAN_POINT('Ctrl Pts',(14.6329801078086,-0.107244412024774,
4.62452960748548));
#36012=CARTESIAN_POINT('Ctrl Pts',(14.6488845696379,-0.314835022974042,
4.56987302880665));
#36013=CARTESIAN_POINT('Ctrl Pts',(14.6724986857877,-0.547602339746838,
4.35214775046202));
#36014=CARTESIAN_POINT('Ctrl Pts',(14.6961128019376,-0.649132943719538,
4.05002781234082));
#36015=CARTESIAN_POINT('Ctrl Pts',(14.7197269180875,-0.595094318970103,
3.73591836064326));
#36016=CARTESIAN_POINT('Ctrl Pts',(14.7433410342373,-0.398437197867616,
3.48509791236843));
#36017=CARTESIAN_POINT('Ctrl Pts',(14.7669551503872,-0.1062918289807,3.35767733339665));
#36018=CARTESIAN_POINT('Ctrl Pts',(14.7905692665371,0.211327117384507,3.38419385377023));
#36019=CARTESIAN_POINT('Ctrl Pts',(14.8141833826869,0.478300047385911,3.5582926020622));
#36020=CARTESIAN_POINT('Ctrl Pts',(14.8377974988368,0.630645044771057,3.83824960712979));
#36021=CARTESIAN_POINT('Ctrl Pts',(14.8614116149867,0.631851559871185,4.15697121131127));
#36022=CARTESIAN_POINT('Ctrl Pts',(14.8850257311365,0.481630465478622,4.4380735902585));
#36023=CARTESIAN_POINT('Ctrl Pts',(14.9061502929076,0.243989509668873,4.59562135563586));
#36024=CARTESIAN_POINT('Ctrl Pts',(14.9194034826287,0.0704409072858971,
4.62491684623921));
#36025=CARTESIAN_POINT('Ctrl Pts',(14.9247853002999,-1.38824472118368E-5,
4.62497559137666));
#36026=CARTESIAN_POINT('Origin',(11.8752146997001,0.,4.));
#36027=CARTESIAN_POINT('',(14.3247853002999,1.51969053300144E-5,4.6249871875462));
#36028=CARTESIAN_POINT('',(14.4252146997001,6.78316748347314E-6,4.62495403506715));
#36029=CARTESIAN_POINT('',(11.8752146997001,-1.68747709936658E-14,4.625));
#36030=CARTESIAN_POINT('Ctrl Pts',(14.4252146997001,6.78316748347826E-6,
4.62495403506715));
#36031=CARTESIAN_POINT('Ctrl Pts',(14.4297447157347,-0.0593027126443913,
4.62493103170719));
#36032=CARTESIAN_POINT('Ctrl Pts',(14.4421461038192,-0.221686029527806,
4.60198961095629));
#36033=CARTESIAN_POINT('Ctrl Pts',(14.4624188639536,-0.457506203155893,
4.46321101183598));
#36034=CARTESIAN_POINT('Ctrl Pts',(14.4860329801035,-0.622549707754089,
4.19054718257559));
#36035=CARTESIAN_POINT('Ctrl Pts',(14.5096470962533,-0.63839484111024,3.87221739454711));
#36036=CARTESIAN_POINT('Ctrl Pts',(14.5332612124032,-0.501244206711231,
3.58451159745434));
#36037=CARTESIAN_POINT('Ctrl Pts',(14.5568753285531,-0.243966908844842,
3.39638048838484));
#36038=CARTESIAN_POINT('Ctrl Pts',(14.5804894447029,0.0717787570654544,
3.35291099727801));
#36039=CARTESIAN_POINT('Ctrl Pts',(14.6041035608528,0.370322144162233,3.46452089026927));
#36040=CARTESIAN_POINT('Ctrl Pts',(14.6277176770027,0.580115251486915,3.70446207957941));
#36041=CARTESIAN_POINT('Ctrl Pts',(14.6513317931525,0.650879700384091,4.0152309888134));
#36042=CARTESIAN_POINT('Ctrl Pts',(14.6749459093024,0.565656298155129,4.32234968564526));
#36043=CARTESIAN_POINT('Ctrl Pts',(14.6985600254523,0.344869426209941,4.55221503612336));
#36044=CARTESIAN_POINT('Ctrl Pts',(14.7153162889182,0.129554394067723,4.62141618582314));
#36045=CARTESIAN_POINT('Ctrl Pts',(14.7242011803341,0.0132765736394338,
4.62504369367533));
#36046=CARTESIAN_POINT('Ctrl Pts',(14.7252146997001,1.17863019662174E-5,
4.62503218402409));
#36047=CARTESIAN_POINT('Ctrl Pts',(14.3247853002999,1.51969053300109E-5,
4.6249871875462));
#36048=CARTESIAN_POINT('Ctrl Pts',(14.3304905534298,-0.0746697890657793,
4.62491698721088));
#36049=CARTESIAN_POINT('Ctrl Pts',(14.3440671786096,-0.252453835406249,
4.59302599116618));
#36050=CARTESIAN_POINT('Ctrl Pts',(14.3655151758395,-0.490432948250941,
4.42819608115853));
#36051=CARTESIAN_POINT('Ctrl Pts',(14.3891292919893,-0.634910852255616,
4.14409916841427));
#36052=CARTESIAN_POINT('Ctrl Pts',(14.4127434081392,-0.627227950688033,
3.82546788683648));
#36053=CARTESIAN_POINT('Ctrl Pts',(14.4363575242891,-0.469225504392149,
3.54866444115539));
#36054=CARTESIAN_POINT('Ctrl Pts',(14.4599716404389,-0.198769899531221,
3.38002670405092));
#36055=CARTESIAN_POINT('Ctrl Pts',(14.4835857565888,0.11932229545683,3.35996988316441));
#36056=CARTESIAN_POINT('Ctrl Pts',(14.5071998727387,0.408818071695872,3.49330073524378));
#36057=CARTESIAN_POINT('Ctrl Pts',(14.5308139888885,0.600337751131954,3.74806559342675));
#36058=CARTESIAN_POINT('Ctrl Pts',(14.5544281050384,0.647982309355475,4.06320828594604));
#36059=CARTESIAN_POINT('Ctrl Pts',(14.5780422211883,0.540333396317157,4.36320267272319));
#36060=CARTESIAN_POINT('Ctrl Pts',(14.6014946196088,0.304813865567294,4.57469465218781));
#36061=CARTESIAN_POINT('Ctrl Pts',(14.6170756459793,0.100891269655612,4.62503197968527));
#36062=CARTESIAN_POINT('Ctrl Pts',(14.6247853002999,-2.16459804049194E-6,
4.62505212776347));
#36063=CARTESIAN_POINT('Origin',(11.8752146997001,0.,4.));
#36064=CARTESIAN_POINT('',(14.0247853002999,-6.3966029390794E-6,4.62495348172753));
#36065=CARTESIAN_POINT('',(14.1252146997001,-1.50974863142078E-5,4.62498583382255));
#36066=CARTESIAN_POINT('',(11.8752146997001,-1.68747709936658E-14,4.625));
#36067=CARTESIAN_POINT('Ctrl Pts',(14.1252146997001,-1.50974863141889E-5,
4.62498583382255));
#36068=CARTESIAN_POINT('Ctrl Pts',(14.1274168790852,-0.0288430498503269,
4.62501265364587));
#36069=CARTESIAN_POINT('Ctrl Pts',(14.1374904305203,-0.160695812902997,
4.61605202430223));
#36070=CARTESIAN_POINT('Ctrl Pts',(14.1554353540053,-0.385112282251534,
4.52494275637564));
#36071=CARTESIAN_POINT('Ctrl Pts',(14.1790494701552,-0.588131968915973,
4.27924389796604));
#36072=CARTESIAN_POINT('Ctrl Pts',(14.2026635863051,-0.65020173504413,3.96662229549764));
#36073=CARTESIAN_POINT('Ctrl Pts',(14.2262777024549,-0.556446129094758,
3.66199989226673));
#36074=CARTESIAN_POINT('Ctrl Pts',(14.2498918186048,-0.329334334698108,
3.43838156778717));
#36075=CARTESIAN_POINT('Ctrl Pts',(14.2735059347547,-0.0232952743833569,
3.34935901020328));
#36076=CARTESIAN_POINT('Ctrl Pts',(14.2971200509045,0.28832666060365,3.41626709515619));
#36077=CARTESIAN_POINT('Ctrl Pts',(14.3207341670544,0.530849104237583,3.62307083431711));
#36078=CARTESIAN_POINT('Ctrl Pts',(14.3443482832043,0.646149864620809,3.92020827196535));
#36079=CARTESIAN_POINT('Ctrl Pts',(14.3679623993541,0.606596311879891,4.2364683526943));
#36080=CARTESIAN_POINT('Ctrl Pts',(14.391576515504,0.42166773027486,4.49605714656388));
#36081=CARTESIAN_POINT('Ctrl Pts',(14.4106606156193,0.190545343529355,4.60977018898031));
#36082=CARTESIAN_POINT('Ctrl Pts',(14.4218733436847,0.0437536792250838,
4.62497100242767));
#36083=CARTESIAN_POINT('Ctrl Pts',(14.4252146997001,6.78316748347826E-6,
4.62495403506715));
#36084=CARTESIAN_POINT('Ctrl Pts',(14.0247853002999,-6.39660293913491E-6,
4.62495348172753));
#36085=CARTESIAN_POINT('Ctrl Pts',(14.0281627167804,-0.0442255271350925,
4.62496963662755));
#36086=CARTESIAN_POINT('Ctrl Pts',(14.0394115053108,-0.191490205391595,
4.6095527480466));
#36087=CARTESIAN_POINT('Ctrl Pts',(14.0585316658912,-0.422790583021024,
4.49510047824495));
#36088=CARTESIAN_POINT('Ctrl Pts',(14.0821457820411,-0.60713052675338,4.23509335195577));
#36089=CARTESIAN_POINT('Ctrl Pts',(14.1057598981909,-0.645967413308333,
3.91874446730605));
#36090=CARTESIAN_POINT('Ctrl Pts',(14.1293740143408,-0.529993712466286,
3.62186903671368));
#36091=CARTESIAN_POINT('Ctrl Pts',(14.1529881304907,-0.287003328966194,
3.41561532377041));
#36092=CARTESIAN_POINT('Ctrl Pts',(14.1766022466405,0.0247694002478971,
3.34941346658496));
#36093=CARTESIAN_POINT('Ctrl Pts',(14.2002163627904,0.330605970264406,3.43912920108534));
#36094=CARTESIAN_POINT('Ctrl Pts',(14.2238304789403,0.557210518047066,3.66326152695696));
#36095=CARTESIAN_POINT('Ctrl Pts',(14.2474445950901,0.650275686248857,3.96809557204375));
#36096=CARTESIAN_POINT('Ctrl Pts',(14.27105871124,0.587497759452106,4.28057573538778));
#36097=CARTESIAN_POINT('Ctrl Pts',(14.2946728273899,0.383921904832036,4.52581397056352));
#36098=CARTESIAN_POINT('Ctrl Pts',(14.3125816904098,0.159750963363977,4.61623247111552));
#36099=CARTESIAN_POINT('Ctrl Pts',(14.3226191813798,0.0283709170587055,
4.62501384057475));
#36100=CARTESIAN_POINT('Ctrl Pts',(14.3247853002999,1.51969053300109E-5,
4.6249871875462));
#36101=CARTESIAN_POINT('Origin',(11.8752146997001,0.,4.));
#36102=CARTESIAN_POINT('',(13.7247853002999,-1.20831421157597E-5,4.62503091248755));
#36103=CARTESIAN_POINT('',(13.8252146997001,1.68461488569462E-6,4.62505238998457));
#36104=CARTESIAN_POINT('',(11.8752146997001,-1.68747709936658E-14,4.625));
#36105=CARTESIAN_POINT('Ctrl Pts',(13.8252146997001,1.68461488569581E-6,
4.62505238998457));
#36106=CARTESIAN_POINT('Ctrl Pts',(13.8329604144858,-0.101363538932993,
4.62503644193381));
#36107=CARTESIAN_POINT('Ctrl Pts',(13.8485775013214,-0.305753798836605,
4.57432856173903));
#36108=CARTESIAN_POINT('Ctrl Pts',(13.8720659602069,-0.541154937947787,
4.36197748624323));
#36109=CARTESIAN_POINT('Ctrl Pts',(13.8956800763568,-0.648123865072376,
4.06173996222779));
#36110=CARTESIAN_POINT('Ctrl Pts',(13.9192941925067,-0.599765396122921,
3.74670602647169));
#36111=CARTESIAN_POINT('Ctrl Pts',(13.9429083086565,-0.407668974822819,
3.49237575473668));
#36112=CARTESIAN_POINT('Ctrl Pts',(13.9665224248064,-0.117871845784803,
3.35970116712309));
#36113=CARTESIAN_POINT('Ctrl Pts',(13.9901365409563,0.200174091641329,3.38047865214521));
#36114=CARTESIAN_POINT('Ctrl Pts',(14.0137506571061,0.470246914526057,3.54972874087838));
#36115=CARTESIAN_POINT('Ctrl Pts',(14.037364773256,0.627621790796785,3.82688947135059));
#36116=CARTESIAN_POINT('Ctrl Pts',(14.0609788894059,0.634582735815489,4.14553734509456));
#36117=CARTESIAN_POINT('Ctrl Pts',(14.0845930055557,0.489461510650943,4.42930618095194));
#36118=CARTESIAN_POINT('Ctrl Pts',(14.1060049423205,0.251510284961593,4.59332024860173));
#36119=CARTESIAN_POINT('Ctrl Pts',(14.1195455070353,0.074198300926532,4.62491679006221));
#36120=CARTESIAN_POINT('Ctrl Pts',(14.1252146997001,-1.50974863141889E-5,
4.62498583382255));
#36121=CARTESIAN_POINT('Ctrl Pts',(13.7247853002999,-1.20831421156938E-5,
4.62503091248755));
#36122=CARTESIAN_POINT('Ctrl Pts',(13.7258348801309,-0.013748904810447,
4.62504304225186));
#36123=CARTESIAN_POINT('Ctrl Pts',(13.734755832012,-0.130498998332177,4.62127102305724));
#36124=CARTESIAN_POINT('Ctrl Pts',(13.7515481559429,-0.346119716157775,
4.55143222859795));
#36125=CARTESIAN_POINT('Ctrl Pts',(13.7751622720928,-0.566385203513325,
4.32106722332061));
#36126=CARTESIAN_POINT('Ctrl Pts',(13.7987763882427,-0.650912534047929,
4.01375622291695));
#36127=CARTESIAN_POINT('Ctrl Pts',(13.8223905043925,-0.57944414457563,3.70314844792952));
#36128=CARTESIAN_POINT('Ctrl Pts',(13.8460046205424,-0.369107932149097,
3.46368321387984));
#36129=CARTESIAN_POINT('Ctrl Pts',(13.8696187366923,-0.0703124342978696,
3.35275003110641));
#36130=CARTESIAN_POINT('Ctrl Pts',(13.8932328528421,0.245333927901481,3.3969348091043));
#36131=CARTESIAN_POINT('Ctrl Pts',(13.916846968992,0.502184306426786,3.58564835824111));
#36132=CARTESIAN_POINT('Ctrl Pts',(13.9404610851419,0.638682720042094,3.87366416276737));
#36133=CARTESIAN_POINT('Ctrl Pts',(13.9640752012917,0.62211637371287,4.19195723015293));
#36134=CARTESIAN_POINT('Ctrl Pts',(13.9876893174416,0.456455507660852,4.46424641105313));
#36135=CARTESIAN_POINT('Ctrl Pts',(14.007926017111,0.220741531225703,4.60224444133776));
#36136=CARTESIAN_POINT('Ctrl Pts',(14.0202913447304,0.058831122868106,4.62493198618401));
#36137=CARTESIAN_POINT('Ctrl Pts',(14.0247853002999,-6.39660293913491E-6,
4.62495348172753));
#36138=CARTESIAN_POINT('Origin',(11.8752146997001,0.,4.));
#36139=CARTESIAN_POINT('',(13.4247853002999,1.36962628664028E-5,4.62502243215823));
#36140=CARTESIAN_POINT('',(13.5252146997001,1.40828270379035E-5,4.62497680637469));
#36141=CARTESIAN_POINT('',(11.8752146997001,-1.68747709936658E-14,4.625));
#36142=CARTESIAN_POINT('Ctrl Pts',(13.5252146997001,1.4082827037902E-5,
4.62497680637469));
#36143=CARTESIAN_POINT('Ctrl Pts',(13.5306325778363,-0.0709123884867814,
4.62491668074428));
#36144=CARTESIAN_POINT('Ctrl Pts',(13.5439218280225,-0.244933372371362,
4.59533688876844));
#36145=CARTESIAN_POINT('Ctrl Pts',(13.5650824502587,-0.482621788093898,
4.43698120905743));
#36146=CARTESIAN_POINT('Ctrl Pts',(13.5886965664085,-0.632205603168059,
4.15553919999523));
#36147=CARTESIAN_POINT('Ctrl Pts',(13.6123106825584,-0.630276944445953,
3.83682113889318));
#36148=CARTESIAN_POINT('Ctrl Pts',(13.6359247987083,-0.477298028416376,
3.55721002779864));
#36149=CARTESIAN_POINT('Ctrl Pts',(13.6595389148582,-0.209931317243796,
3.38371661595291));
#36150=CARTESIAN_POINT('Ctrl Pts',(13.683153031008,0.107746895509167,3.35791980725116));
#36151=CARTESIAN_POINT('Ctrl Pts',(13.7067671471579,0.399602814690774,3.48600198647908));
#36152=CARTESIAN_POINT('Ctrl Pts',(13.7303812633077,0.59569113756138,3.73726736776131));
#36153=CARTESIAN_POINT('Ctrl Pts',(13.7539953794576,0.649017932507905,4.05149845333026));
#36154=CARTESIAN_POINT('Ctrl Pts',(13.7776094956075,0.546803061895555,4.35338757606046));
#36155=CARTESIAN_POINT('Ctrl Pts',(13.8012236117573,0.313543031018869,4.57058490613733));
#36156=CARTESIAN_POINT('Ctrl Pts',(13.8170920131216,0.106300066848774,4.6246481407235));
#36157=CARTESIAN_POINT('Ctrl Pts',(13.8250890424358,0.00164611344283092,
4.62505264870678));
#36158=CARTESIAN_POINT('Ctrl Pts',(13.8252146997001,1.68461488569581E-6,
4.62505238998457));
#36159=CARTESIAN_POINT('Ctrl Pts',(13.4247853002999,1.36962628664097E-5,
4.62502243215823));
#36160=CARTESIAN_POINT('Ctrl Pts',(13.4313784155315,-0.086279884022628,
4.62493973056585));
#36161=CARTESIAN_POINT('Ctrl Pts',(13.445842902813,-0.275670893367246,4.58538934244717));
#36162=CARTESIAN_POINT('Ctrl Pts',(13.4681787621445,-0.513544980480383,
4.40018484937968));
#36163=CARTESIAN_POINT('Ctrl Pts',(13.4917928782944,-0.64195771209056,4.10847422061066));
#36164=CARTESIAN_POINT('Ctrl Pts',(13.5154069944443,-0.616520809113462,
3.79076698974655));
#36165=CARTESIAN_POINT('Ctrl Pts',(13.5390211105941,-0.443330402422436,
3.52320390633144));
#36166=CARTESIAN_POINT('Ctrl Pts',(13.562635226744,-0.163892778617988,3.36990832590288));
#36167=CARTESIAN_POINT('Ctrl Pts',(13.5862493428939,0.154822890495328,3.36761860145296));
#36168=CARTESIAN_POINT('Ctrl Pts',(13.6098634590437,0.43643417612693,3.51688348138565));
#36169=CARTESIAN_POINT('Ctrl Pts',(13.6334775751936,0.613450973283793,3.78193059814177));
#36170=CARTESIAN_POINT('Ctrl Pts',(13.6570916913435,0.643449974253473,4.09923956510808));
#36171=CARTESIAN_POINT('Ctrl Pts',(13.6807058074933,0.519241709620395,4.39276507945606));
#36172=CARTESIAN_POINT('Ctrl Pts',(13.7032703438121,0.281645253009076,4.58329909926801));
#36173=CARTESIAN_POINT('Ctrl Pts',(13.717963508081,0.0892710189108511,4.62495207452848));
#36174=CARTESIAN_POINT('Ctrl Pts',(13.7247853002999,-1.20831421156938E-5,
4.62503091248755));
#36175=CARTESIAN_POINT('Origin',(11.8752146997001,0.,4.));
#36176=CARTESIAN_POINT('',(13.1247853002999,3.84888821539087E-6,4.62495078081483));
#36177=CARTESIAN_POINT('',(13.2252146997001,-9.32440196476731E-6,4.62495874418382));
#36178=CARTESIAN_POINT('',(11.8752146997001,-1.68747709936658E-14,4.625));
#36179=CARTESIAN_POINT('Ctrl Pts',(13.2252146997001,-9.32440196474427E-6,
4.62495874418382));
#36180=CARTESIAN_POINT('Ctrl Pts',(13.2283047411869,-0.040464997295585,
4.62498052751194));
#36181=CARTESIAN_POINT('Ctrl Pts',(13.2392661547237,-0.18396024524725,4.61125364372682));
#36182=CARTESIAN_POINT('Ctrl Pts',(13.2580989403104,-0.413782468289504,
4.50265339583901));
#36183=CARTESIAN_POINT('Ctrl Pts',(13.2817130564603,-0.602786876612853,
4.24601696851145));
#36184=CARTESIAN_POINT('Ctrl Pts',(13.3053271726101,-0.647329213752593,
3.9304208620728));
#36185=CARTESIAN_POINT('Ctrl Pts',(13.32894128876,-0.536734598538914,3.6314998804023));
#36186=CARTESIAN_POINT('Ctrl Pts',(13.3525554049099,-0.297507800394296,
3.42089251764738));
#36187=CARTESIAN_POINT('Ctrl Pts',(13.3761695210598,0.0130188131672444,
3.34907229440132));
#36188=CARTESIAN_POINT('Ctrl Pts',(13.3997836372096,0.320425377524893,3.43325142712992));
#36189=CARTESIAN_POINT('Ctrl Pts',(13.4233977533595,0.551039769569266,3.65325580067535));
#36190=CARTESIAN_POINT('Ctrl Pts',(13.4470118695093,0.649593644862141,3.95635983539258));
#36191=CARTESIAN_POINT('Ctrl Pts',(13.4706259856592,0.592467881122722,4.26992253935193));
#36192=CARTESIAN_POINT('Ctrl Pts',(13.4942401018091,0.393353065302923,4.5187964277335));
#36193=CARTESIAN_POINT('Ctrl Pts',(13.5124363398227,0.1672808180195,4.61476328251587));
#36194=CARTESIAN_POINT('Ctrl Pts',(13.5227612057864,0.0321332374692893,
4.62500403435298));
#36195=CARTESIAN_POINT('Ctrl Pts',(13.5252146997001,1.4082827037902E-5,
4.62497680637469));
#36196=CARTESIAN_POINT('Ctrl Pts',(13.1247853002999,3.84888821536311E-6,
4.62495078081483));
#36197=CARTESIAN_POINT('Ctrl Pts',(13.1290505788821,-0.0558403875021823,
4.6249385719914));
#36198=CARTESIAN_POINT('Ctrl Pts',(13.1411872295142,-0.214751600407627,
4.60383286368317));
#36199=CARTESIAN_POINT('Ctrl Pts',(13.1611952521963,-0.449738236712957,
4.47075670902068));
#36200=CARTESIAN_POINT('Ctrl Pts',(13.1848093683461,-0.619294173608025,
4.2008758003961));
#36201=CARTESIAN_POINT('Ctrl Pts',(13.208423484496,-0.64043195068177,3.88285360784221));
#36202=CARTESIAN_POINT('Ctrl Pts',(13.2320376006459,-0.508085752511173,
3.59290636366459));
#36203=CARTESIAN_POINT('Ctrl Pts',(13.2556517167957,-0.253973266794505,
3.40052194335125));
#36204=CARTESIAN_POINT('Ctrl Pts',(13.2792658329456,0.0610056803032868,
3.3518066124833));
#36205=CARTESIAN_POINT('Ctrl Pts',(13.3028799490955,0.361364191435218,3.45843533922715));
#36206=CARTESIAN_POINT('Ctrl Pts',(13.3264940652453,0.575119258511334,3.69485380694));
#36207=CARTESIAN_POINT('Ctrl Pts',(13.3501081813952,0.65104299168552,4.00440268404554));
#36208=CARTESIAN_POINT('Ctrl Pts',(13.3737222975451,0.570939739771795,4.31289642727099));
#36209=CARTESIAN_POINT('Ctrl Pts',(13.3973364136949,0.354006804717113,4.54640236352309));
#36210=CARTESIAN_POINT('Ctrl Pts',(13.4143574146132,0.136489422610972,4.62032507485564));
#36211=CARTESIAN_POINT('Ctrl Pts',(13.4235070434815,0.0167440814458925,
4.62503846613771));
#36212=CARTESIAN_POINT('Ctrl Pts',(13.4247853002999,1.36962628664097E-5,
4.62502243215823));
#36213=CARTESIAN_POINT('Origin',(11.8752146997001,0.,4.));
#36214=CARTESIAN_POINT('',(12.8247853002999,-1.55438223423121E-5,4.62499607812274));
#36215=CARTESIAN_POINT('',(12.9252146997001,-9.4222586321007E-6,4.62504029123831));
#36216=CARTESIAN_POINT('',(11.8752146997001,-1.68747709936658E-14,4.625));
#36217=CARTESIAN_POINT('Ctrl Pts',(12.9252146997001,-9.42225863212465E-6,
4.62504029123832));
#36218=CARTESIAN_POINT('Ctrl Pts',(12.9259769045375,-0.00998466834883174,
4.6250476064301));
#36219=CARTESIAN_POINT('Ctrl Pts',(12.9346104814248,-0.122971475467856,
4.62239759066569));
#36220=CARTESIAN_POINT('Ctrl Pts',(12.9511154303622,-0.336107011072318,
4.55759164674784));
#36221=CARTESIAN_POINT('Ctrl Pts',(12.974729546512,-0.56049590900091,4.33124115596169));
#36222=CARTESIAN_POINT('Ctrl Pts',(12.9983436626619,-0.650558060547343,
4.02550641626558));
#36223=CARTESIAN_POINT('Ctrl Pts',(13.0219577788117,-0.584709444123524,
3.71365888635357));
#36224=CARTESIAN_POINT('Ctrl Pts',(13.0455718949616,-0.378731139057797,
3.47043499764384));
#36225=CARTESIAN_POINT('Ctrl Pts',(13.0691860111115,-0.0819872800401352,
3.35412504823007));
#36226=CARTESIAN_POINT('Ctrl Pts',(13.0928001272613,0.234405401379786,3.39260352716186));
#36227=CARTESIAN_POINT('Ctrl Pts',(13.1164142434112,0.494621196584012,3.57664879910166));
#36228=CARTESIAN_POINT('Ctrl Pts',(13.1400283595611,0.636297578801308,3.86215313342763));
#36229=CARTESIAN_POINT('Ctrl Pts',(13.1636424757109,0.625480816776257,4.18069342892634));
#36230=CARTESIAN_POINT('Ctrl Pts',(13.1872565918608,0.464763222827219,4.45592928631477));
#36231=CARTESIAN_POINT('Ctrl Pts',(13.2077806665239,0.228267895462889,4.60018049807294));
#36232=CARTESIAN_POINT('Ctrl Pts',(13.220433369137,0.0625891701764018,4.62492503806923));
#36233=CARTESIAN_POINT('Ctrl Pts',(13.2252146997001,-9.32440196474427E-6,
4.62495874418382));
#36234=CARTESIAN_POINT('Ctrl Pts',(12.8247853002999,-1.55438223423052E-5,
4.62499607812274));
#36235=CARTESIAN_POINT('Ctrl Pts',(12.8267227422326,-0.0253767156259869,
4.62502109614712));
#36236=CARTESIAN_POINT('Ctrl Pts',(12.8365315562153,-0.153759343851268,
4.61735081595804));
#36237=CARTESIAN_POINT('Ctrl Pts',(12.854211742248,-0.376327535803878,4.5312757721487));
#36238=CARTESIAN_POINT('Ctrl Pts',(12.8778258583979,-0.583405888470749,
4.28898776831928));
#36239=CARTESIAN_POINT('Ctrl Pts',(12.9014399745477,-0.650666957548692,
3.97744183415536));
#36240=CARTESIAN_POINT('Ctrl Pts',(12.9250540906976,-0.561991161265395,
3.67130212143154));
#36241=CARTESIAN_POINT('Ctrl Pts',(12.9486682068475,-0.338630270727757,
3.44393714350224));
#36242=CARTESIAN_POINT('Ctrl Pts',(12.9722823229973,-0.0341142786054444,
3.34983650006563));
#36243=CARTESIAN_POINT('Ctrl Pts',(12.9958964391472,0.278577437919422,3.41155206540036));
#36244=CARTESIAN_POINT('Ctrl Pts',(13.0195105552971,0.524506132150044,3.61429327464512));
#36245=CARTESIAN_POINT('Ctrl Pts',(13.0431246714469,0.644733280558021,3.90947178565704));
#36246=CARTESIAN_POINT('Ctrl Pts',(13.0667387875968,0.61044561006836,4.22634601343335));
#36247=CARTESIAN_POINT('Ctrl Pts',(13.0903529037467,0.429860399609997,4.4889748434194));
#36248=CARTESIAN_POINT('Ctrl Pts',(13.1097017413144,0.197481915229314,4.60814700801091));
#36249=CARTESIAN_POINT('Ctrl Pts',(13.1211792068321,0.0472175377905832,
4.6249611028038));
#36250=CARTESIAN_POINT('Ctrl Pts',(13.1247853002999,3.84888821536311E-6,
4.62495078081483));
#36251=CARTESIAN_POINT('Origin',(11.8752146997001,0.,4.));
#36252=CARTESIAN_POINT('',(12.5247853002999,3.80998376854277E-6,4.62503871776264));
#36253=CARTESIAN_POINT('',(12.6252146997001,1.49489494596481E-5,4.6250110476872));
#36254=CARTESIAN_POINT('',(11.8752146997001,-1.68747709936658E-14,4.625));
#36255=CARTESIAN_POINT('',(12.5,0.310062960217711,4.54266560670548));
#36256=CARTESIAN_POINT('Ctrl Pts',(12.5,0.310062960217722,4.54266560670548));
#36257=CARTESIAN_POINT('Ctrl Pts',(12.50787137205,0.220600394030941,4.59378185169648));
#36258=CARTESIAN_POINT('Ctrl Pts',(12.5161331388166,0.113220056708515,4.6237347594226));
#36259=CARTESIAN_POINT('Ctrl Pts',(12.5243949055832,0.00511234815255113,
4.6250406321328));
#36260=CARTESIAN_POINT('Ctrl Pts',(12.5247853002999,3.80998376856706E-6,
4.62503871776264));
#36261=CARTESIAN_POINT('',(12.5,0.310062960217774,3.45733439329455));
#36262=CARTESIAN_POINT('Origin',(12.5,0.,4.));
#36263=CARTESIAN_POINT('Ctrl Pts',(12.5,0.310093463203755,3.45730861053195));
#36264=CARTESIAN_POINT('Ctrl Pts',(12.5008157411716,0.319367492808711,3.46259780682489));
#36265=CARTESIAN_POINT('Ctrl Pts',(12.5095028543931,0.416666480413896,3.52147574364868));
#36266=CARTESIAN_POINT('Ctrl Pts',(12.5260613396645,0.569511032758309,3.68451895614546));
#36267=CARTESIAN_POINT('Ctrl Pts',(12.5496754558144,0.651018771792273,3.99264764559437));
#36268=CARTESIAN_POINT('Ctrl Pts',(12.5732895719643,0.576495013506714,4.3025367374363));
#36269=CARTESIAN_POINT('Ctrl Pts',(12.5969036881141,0.363815091701307,4.53992168461618));
#36270=CARTESIAN_POINT('Ctrl Pts',(12.6142120640261,0.144017971622128,4.61907377583531));
#36271=CARTESIAN_POINT('Ctrl Pts',(12.6236490678881,0.0205077016108913,
4.62503160004571));
#36272=CARTESIAN_POINT('Ctrl Pts',(12.6252146997001,1.49489494596471E-5,
4.6250110476872));
#36273=CARTESIAN_POINT('Origin',(11.8752146997001,0.,4.));
#36274=CARTESIAN_POINT('Ctrl Pts',(12.6252146997001,1.49489494596471E-5,
4.6250110476872));
#36275=CARTESIAN_POINT('Ctrl Pts',(12.631520439938,-0.0825216819810338,
4.62492827098767));
#36276=CARTESIAN_POINT('Ctrl Pts',(12.6456975522259,-0.268159494659544,
4.5879440580038));
#36277=CARTESIAN_POINT('Ctrl Pts',(12.6677460365637,-0.506235857616531,
4.40939182910775));
#36278=CARTESIAN_POINT('Ctrl Pts',(12.6913601527136,-0.639894509617229,
4.12004729681268));
#36279=CARTESIAN_POINT('Ctrl Pts',(12.7149742688635,-0.620198095551099,
3.8019325752266));
#36280=CARTESIAN_POINT('Ctrl Pts',(12.7385883850133,-0.451866840211785,
3.53128609963859));
#36281=CARTESIAN_POINT('Ctrl Pts',(12.7622025011632,-0.17524257447904,3.37297016902465));
#36282=CARTESIAN_POINT('Ctrl Pts',(12.7858166173131,0.143379805101228,3.36492630429559));
#36283=CARTESIAN_POINT('Ctrl Pts',(12.809430733463,0.42764021116234,3.50908227080648));
#36284=CARTESIAN_POINT('Ctrl Pts',(12.8330448496128,0.609413666055986,3.77089008898231));
#36285=CARTESIAN_POINT('Ctrl Pts',(12.8566589657627,0.645136892431096,4.08760569204938));
#36286=CARTESIAN_POINT('Ctrl Pts',(12.8802730819125,0.526248572038732,4.38332598125533));
#36287=CARTESIAN_POINT('Ctrl Pts',(12.903124993225,0.289149347937084,4.5805996458561));
#36288=CARTESIAN_POINT('Ctrl Pts',(12.9181055324875,0.0930307802739178,
4.62497206165088));
#36289=CARTESIAN_POINT('Ctrl Pts',(12.9252146997001,-9.42225863212465E-6,
4.62504029123832));
#36290=CARTESIAN_POINT('Ctrl Pts',(12.5247853002999,3.80998376856706E-6,
4.62503871776264));
#36291=CARTESIAN_POINT('Ctrl Pts',(12.5322662776332,-0.0978890574527522,
4.62500203345524));
#36292=CARTESIAN_POINT('Ctrl Pts',(12.5476186270164,-0.298862923743373,
4.57698368148067));
#36293=CARTESIAN_POINT('Ctrl Pts',(12.5708423484496,-0.535054221536356,
4.37092866956447));
#36294=CARTESIAN_POINT('Ctrl Pts',(12.5944564645995,-0.647009713430093,
4.07251155115386));
#36295=CARTESIAN_POINT('Ctrl Pts',(12.6180705807493,-0.603894380709874,
3.75671714932517));
#36296=CARTESIAN_POINT('Ctrl Pts',(12.6416846968992,-0.416056506175611,
3.49922677321964));
#36297=CARTESIAN_POINT('Ctrl Pts',(12.6652988130491,-0.128505496873939,
3.36175035317655));
#36298=CARTESIAN_POINT('Ctrl Pts',(12.6889129291989,0.189841674427298,3.37723482234205));
#36299=CARTESIAN_POINT('Ctrl Pts',(12.7125270453488,0.462692468193658,3.54196933898577));
#36300=CARTESIAN_POINT('Ctrl Pts',(12.7361411614987,0.624655556881011,3.81647407445394));
#36301=CARTESIAN_POINT('Ctrl Pts',(12.7597552776485,0.636915702199809,4.13496208375113));
#36302=CARTESIAN_POINT('Ctrl Pts',(12.7833693937984,0.496534514683115,4.42110548633398));
#36303=CARTESIAN_POINT('Ctrl Pts',(12.8050460680155,0.258436396781676,4.5911312751119));
#36304=CARTESIAN_POINT('Ctrl Pts',(12.8188513701827,0.0776597756952025,
4.62491945378327));
#36305=CARTESIAN_POINT('Ctrl Pts',(12.8247853002999,-1.55438223423052E-5,
4.62499607812274));
#36306=CARTESIAN_POINT('Ctrl Pts',(12.5,-0.186196943290592,3.58169363627332));
#36307=CARTESIAN_POINT('Ctrl Pts',(12.50787137205,-0.117235947257613,3.55099764935784));
#36308=CARTESIAN_POINT('Ctrl Pts',(12.5236141161499,0.0360970477778841,
3.52440632583991));
#36309=CARTESIAN_POINT('Ctrl Pts',(12.5472282322997,0.257537368848111,3.59853698535937));
#36310=CARTESIAN_POINT('Ctrl Pts',(12.5708423484496,0.417223782598737,3.76887858727216));
#36311=CARTESIAN_POINT('Ctrl Pts',(12.5944564645995,0.476936352215019,3.99461366516243));
#36312=CARTESIAN_POINT('Ctrl Pts',(12.6180705807493,0.422340246895018,4.22163841384584));
#36313=CARTESIAN_POINT('Ctrl Pts',(12.6416846968992,0.266530936180377,4.39554662614981));
#36314=CARTESIAN_POINT('Ctrl Pts',(12.6652988130491,0.0468439715927196,
4.47465904879863));
#36315=CARTESIAN_POINT('Ctrl Pts',(12.6889129291989,-0.184068700558194,
4.44001626345752));
#36316=CARTESIAN_POINT('Ctrl Pts',(12.7125270453488,-0.37086838928987,4.29992045400434));
#36317=CARTESIAN_POINT('Ctrl Pts',(12.7361411614987,-0.468786717745582,
4.08794664964497));
#36318=CARTESIAN_POINT('Ctrl Pts',(12.7597552776485,-0.454357124800734,
3.85489580461101));
#36319=CARTESIAN_POINT('Ctrl Pts',(12.7833693937984,-0.331037647139153,
3.65662019659523));
#36320=CARTESIAN_POINT('Ctrl Pts',(12.8069835099483,-0.128382710063344,
3.54063794582746));
#36321=CARTESIAN_POINT('Ctrl Pts',(12.8305976260981,0.10504004521716,3.53474501052695));
#36322=CARTESIAN_POINT('Ctrl Pts',(12.854211742248,0.31328921869753,3.64035367159283));
#36323=CARTESIAN_POINT('Ctrl Pts',(12.8778258583979,0.446456451752615,3.83215407918844));
#36324=CARTESIAN_POINT('Ctrl Pts',(12.9014399745477,0.47262728739502,4.06417992999538));
#36325=CARTESIAN_POINT('Ctrl Pts',(12.9250540906976,0.385529703875575,4.28082461386765));
#36326=CARTESIAN_POINT('Ctrl Pts',(12.9486682068475,0.206037242841946,4.43016772408018));
#36327=CARTESIAN_POINT('Ctrl Pts',(12.9722823229973,-0.0228334776507366,
4.47641814468844));
#36328=CARTESIAN_POINT('Ctrl Pts',(12.9958964391472,-0.24623199631158,4.40849164040747));
#36329=CARTESIAN_POINT('Ctrl Pts',(13.0195105552971,-0.410619302934066,
4.24266727085754));
#36330=CARTESIAN_POINT('Ctrl Pts',(13.0431246714469,-0.476598835156983,
4.01868600055616));
#36331=CARTESIAN_POINT('Ctrl Pts',(13.0667387875968,-0.428358138764893,
3.79022650014263));
#36332=CARTESIAN_POINT('Ctrl Pts',(13.0903529037467,-0.277458432473742,
3.61204067927388));
#36333=CARTESIAN_POINT('Ctrl Pts',(13.1139670198965,-0.060063881357403,
3.52683201033335));
#36334=CARTESIAN_POINT('Ctrl Pts',(13.1375811360464,0.171725397050831,3.55502134399878));
#36335=CARTESIAN_POINT('Ctrl Pts',(13.1611952521963,0.362359488617447,3.68985291022187));
#36336=CARTESIAN_POINT('Ctrl Pts',(13.1848093683461,0.466151606229838,3.89901338554908));
#36337=CARTESIAN_POINT('Ctrl Pts',(13.208423484496,0.458227246370285,4.13237600603144));
#36338=CARTESIAN_POINT('Ctrl Pts',(13.2320376006459,0.34048553704322,4.3340137951542));
#36339=CARTESIAN_POINT('Ctrl Pts',(13.2556517167957,0.141144098528766,4.45560285308526));
#36340=CARTESIAN_POINT('Ctrl Pts',(13.2792658329456,-0.0920235057499227,
4.46800351566886));
#36341=CARTESIAN_POINT('Ctrl Pts',(13.3028799490955,-0.30313703626889,4.36824387779166));
#36342=CARTESIAN_POINT('Ctrl Pts',(13.3264940652453,-0.441601665806575,
4.18023203113149));
#36343=CARTESIAN_POINT('Ctrl Pts',(13.3501081813952,-0.47423338199515,3.94902632355453));
#36344=CARTESIAN_POINT('Ctrl Pts',(13.3737222975451,-0.393211766889608,
3.73003681238273));
#36345=CARTESIAN_POINT('Ctrl Pts',(13.3973364136949,-0.217954214568861,
3.57574585842847));
#36346=CARTESIAN_POINT('Ctrl Pts',(13.4209505298448,0.00953758252632317,
3.52313036287841));
#36347=CARTESIAN_POINT('Ctrl Pts',(13.4445646459947,0.234743631574736,3.58479999551538));
#36348=CARTESIAN_POINT('Ctrl Pts',(13.4681787621445,0.403691735186444,3.74597519957476));
#36349=CARTESIAN_POINT('Ctrl Pts',(13.4917928782944,0.475892304226004,3.96802921540861));
#36350=CARTESIAN_POINT('Ctrl Pts',(13.5154069944443,0.434041969710506,4.19774525232923));
#36351=CARTESIAN_POINT('Ctrl Pts',(13.5390211105941,0.288170455640921,4.38007026295756));
#36352=CARTESIAN_POINT('Ctrl Pts',(13.562635226744,0.0732368858249759,4.47130878927046));
#36353=CARTESIAN_POINT('Ctrl Pts',(13.5862493428939,-0.159248413505658,
4.44959488329479));
#36354=CARTESIAN_POINT('Ctrl Pts',(13.6098634590437,-0.353568721957589,
4.32013243375547));
#36355=CARTESIAN_POINT('Ctrl Pts',(13.6334775751936,-0.46315382488092,4.1139480179165));
#36356=CARTESIAN_POINT('Ctrl Pts',(13.6570916913435,-0.461740889501104,
3.88045516635315));
#36357=CARTESIAN_POINT('Ctrl Pts',(13.6807058074933,-0.349668535617837,
3.67561206636528));
#36358=CARTESIAN_POINT('Ctrl Pts',(13.7043199236432,-0.153795683012805,
3.5485107928471));
#36359=CARTESIAN_POINT('Ctrl Pts',(13.7279340397931,0.0789353756500159,
3.5296120507922));
#36360=CARTESIAN_POINT('Ctrl Pts',(13.7515481559429,0.292749022042461,3.62344505529457));
#36361=CARTESIAN_POINT('Ctrl Pts',(13.7751622720928,0.436403327377467,3.80752207362193));
#36362=CARTESIAN_POINT('Ctrl Pts',(13.7987763882427,0.475470537355291,4.03772776690975));
#36363=CARTESIAN_POINT('Ctrl Pts',(13.8223905043925,0.400587923144683,4.25889173822189));
#36364=CARTESIAN_POINT('Ctrl Pts',(13.8460046205424,0.229701624524423,4.41801050223621));
#36365=CARTESIAN_POINT('Ctrl Pts',(13.8696187366923,0.00376573255618155,
4.47695013947711));
#36366=CARTESIAN_POINT('Ctrl Pts',(13.8932328528421,-0.223072643433687,
4.42158535558109));
#36367=CARTESIAN_POINT('Ctrl Pts',(13.916846968992,-0.396450107540549,4.26518470642179));
#36368=CARTESIAN_POINT('Ctrl Pts',(13.9404610851419,-0.474815543552022,
4.04523069632808));
#36369=CARTESIAN_POINT('Ctrl Pts',(13.9640752012917,-0.439388129199652,
3.81443683499316));
#36370=CARTESIAN_POINT('Ctrl Pts',(13.9876893174416,-0.298658290955197,
3.62811447792009));
#36371=CARTESIAN_POINT('Ctrl Pts',(14.0113034335915,-0.0863529142219465,
3.53091707503438));
#36372=CARTESIAN_POINT('Ctrl Pts',(14.0349175497413,0.146647539536438,3.54613866056158));
#36373=CARTESIAN_POINT('Ctrl Pts',(14.0585316658912,0.344502889581789,3.6701312755675));
#36374=CARTESIAN_POINT('Ctrl Pts',(14.0821457820411,0.459795723937725,3.87317922671144));
#36375=CARTESIAN_POINT('Ctrl Pts',(14.1057598981909,0.464895312258427,4.10662065901627));
#36376=CARTESIAN_POINT('Ctrl Pts',(14.1293740143408,0.358579502702881,4.31450970816539));
#36377=CARTESIAN_POINT('Ctrl Pts',(14.1529881304907,0.166327619131383,4.44702431634421));
#36378=CARTESIAN_POINT('Ctrl Pts',(14.1766022466405,-0.0657858362277661,
4.47240643522367));
#36379=CARTESIAN_POINT('Ctrl Pts',(14.2002163627904,-0.282133257977474,
4.38457306332079));
#36380=CARTESIAN_POINT('Ctrl Pts',(14.2238304789403,-0.430865480427841,
4.20457407964992));
#36381=CARTESIAN_POINT('Ctrl Pts',(14.2474445950901,-0.476337791093329,
3.97554749368157));
#36382=CARTESIAN_POINT('Ctrl Pts',(14.27105871124,-0.407652434174819,3.75238112107461));
#36383=CARTESIAN_POINT('Ctrl Pts',(14.2946728273899,-0.241270333599833,
3.58855833656088));
#36384=CARTESIAN_POINT('Ctrl Pts',(14.3182869435397,-0.0170661180132474,
3.52334041087493));
#36385=CARTESIAN_POINT('Ctrl Pts',(14.3419010596896,0.211228111558234,3.57235727391142));
#36386=CARTESIAN_POINT('Ctrl Pts',(14.3655151758395,0.388900053764453,3.72386169322071));
#36387=CARTESIAN_POINT('Ctrl Pts',(14.3891292919893,0.473369390821204,3.94154458004181));
#36388=CARTESIAN_POINT('Ctrl Pts',(14.4127434081392,0.444392458083208,4.17323671518384));
#36389=CARTESIAN_POINT('Ctrl Pts',(14.4363575242891,0.308913779199362,4.3634114655727));
#36390=CARTESIAN_POINT('Ctrl Pts',(14.4599716404389,0.0994017626770733,
4.46649212840691));
#36391=CARTESIAN_POINT('Ctrl Pts',(14.4835857565888,-0.133932578240045,
4.45777470525894));
#36392=CARTESIAN_POINT('Ctrl Pts',(14.5071998727387,-0.335169044432007,
4.33934838727104));
#36393=CARTESIAN_POINT('Ctrl Pts',(14.5308139888885,-0.456079915900645,
4.13959486595487));
#36394=CARTESIAN_POINT('Ctrl Pts',(14.5544281050384,-0.467688060597361,
3.90638646324521));
#36395=CARTESIAN_POINT('Ctrl Pts',(14.5780422211883,-0.367211505836647,
3.69561319629505));
#36396=CARTESIAN_POINT('Ctrl Pts',(14.6016563373381,-0.178730157419731,
3.55778834579073));
#36397=CARTESIAN_POINT('Ctrl Pts',(14.625270453488,0.0525851174261518,3.52594259660587));
#36398=CARTESIAN_POINT('Ctrl Pts',(14.6488845696379,0.271298002813252,3.60770800421126));
#36399=CARTESIAN_POINT('Ctrl Pts',(14.6724986857877,0.424992433239313,3.78348891949988));
#36400=CARTESIAN_POINT('Ctrl Pts',(14.6961128019376,0.476834468501385,4.01115822240469));
#36401=CARTESIAN_POINT('Ctrl Pts',(14.7197269180875,0.414399804028447,4.23615337970372));
#36402=CARTESIAN_POINT('Ctrl Pts',(14.7433410342373,0.252651341641402,4.40455273546398));
#36403=CARTESIAN_POINT('Ctrl Pts',(14.7669551503872,0.0303532266559796,
4.47599821226155));
#36404=CARTESIAN_POINT('Ctrl Pts',(14.7905692665371,-0.199219250862459,
4.43336740322118));
#36405=CARTESIAN_POINT('Ctrl Pts',(14.8141833826869,-0.381047447081096,
4.28687708064914));
#36406=CARTESIAN_POINT('Ctrl Pts',(14.8377974988368,-0.471554972144783,
4.07163466550741));
#36407=CARTESIAN_POINT('Ctrl Pts',(14.8614116149867,-0.449051060899263,
3.83922451083896));
#36408=CARTESIAN_POINT('Ctrl Pts',(14.8850257311365,-0.318928946727196,
3.64534530693059));
#36409=CARTESIAN_POINT('Ctrl Pts',(14.9086398472864,-0.112373269271187,
3.53646160000302));
#36410=CARTESIAN_POINT('Ctrl Pts',(14.9322539634362,0.121113399391719,3.5386680312482));
#36411=CARTESIAN_POINT('Ctrl Pts',(14.9558680795861,0.325574495333277,3.65143602219853));
#36412=CARTESIAN_POINT('Ctrl Pts',(14.979482195736,0.452009190454857,3.84773949289016));
#36413=CARTESIAN_POINT('Ctrl Pts',(15.0030963118858,0.470117180575255,4.08053390545391));
#36414=CARTESIAN_POINT('Ctrl Pts',(15.0267104280357,0.375557372208547,4.29402641177155));
#36415=CARTESIAN_POINT('Ctrl Pts',(15.0503245441856,0.190994688421392,4.43705643304037));
#36416=CARTESIAN_POINT('Ctrl Pts',(15.0739386603355,-0.0393454023191647,
4.47533644032795));
#36417=CARTESIAN_POINT('Ctrl Pts',(15.0975527764853,-0.260245916509526,
4.39971253597763));
#36418=CARTESIAN_POINT('Ctrl Pts',(15.1211668926352,-0.418792603204267,
4.22826540530875));
#36419=CARTESIAN_POINT('Ctrl Pts',(15.1369096367351,-0.457530945318996,
4.07754232577813));
#36420=CARTESIAN_POINT('Ctrl Pts',(15.1447810087851,-0.457870370902723,
4.00205890126089));
#36421=CARTESIAN_POINT('Ctrl Pts',(12.4850729970717,-0.208850989443975,
3.53079950502365));
#36422=CARTESIAN_POINT('Ctrl Pts',(12.4929443691216,-0.131499707516366,
3.49636882573344));
#36423=CARTESIAN_POINT('Ctrl Pts',(12.5086871132215,0.0404888716816997,
3.46654221242176));
#36424=CARTESIAN_POINT('Ctrl Pts',(12.5323012293714,0.288871199237585,3.54969213591223));
#36425=CARTESIAN_POINT('Ctrl Pts',(12.5559153455212,0.467986199318594,3.74075871022993));
#36426=CARTESIAN_POINT('Ctrl Pts',(12.5795294616711,0.534963825407437,3.99395832530641));
#36427=CARTESIAN_POINT('Ctrl Pts',(12.603143577821,0.473725169098917,4.24860452170932));
#36428=CARTESIAN_POINT('Ctrl Pts',(12.6267576939708,0.298958988020687,4.4436716456386));
#36429=CARTESIAN_POINT('Ctrl Pts',(12.6503718101207,0.0525433427838623,
4.53240944903922));
#36430=CARTESIAN_POINT('Ctrl Pts',(12.6739859262706,-0.206463809544117,
4.49355177571912));
#36431=CARTESIAN_POINT('Ctrl Pts',(12.6976000424205,-0.41599087873209,4.33641091237214));
#36432=CARTESIAN_POINT('Ctrl Pts',(12.7212141585703,-0.525822648369464,
4.09864686536754));
#36433=CARTESIAN_POINT('Ctrl Pts',(12.7448282747202,-0.509637448384189,
3.8372413948162));
#36434=CARTESIAN_POINT('Ctrl Pts',(12.76844239087,-0.37131404483003,3.61484216427635));
#36435=CARTESIAN_POINT('Ctrl Pts',(12.7920565070199,-0.144002664868576,
3.48474868689319));
#36436=CARTESIAN_POINT('Ctrl Pts',(12.8156706231698,0.117819965178516,3.47813877511649));
#36437=CARTESIAN_POINT('Ctrl Pts',(12.8392847393197,0.351406216185799,3.59659653799738));
#36438=CARTESIAN_POINT('Ctrl Pts',(12.8628988554695,0.500775523187073,3.81173274911973));
#36439=CARTESIAN_POINT('Ctrl Pts',(12.8865129716194,0.530130489073712,4.07198851734671));
#36440=CARTESIAN_POINT('Ctrl Pts',(12.9101270877692,0.432435993263294,4.31499173633021));
#36441=CARTESIAN_POINT('Ctrl Pts',(12.9337412039191,0.231105201134755,4.48250499290311));
#36442=CARTESIAN_POINT('Ctrl Pts',(12.957355320069,-0.0256115611541523,
4.53438256906268));
#36443=CARTESIAN_POINT('Ctrl Pts',(12.9809694362189,-0.276190334565159,
4.45819164252092));
#36444=CARTESIAN_POINT('Ctrl Pts',(13.0045835523687,-0.460578171623014,
4.27219189922559));
#36445=CARTESIAN_POINT('Ctrl Pts',(13.0281976685186,-0.534585243620437,
4.0209594724593));
#36446=CARTESIAN_POINT('Ctrl Pts',(13.0518117846684,-0.480475240551103,
3.76470396221295));
#36447=CARTESIAN_POINT('Ctrl Pts',(13.0754259008183,-0.311216001335094,
3.5648387853972));
#36448=CARTESIAN_POINT('Ctrl Pts',(13.0990400169682,-0.0673716809183137,
3.46926302296559));
#36449=CARTESIAN_POINT('Ctrl Pts',(13.122654133118,0.19261873182715,3.50088207171981));
#36450=CARTESIAN_POINT('Ctrl Pts',(13.1462682492679,0.406446724606302,3.65211820651514));
#36451=CARTESIAN_POINT('Ctrl Pts',(13.1698823654178,0.522866930420328,3.88672663484193));
#36452=CARTESIAN_POINT('Ctrl Pts',(13.1934964815676,0.513978436505609,4.14848181366307));
#36453=CARTESIAN_POINT('Ctrl Pts',(13.2171105977175,0.381911432304553,4.37465229220773));
#36454=CARTESIAN_POINT('Ctrl Pts',(13.2407247138674,0.158316694737061,4.51103474084347));
#36455=CARTESIAN_POINT('Ctrl Pts',(13.2643388300172,-0.103219740820234,
4.52494415635039));
#36456=CARTESIAN_POINT('Ctrl Pts',(13.2879529461671,-0.340018846942428,
4.41304705047411));
#36457=CARTESIAN_POINT('Ctrl Pts',(13.311567062317,-0.495330069408668,4.20216034359148));
#36458=CARTESIAN_POINT('Ctrl Pts',(13.3351811784669,-0.531931992580964,
3.94282450306062));
#36459=CARTESIAN_POINT('Ctrl Pts',(13.3587952946167,-0.44105271077271,3.69719116838925));
#36460=CARTESIAN_POINT('Ctrl Pts',(13.3824094107666,-0.244472076510672,
3.5241280781681));
#36461=CARTESIAN_POINT('Ctrl Pts',(13.4060235269164,0.0106979927399635,
3.46511100671938));
#36462=CARTESIAN_POINT('Ctrl Pts',(13.4296376430663,0.263304213558122,3.53428380605355));
#36463=CARTESIAN_POINT('Ctrl Pts',(13.4532517592162,0.452807746647384,3.71506873327496));
#36464=CARTESIAN_POINT('Ctrl Pts',(13.476865875366,0.533792751104717,3.96413942206993));
#36465=CARTESIAN_POINT('Ctrl Pts',(13.5004799915159,0.486850606847911,4.22180434800346));
#36466=CARTESIAN_POINT('Ctrl Pts',(13.5240941076658,0.323231325528255,4.42631231788287));
#36467=CARTESIAN_POINT('Ctrl Pts',(13.5477082238157,0.0821474069231642,
4.52865157307741));
#36468=CARTESIAN_POINT('Ctrl Pts',(13.5713223399655,-0.178623709606947,
4.50429579866153));
#36469=CARTESIAN_POINT('Ctrl Pts',(13.5949364561154,-0.396586410669692,
4.35908202552279));
#36470=CARTESIAN_POINT('Ctrl Pts',(13.6185505722652,-0.519504417643299,
4.12781174527607));
#36471=CARTESIAN_POINT('Ctrl Pts',(13.6421646884151,-0.517919574482721,
3.86591049053316));
#36472=CARTESIAN_POINT('Ctrl Pts',(13.665778804565,-0.392211699884016,3.6361447201764));
#36473=CARTESIAN_POINT('Ctrl Pts',(13.6893929207148,-0.172507561089802,
3.49357940054904));
#36474=CARTESIAN_POINT('Ctrl Pts',(13.7130070368647,0.0885392156030666,
3.47238130294519));
#36475=CARTESIAN_POINT('Ctrl Pts',(13.7366211530146,0.328366952925232,3.57763069902274));
#36476=CARTESIAN_POINT('Ctrl Pts',(13.7602352691644,0.489499264105438,3.78410383833506));
#36477=CARTESIAN_POINT('Ctrl Pts',(13.7838493853143,0.533319669072828,4.04231799571659));
#36478=CARTESIAN_POINT('Ctrl Pts',(13.8074635014642,0.449326302728307,4.29039035083475));
#36479=CARTESIAN_POINT('Ctrl Pts',(13.831077617614,0.257648760022572,4.46886863686992));
#36480=CARTESIAN_POINT('Ctrl Pts',(13.8546917337639,0.00422389839726028,
4.53497929012603));
#36481=CARTESIAN_POINT('Ctrl Pts',(13.8783058499138,-0.25021324988294,4.47287843233165));
#36482=CARTESIAN_POINT('Ctrl Pts',(13.9019199660636,-0.444685051009628,
4.29744896636227));
#36483=CARTESIAN_POINT('Ctrl Pts',(13.9255340822135,-0.532584984058807,
4.05073378496132));
#36484=CARTESIAN_POINT('Ctrl Pts',(13.9491481983634,-0.492847218174075,
3.79185989881933));
#36485=CARTESIAN_POINT('Ctrl Pts',(13.9727623145132,-0.334995185577738,
3.58286823685896));
#36486=CARTESIAN_POINT('Ctrl Pts',(13.9963764306631,-0.0968592247428986,
3.47384510573062));
#36487=CARTESIAN_POINT('Ctrl Pts',(14.019990546813,0.164489723571401,3.49091865775613));
#36488=CARTESIAN_POINT('Ctrl Pts',(14.0436046629628,0.386417564563212,3.62999709733779));
#36489=CARTESIAN_POINT('Ctrl Pts',(14.0672187791127,0.515737746224078,3.85774930825782));
#36490=CARTESIAN_POINT('Ctrl Pts',(14.0908328952626,0.521457786777448,4.11959288770904));
#36491=CARTESIAN_POINT('Ctrl Pts',(14.1144470114124,0.402206838685568,4.35277519909424));
#36492=CARTESIAN_POINT('Ctrl Pts',(14.1380611275623,0.186564221804844,4.50141247822903));
#36493=CARTESIAN_POINT('Ctrl Pts',(14.1616752437122,-0.0737898095680628,
4.52988276645436));
#36494=CARTESIAN_POINT('Ctrl Pts',(14.185289359862,-0.316459599402161,4.43136296100575));
#36495=CARTESIAN_POINT('Ctrl Pts',(14.2089034760119,-0.483287643257218,
4.22946401908862));
#36496=CARTESIAN_POINT('Ctrl Pts',(14.2325175921618,-0.53429243907693,3.97257242762026));
#36497=CARTESIAN_POINT('Ctrl Pts',(14.2561317083116,-0.457250332481466,
3.72225404480531));
#36498=CARTESIAN_POINT('Ctrl Pts',(14.2797458244615,-0.270625000632592,
3.53849941363631));
#36499=CARTESIAN_POINT('Ctrl Pts',(14.3033599406114,-0.0191425034699505,
3.46534661065105));
#36500=CARTESIAN_POINT('Ctrl Pts',(14.3269740567612,0.236927627906706,3.52032721432634));
#36501=CARTESIAN_POINT('Ctrl Pts',(14.3505881729111,0.436216403922163,3.69026474025285));
#36502=CARTESIAN_POINT('Ctrl Pts',(14.374202289061,0.530962882087739,3.93443247734966));
#36503=CARTESIAN_POINT('Ctrl Pts',(14.3978164052108,0.498460409348769,4.19431392768733));
#36504=CARTESIAN_POINT('Ctrl Pts',(14.4214305213607,0.346498429557861,4.40762669256976));
#36505=CARTESIAN_POINT('Ctrl Pts',(14.4450446375106,0.111495689030631,4.52324888295055));
#36506=CARTESIAN_POINT('Ctrl Pts',(14.4686587536604,-0.150227769531968,
4.51347083601981));
#36507=CARTESIAN_POINT('Ctrl Pts',(14.4922728698103,-0.375948097339969,
4.38063592879268));
#36508=CARTESIAN_POINT('Ctrl Pts',(14.5158869859602,-0.51156984651846,4.15657897149511));
#36509=CARTESIAN_POINT('Ctrl Pts',(14.53950110211,-0.52459032076832,3.89499677367918));
#36510=CARTESIAN_POINT('Ctrl Pts',(14.5631152182599,-0.411889072794842,
3.65857933001481));
#36511=CARTESIAN_POINT('Ctrl Pts',(14.5867293344098,-0.200475741228102,
3.50398572665543));
#36512=CARTESIAN_POINT('Ctrl Pts',(14.6103434505596,0.0589829973059192,
3.46826539682992));
#36513=CARTESIAN_POINT('Ctrl Pts',(14.6339575667095,0.304306049929579,3.5599789662306));
#36514=CARTESIAN_POINT('Ctrl Pts',(14.6575716828594,0.476700039321847,3.75714663952638));
#36515=CARTESIAN_POINT('Ctrl Pts',(14.6811857990092,0.53484954579562,4.0125158112076));
#36516=CARTESIAN_POINT('Ctrl Pts',(14.7047999151591,0.464818635404008,4.26488548168423));
#36517=CARTESIAN_POINT('Ctrl Pts',(14.728414031309,0.283390703164248,4.45377350235044));
#36518=CARTESIAN_POINT('Ctrl Pts',(14.7520281474588,0.0340462163765225,
4.5339115446661));
#36519=CARTESIAN_POINT('Ctrl Pts',(14.7756422636087,-0.223457683695575,
4.48609396779546));
#36520=CARTESIAN_POINT('Ctrl Pts',(14.7992563797586,-0.427408393186059,
4.32178058932398));
#36521=CARTESIAN_POINT('Ctrl Pts',(14.8228704959084,-0.528927708313459,
4.08035024907128));
#36522=CARTESIAN_POINT('Ctrl Pts',(14.8464846120583,-0.503685810960444,
3.81966341983811));
#36523=CARTESIAN_POINT('Ctrl Pts',(14.8700987282082,-0.357732113691821,
3.6021954912391));
#36524=CARTESIAN_POINT('Ctrl Pts',(14.893712844358,-0.126045401495737,3.48006421709321));
#36525=CARTESIAN_POINT('Ctrl Pts',(14.9173269605079,0.13584891809103,3.48253909847714));
#36526=CARTESIAN_POINT('Ctrl Pts',(14.9409410766578,0.365186207068703,3.60902724630258));
#36527=CARTESIAN_POINT('Ctrl Pts',(14.9645551928076,0.507003847624586,3.82921439524653));
#36528=CARTESIAN_POINT('Ctrl Pts',(14.9881693089575,0.52731498478211,4.0903322339271));
#36529=CARTESIAN_POINT('Ctrl Pts',(15.0117834251074,0.421250356706029,4.32979975898591));
#36530=CARTESIAN_POINT('Ctrl Pts',(15.0353975412572,0.214232462415332,4.49023183125449));
#36531=CARTESIAN_POINT('Ctrl Pts',(15.0590116574071,-0.0441324441701724,
4.53316925684615));
#36532=CARTESIAN_POINT('Ctrl Pts',(15.082625773557,-0.291909288096862,4.4483444097243));
#36533=CARTESIAN_POINT('Ctrl Pts',(15.1062398897068,-0.469745893811612,
4.25603780014884));
#36534=CARTESIAN_POINT('Ctrl Pts',(15.1219826338067,-0.513197418509596,
4.08697667736293));
#36535=CARTESIAN_POINT('Ctrl Pts',(15.1298540058567,-0.513578141027115,
4.0023094018511));
#36536=CARTESIAN_POINT('Ctrl Pts',(12.4701459941433,-0.231505035597357,
3.47990537377399));
#36537=CARTESIAN_POINT('Ctrl Pts',(12.4780173661933,-0.145763467775118,
3.44174000210903));
#36538=CARTESIAN_POINT('Ctrl Pts',(12.4937601102932,0.0448806955855158,
3.40867809900361));
#36539=CARTESIAN_POINT('Ctrl Pts',(12.517374226443,0.320205029627059,3.5008472864651));
#36540=CARTESIAN_POINT('Ctrl Pts',(12.5409883425929,0.518748616038451,3.71263883318769));
#36541=CARTESIAN_POINT('Ctrl Pts',(12.5646024587428,0.592991298599855,3.99330298545039));
#36542=CARTESIAN_POINT('Ctrl Pts',(12.5882165748926,0.525110091302815,4.27557062957281));
#36543=CARTESIAN_POINT('Ctrl Pts',(12.6118306910425,0.331387039860997,4.49179666512739));
#36544=CARTESIAN_POINT('Ctrl Pts',(12.6354448071924,0.0582427139750047,
4.5901598492798));
#36545=CARTESIAN_POINT('Ctrl Pts',(12.6590589233422,-0.22885891853004,4.54708728798072));
#36546=CARTESIAN_POINT('Ctrl Pts',(12.6826730394921,-0.461113368174311,
4.37290137073994));
#36547=CARTESIAN_POINT('Ctrl Pts',(12.706287155642,-0.582858578993347,4.10934708109011));
#36548=CARTESIAN_POINT('Ctrl Pts',(12.7299012717918,-0.564917771967644,
3.8195869850214));
#36549=CARTESIAN_POINT('Ctrl Pts',(12.7535153879417,-0.411590442520908,
3.57306413195747));
#36550=CARTESIAN_POINT('Ctrl Pts',(12.7771295040916,-0.159622619673808,
3.42885942795892));
#36551=CARTESIAN_POINT('Ctrl Pts',(12.8007436202414,0.130599885139872,3.42153253970604));
#36552=CARTESIAN_POINT('Ctrl Pts',(12.8243577363913,0.38952321367407,3.55283940440193));
#36553=CARTESIAN_POINT('Ctrl Pts',(12.8479718525412,0.555094594621529,3.79131141905102));
#36554=CARTESIAN_POINT('Ctrl Pts',(12.871585968691,0.587633690752404,4.07979710469805));
#36555=CARTESIAN_POINT('Ctrl Pts',(12.8952000848409,0.479342282651013,4.34915885879276));
#36556=CARTESIAN_POINT('Ctrl Pts',(12.9188142009908,0.256173159427565,4.53484226172604));
#36557=CARTESIAN_POINT('Ctrl Pts',(12.9424283171406,-0.0283896446575681,
4.59234699343691));
#36558=CARTESIAN_POINT('Ctrl Pts',(12.9660424332905,-0.306148672818738,
4.50789164463438));
#36559=CARTESIAN_POINT('Ctrl Pts',(12.9896565494404,-0.510537040311962,
4.30171652759364));
#36560=CARTESIAN_POINT('Ctrl Pts',(13.0132706655902,-0.59257165208389,4.02323294436244));
#36561=CARTESIAN_POINT('Ctrl Pts',(13.0368847817401,-0.532592342337314,
3.73918142428326));
#36562=CARTESIAN_POINT('Ctrl Pts',(13.06049889789,-0.344973570196446,3.51763689152052));
#36563=CARTESIAN_POINT('Ctrl Pts',(13.0841130140398,-0.0746794804792245,
3.41169403559782));
#36564=CARTESIAN_POINT('Ctrl Pts',(13.1077271301897,0.213512066603468,3.44674279944083));
#36565=CARTESIAN_POINT('Ctrl Pts',(13.1313412463396,0.450533960595157,3.6143835028084));
#36566=CARTESIAN_POINT('Ctrl Pts',(13.1549553624894,0.579582254610818,3.87443988413478));
#36567=CARTESIAN_POINT('Ctrl Pts',(13.1785694786393,0.569729626640933,4.1645876212947));
#36568=CARTESIAN_POINT('Ctrl Pts',(13.2021835947892,0.423337327565886,4.41529078926125));
#36569=CARTESIAN_POINT('Ctrl Pts',(13.225797710939,0.175489290945357,4.56646662860168));
#36570=CARTESIAN_POINT('Ctrl Pts',(13.2494118270889,-0.114415975890545,
4.58188479703192));
#36571=CARTESIAN_POINT('Ctrl Pts',(13.2730259432388,-0.376900657615966,
4.45785022315656));
#36572=CARTESIAN_POINT('Ctrl Pts',(13.2966400593886,-0.54905847301076,4.22408865605146));
#36573=CARTESIAN_POINT('Ctrl Pts',(13.3202541755385,-0.589630603166779,
3.93662268256671));
#36574=CARTESIAN_POINT('Ctrl Pts',(13.3438682916884,-0.488893654655812,
3.66434552439578));
#36575=CARTESIAN_POINT('Ctrl Pts',(13.3674824078382,-0.270989938452484,
3.47251029790774));
#36576=CARTESIAN_POINT('Ctrl Pts',(13.3910965239881,0.0118584029536041,
3.40709165056035));
#36577=CARTESIAN_POINT('Ctrl Pts',(13.414710640138,0.291864795541507,3.48376761659174));
#36578=CARTESIAN_POINT('Ctrl Pts',(13.4383247562878,0.501923758108325,3.68416226697515));
#36579=CARTESIAN_POINT('Ctrl Pts',(13.4619388724377,0.591693197983429,3.96024962873126));
#36580=CARTESIAN_POINT('Ctrl Pts',(13.4855529885876,0.539659243985316,4.2458634436777));
#36581=CARTESIAN_POINT('Ctrl Pts',(13.5091671047374,0.358292195415589,4.47255437280819));
#36582=CARTESIAN_POINT('Ctrl Pts',(13.5327812208873,0.0910579280213527,
4.58599435688436));
#36583=CARTESIAN_POINT('Ctrl Pts',(13.5563953370372,-0.197999005708236,
4.55899671402827));
#36584=CARTESIAN_POINT('Ctrl Pts',(13.580009453187,-0.439604099381795,4.39803161729011));
#36585=CARTESIAN_POINT('Ctrl Pts',(13.6036235693369,-0.575855010405679,
4.14167547263565));
#36586=CARTESIAN_POINT('Ctrl Pts',(13.6272376854868,-0.574098259464336,
3.85136581471317));
#36587=CARTESIAN_POINT('Ctrl Pts',(13.6508518016366,-0.434754864150196,
3.59667737398752));
#36588=CARTESIAN_POINT('Ctrl Pts',(13.6744659177865,-0.191219439166798,
3.43864800825098));
#36589=CARTESIAN_POINT('Ctrl Pts',(13.6980800339364,0.0981430555561168,
3.41515055509818));
#36590=CARTESIAN_POINT('Ctrl Pts',(13.7216941500862,0.363984883808003,3.53181634275091));
#36591=CARTESIAN_POINT('Ctrl Pts',(13.7453082662361,0.54259520083341,3.76068560304818));
#36592=CARTESIAN_POINT('Ctrl Pts',(13.768922382386,0.591168800790367,4.04690822452342));
#36593=CARTESIAN_POINT('Ctrl Pts',(13.7925364985358,0.498064682311931,4.32188896344761));
#36594=CARTESIAN_POINT('Ctrl Pts',(13.8161506146857,0.28559589552072,4.51972677150362));
#36595=CARTESIAN_POINT('Ctrl Pts',(13.8397647308356,0.00468206423833927,
4.59300844077494));
#36596=CARTESIAN_POINT('Ctrl Pts',(13.8633788469854,-0.277353856332193,
4.52417150908221));
#36597=CARTESIAN_POINT('Ctrl Pts',(13.8869929631353,-0.492919994478707,
4.32971322630275));
#36598=CARTESIAN_POINT('Ctrl Pts',(13.9106070792852,-0.590354424565592,
4.05623687359455));
#36599=CARTESIAN_POINT('Ctrl Pts',(13.934221195435,-0.546306307148498,3.76928296264551));
#36600=CARTESIAN_POINT('Ctrl Pts',(13.9578353115849,-0.371332080200278,
3.53762199579782));
#36601=CARTESIAN_POINT('Ctrl Pts',(13.9814494277348,-0.107365535263851,
3.41677313642685));
#36602=CARTESIAN_POINT('Ctrl Pts',(14.0050635438846,0.182331907606365,3.43569865495067));
#36603=CARTESIAN_POINT('Ctrl Pts',(14.0286776600345,0.428332239544634,3.58986291910809));
#36604=CARTESIAN_POINT('Ctrl Pts',(14.0522917761844,0.571679768510432,3.8423193898042));
#36605=CARTESIAN_POINT('Ctrl Pts',(14.0759058923342,0.578020261296468,4.1325651164018));
#36606=CARTESIAN_POINT('Ctrl Pts',(14.0995200084841,0.445834174668256,4.39104069002309));
#36607=CARTESIAN_POINT('Ctrl Pts',(14.123134124634,0.206800824478305,4.55580064011384));
#36608=CARTESIAN_POINT('Ctrl Pts',(14.1467482407838,-0.0817937829083601,
4.58735909768505));
#36609=CARTESIAN_POINT('Ctrl Pts',(14.1703623569337,-0.350785940826847,
4.4781528586907));
#36610=CARTESIAN_POINT('Ctrl Pts',(14.1939764730836,-0.535709806086595,
4.25435395852733));
#36611=CARTESIAN_POINT('Ctrl Pts',(14.2175905892334,-0.59224708706053,3.96959736155895));
#36612=CARTESIAN_POINT('Ctrl Pts',(14.2412047053833,-0.506848230788112,
3.69212696853602));
#36613=CARTESIAN_POINT('Ctrl Pts',(14.2648188215332,-0.29997966766535,3.48844049071174));
#36614=CARTESIAN_POINT('Ctrl Pts',(14.288432937683,-0.0212188889266537,
3.40735281042717));
#36615=CARTESIAN_POINT('Ctrl Pts',(14.3120470538329,0.262627144255178,3.46829715474127));
#36616=CARTESIAN_POINT('Ctrl Pts',(14.3356611699828,0.483532754079872,3.65666778728498));
#36617=CARTESIAN_POINT('Ctrl Pts',(14.3592752861326,0.588556373354274,3.9273203746575));
#36618=CARTESIAN_POINT('Ctrl Pts',(14.3828894022825,0.55252836061433,4.21539114019081));
#36619=CARTESIAN_POINT('Ctrl Pts',(14.4065035184324,0.384083079916361,4.45184191956682));
#36620=CARTESIAN_POINT('Ctrl Pts',(14.4301176345822,0.123589615384189,4.58000563749418));
#36621=CARTESIAN_POINT('Ctrl Pts',(14.4537317507321,-0.166522960823891,
4.56916696678068));
#36622=CARTESIAN_POINT('Ctrl Pts',(14.477345866882,-0.416727150247931,4.42192347031433));
#36623=CARTESIAN_POINT('Ctrl Pts',(14.5009599830318,-0.567059777136274,
4.17356307703535));
#36624=CARTESIAN_POINT('Ctrl Pts',(14.5245740991817,-0.58149258093928,3.88360708411314));
#36625=CARTESIAN_POINT('Ctrl Pts',(14.5481882153316,-0.456566639753037,
3.62154546373458));
#36626=CARTESIAN_POINT('Ctrl Pts',(14.5718023314814,-0.222221325036472,
3.45018310752014));
#36627=CARTESIAN_POINT('Ctrl Pts',(14.5954164476313,0.0653808771856868,
3.41058819705396));
#36628=CARTESIAN_POINT('Ctrl Pts',(14.6190305637812,0.337314097045906,3.51224992824993));
#36629=CARTESIAN_POINT('Ctrl Pts',(14.642644679931,0.528407645404381,3.73080435955289));
#36630=CARTESIAN_POINT('Ctrl Pts',(14.6662587960809,0.592864623089856,4.0138734000105));
#36631=CARTESIAN_POINT('Ctrl Pts',(14.6898729122308,0.515237466779568,4.29361758366474));
#36632=CARTESIAN_POINT('Ctrl Pts',(14.7134870283806,0.314130064687094,4.5029942692369));
#36633=CARTESIAN_POINT('Ctrl Pts',(14.7371011445305,0.0377392060970651,
4.59182487707066));
#36634=CARTESIAN_POINT('Ctrl Pts',(14.7607152606804,-0.24769611652869,4.53882053236973));
#36635=CARTESIAN_POINT('Ctrl Pts',(14.7843293768302,-0.47376933929102,4.35668409799883));
#36636=CARTESIAN_POINT('Ctrl Pts',(14.8079434929801,-0.586300444482135,
4.08906583263515));
#36637=CARTESIAN_POINT('Ctrl Pts',(14.83155760913,-0.558320561021625,3.80010232883727));
#36638=CARTESIAN_POINT('Ctrl Pts',(14.8551717252798,-0.396535280656446,
3.55904567554761));
#36639=CARTESIAN_POINT('Ctrl Pts',(14.8787858414297,-0.139717533720287,
3.42366683418339));
#36640=CARTESIAN_POINT('Ctrl Pts',(14.9023999575795,0.150584436790342,3.42641016570609));
#36641=CARTESIAN_POINT('Ctrl Pts',(14.9260140737294,0.404797918804129,3.56661847040663));
#36642=CARTESIAN_POINT('Ctrl Pts',(14.9496281898793,0.561998504794314,3.8106892976029));
#36643=CARTESIAN_POINT('Ctrl Pts',(14.9732423060292,0.584512788988964,4.10013056240029));
#36644=CARTESIAN_POINT('Ctrl Pts',(14.996856422179,0.466943341203511,4.36557310620026));
#36645=CARTESIAN_POINT('Ctrl Pts',(15.0204705383289,0.237470236409271,4.54340722946861));
#36646=CARTESIAN_POINT('Ctrl Pts',(15.0440846544788,-0.0489194860211801,
4.59100207336435));
#36647=CARTESIAN_POINT('Ctrl Pts',(15.0676987706286,-0.323572659684198,
4.49697628347096));
#36648=CARTESIAN_POINT('Ctrl Pts',(15.0913128867785,-0.520699184418956,
4.28381019498893));
#36649=CARTESIAN_POINT('Ctrl Pts',(15.1070556308784,-0.568863891700195,
4.09641102894772));
#36650=CARTESIAN_POINT('Ctrl Pts',(15.1149270029284,-0.569285911151507,
4.00255990244131));
#36651=CARTESIAN_POINT('Ctrl Pts',(12.455218991215,-0.25415908175074,3.42901124252432));
#36652=CARTESIAN_POINT('Ctrl Pts',(12.4630903632649,-0.16002722803387,3.38711117848463));
#36653=CARTESIAN_POINT('Ctrl Pts',(12.4788331073648,0.0492725194893315,
3.35081398558546));
#36654=CARTESIAN_POINT('Ctrl Pts',(12.5024472235147,0.351538860016532,3.45200243701797));
#36655=CARTESIAN_POINT('Ctrl Pts',(12.5260613396645,0.569511032758309,3.68451895614546));
#36656=CARTESIAN_POINT('Ctrl Pts',(12.5496754558144,0.651018771792273,3.99264764559437));
#36657=CARTESIAN_POINT('Ctrl Pts',(12.5732895719643,0.576495013506714,4.3025367374363));
#36658=CARTESIAN_POINT('Ctrl Pts',(12.5969036881141,0.363815091701307,4.53992168461618));
#36659=CARTESIAN_POINT('Ctrl Pts',(12.620517804264,0.0639420851661475,4.64791024952038));
#36660=CARTESIAN_POINT('Ctrl Pts',(12.6441319204139,-0.251254027515963,
4.60062280024232));
#36661=CARTESIAN_POINT('Ctrl Pts',(12.6677460365637,-0.506235857616531,
4.40939182910775));
#36662=CARTESIAN_POINT('Ctrl Pts',(12.6913601527136,-0.639894509617229,
4.12004729681268));
#36663=CARTESIAN_POINT('Ctrl Pts',(12.7149742688635,-0.620198095551099,
3.8019325752266));
#36664=CARTESIAN_POINT('Ctrl Pts',(12.7385883850133,-0.451866840211785,
3.53128609963859));
#36665=CARTESIAN_POINT('Ctrl Pts',(12.7622025011632,-0.17524257447904,3.37297016902465));
#36666=CARTESIAN_POINT('Ctrl Pts',(12.7858166173131,0.143379805101228,3.36492630429559));
#36667=CARTESIAN_POINT('Ctrl Pts',(12.809430733463,0.42764021116234,3.50908227080648));
#36668=CARTESIAN_POINT('Ctrl Pts',(12.8330448496128,0.609413666055986,3.77089008898231));
#36669=CARTESIAN_POINT('Ctrl Pts',(12.8566589657627,0.645136892431096,4.08760569204938));
#36670=CARTESIAN_POINT('Ctrl Pts',(12.8802730819125,0.526248572038732,4.38332598125533));
#36671=CARTESIAN_POINT('Ctrl Pts',(12.9038871980624,0.281241117720374,4.58717953054897));
#36672=CARTESIAN_POINT('Ctrl Pts',(12.9275013142123,-0.0311677281609838,
4.65031141781114));
#36673=CARTESIAN_POINT('Ctrl Pts',(12.9511154303622,-0.336107011072318,
4.55759164674784));
#36674=CARTESIAN_POINT('Ctrl Pts',(12.974729546512,-0.56049590900091,4.33124115596169));
#36675=CARTESIAN_POINT('Ctrl Pts',(12.9983436626619,-0.650558060547343,
4.02550641626558));
#36676=CARTESIAN_POINT('Ctrl Pts',(13.0219577788117,-0.584709444123524,
3.71365888635357));
#36677=CARTESIAN_POINT('Ctrl Pts',(13.0455718949616,-0.378731139057797,
3.47043499764384));
#36678=CARTESIAN_POINT('Ctrl Pts',(13.0691860111115,-0.0819872800401352,
3.35412504823007));
#36679=CARTESIAN_POINT('Ctrl Pts',(13.0928001272613,0.234405401379786,3.39260352716186));
#36680=CARTESIAN_POINT('Ctrl Pts',(13.1164142434112,0.494621196584012,3.57664879910166));
#36681=CARTESIAN_POINT('Ctrl Pts',(13.1400283595611,0.636297578801308,3.86215313342763));
#36682=CARTESIAN_POINT('Ctrl Pts',(13.1636424757109,0.625480816776257,4.18069342892634));
#36683=CARTESIAN_POINT('Ctrl Pts',(13.1872565918608,0.464763222827219,4.45592928631477));
#36684=CARTESIAN_POINT('Ctrl Pts',(13.2108707080107,0.192661887153653,4.62189851635989));
#36685=CARTESIAN_POINT('Ctrl Pts',(13.2344848241605,-0.125612210960856,
4.63882543771344));
#36686=CARTESIAN_POINT('Ctrl Pts',(13.2580989403104,-0.413782468289504,
4.50265339583901));
#36687=CARTESIAN_POINT('Ctrl Pts',(13.2817130564603,-0.602786876612853,
4.24601696851145));
#36688=CARTESIAN_POINT('Ctrl Pts',(13.3053271726101,-0.647329213752593,
3.9304208620728));
#36689=CARTESIAN_POINT('Ctrl Pts',(13.32894128876,-0.536734598538914,3.6314998804023));
#36690=CARTESIAN_POINT('Ctrl Pts',(13.3525554049099,-0.297507800394296,
3.42089251764738));
#36691=CARTESIAN_POINT('Ctrl Pts',(13.3761695210598,0.0130188131672444,
3.34907229440132));
#36692=CARTESIAN_POINT('Ctrl Pts',(13.3997836372096,0.320425377524893,3.43325142712992));
#36693=CARTESIAN_POINT('Ctrl Pts',(13.4233977533595,0.551039769569266,3.65325580067535));
#36694=CARTESIAN_POINT('Ctrl Pts',(13.4470118695093,0.649593644862141,3.95635983539258));
#36695=CARTESIAN_POINT('Ctrl Pts',(13.4706259856592,0.592467881122722,4.26992253935193));
#36696=CARTESIAN_POINT('Ctrl Pts',(13.4942401018091,0.393353065302923,4.5187964277335));
#36697=CARTESIAN_POINT('Ctrl Pts',(13.5178542179589,0.0999684491195412,
4.64333714069132));
#36698=CARTESIAN_POINT('Ctrl Pts',(13.5414683341088,-0.217374301809525,
4.61369762939502));
#36699=CARTESIAN_POINT('Ctrl Pts',(13.5650824502587,-0.482621788093898,
4.43698120905743));
#36700=CARTESIAN_POINT('Ctrl Pts',(13.5886965664085,-0.632205603168059,
4.15553919999523));
#36701=CARTESIAN_POINT('Ctrl Pts',(13.6123106825584,-0.630276944445953,
3.83682113889318));
#36702=CARTESIAN_POINT('Ctrl Pts',(13.6359247987083,-0.477298028416376,
3.55721002779864));
#36703=CARTESIAN_POINT('Ctrl Pts',(13.6595389148582,-0.209931317243796,
3.38371661595291));
#36704=CARTESIAN_POINT('Ctrl Pts',(13.683153031008,0.107746895509167,3.35791980725116));
#36705=CARTESIAN_POINT('Ctrl Pts',(13.7067671471579,0.399602814690774,3.48600198647908));
#36706=CARTESIAN_POINT('Ctrl Pts',(13.7303812633077,0.59569113756138,3.73726736776131));
#36707=CARTESIAN_POINT('Ctrl Pts',(13.7539953794576,0.649017932507905,4.05149845333026));
#36708=CARTESIAN_POINT('Ctrl Pts',(13.7776094956075,0.546803061895555,4.35338757606046));
#36709=CARTESIAN_POINT('Ctrl Pts',(13.8012236117573,0.313543031018869,4.57058490613733));
#36710=CARTESIAN_POINT('Ctrl Pts',(13.8248377279072,0.00514023007941788,
4.65103759142385));
#36711=CARTESIAN_POINT('Ctrl Pts',(13.8484518440571,-0.304494462781446,
4.57546458583277));
#36712=CARTESIAN_POINT('Ctrl Pts',(13.8720659602069,-0.541154937947787,
4.36197748624323));
#36713=CARTESIAN_POINT('Ctrl Pts',(13.8956800763568,-0.648123865072376,
4.06173996222779));
#36714=CARTESIAN_POINT('Ctrl Pts',(13.9192941925067,-0.599765396122921,
3.74670602647169));
#36715=CARTESIAN_POINT('Ctrl Pts',(13.9429083086565,-0.407668974822819,
3.49237575473668));
#36716=CARTESIAN_POINT('Ctrl Pts',(13.9665224248064,-0.117871845784803,
3.35970116712309));
#36717=CARTESIAN_POINT('Ctrl Pts',(13.9901365409563,0.200174091641329,3.38047865214521));
#36718=CARTESIAN_POINT('Ctrl Pts',(14.0137506571061,0.470246914526057,3.54972874087838));
#36719=CARTESIAN_POINT('Ctrl Pts',(14.037364773256,0.627621790796785,3.82688947135059));
#36720=CARTESIAN_POINT('Ctrl Pts',(14.0609788894059,0.634582735815489,4.14553734509456));
#36721=CARTESIAN_POINT('Ctrl Pts',(14.0845930055557,0.489461510650943,4.42930618095194));
#36722=CARTESIAN_POINT('Ctrl Pts',(14.1082071217056,0.227037427151766,4.61018880199865));
#36723=CARTESIAN_POINT('Ctrl Pts',(14.1318212378555,-0.0897977562486571,
4.64483542891575));
#36724=CARTESIAN_POINT('Ctrl Pts',(14.1554353540053,-0.385112282251534,
4.52494275637564));
#36725=CARTESIAN_POINT('Ctrl Pts',(14.1790494701552,-0.588131968915973,
4.27924389796604));
#36726=CARTESIAN_POINT('Ctrl Pts',(14.2026635863051,-0.65020173504413,3.96662229549764));
#36727=CARTESIAN_POINT('Ctrl Pts',(14.2262777024549,-0.556446129094758,
3.66199989226673));
#36728=CARTESIAN_POINT('Ctrl Pts',(14.2498918186048,-0.329334334698108,
3.43838156778717));
#36729=CARTESIAN_POINT('Ctrl Pts',(14.2735059347547,-0.0232952743833569,
3.34935901020328));
#36730=CARTESIAN_POINT('Ctrl Pts',(14.2971200509045,0.28832666060365,3.41626709515619));
#36731=CARTESIAN_POINT('Ctrl Pts',(14.3207341670544,0.530849104237583,3.62307083431711));
#36732=CARTESIAN_POINT('Ctrl Pts',(14.3443482832043,0.646149864620809,3.92020827196535));
#36733=CARTESIAN_POINT('Ctrl Pts',(14.3679623993541,0.606596311879891,4.2364683526943));
#36734=CARTESIAN_POINT('Ctrl Pts',(14.391576515504,0.42166773027486,4.49605714656388));
#36735=CARTESIAN_POINT('Ctrl Pts',(14.4151906316539,0.135683541737747,4.63676239203782));
#36736=CARTESIAN_POINT('Ctrl Pts',(14.4388047478037,-0.182818152115814,
4.62486309754155));
#36737=CARTESIAN_POINT('Ctrl Pts',(14.4624188639536,-0.457506203155893,
4.46321101183598));
#36738=CARTESIAN_POINT('Ctrl Pts',(14.4860329801035,-0.622549707754089,
4.19054718257559));
#36739=CARTESIAN_POINT('Ctrl Pts',(14.5096470962533,-0.63839484111024,3.87221739454711));
#36740=CARTESIAN_POINT('Ctrl Pts',(14.5332612124032,-0.501244206711231,
3.58451159745434));
#36741=CARTESIAN_POINT('Ctrl Pts',(14.5568753285531,-0.243966908844842,
3.39638048838484));
#36742=CARTESIAN_POINT('Ctrl Pts',(14.5804894447029,0.0717787570654544,
3.35291099727801));
#36743=CARTESIAN_POINT('Ctrl Pts',(14.6041035608528,0.370322144162233,3.46452089026927));
#36744=CARTESIAN_POINT('Ctrl Pts',(14.6277176770027,0.580115251486915,3.70446207957941));
#36745=CARTESIAN_POINT('Ctrl Pts',(14.6513317931525,0.650879700384091,4.0152309888134));
#36746=CARTESIAN_POINT('Ctrl Pts',(14.6749459093024,0.565656298155129,4.32234968564526));
#36747=CARTESIAN_POINT('Ctrl Pts',(14.6985600254523,0.344869426209941,4.55221503612336));
#36748=CARTESIAN_POINT('Ctrl Pts',(14.7221741416021,0.041432195817608,4.64973820947522));
#36749=CARTESIAN_POINT('Ctrl Pts',(14.745788257752,-0.271934549361806,4.59154709694401));
#36750=CARTESIAN_POINT('Ctrl Pts',(14.7694023739019,-0.520130285395982,
4.39158760667368));
#36751=CARTESIAN_POINT('Ctrl Pts',(14.7930164900517,-0.64367318065081,4.09778141619902));
#36752=CARTESIAN_POINT('Ctrl Pts',(14.8166306062016,-0.612955311082805,
3.78054123783642));
#36753=CARTESIAN_POINT('Ctrl Pts',(14.8402447223515,-0.435338447621071,
3.51589585985611));
#36754=CARTESIAN_POINT('Ctrl Pts',(14.8638588385013,-0.153389665944836,
3.36726945127358));
#36755=CARTESIAN_POINT('Ctrl Pts',(14.8874729546512,0.165319955489652,3.37028123293502));
#36756=CARTESIAN_POINT('Ctrl Pts',(14.9110870708011,0.444409630539555,3.52420969451069));
#36757=CARTESIAN_POINT('Ctrl Pts',(14.9347011869509,0.616993161964042,3.79216419995926));
#36758=CARTESIAN_POINT('Ctrl Pts',(14.9583153031008,0.641710593195818,4.10992889087348));
#36759=CARTESIAN_POINT('Ctrl Pts',(14.9819294192507,0.512636325700993,4.40134645341462));
#36760=CARTESIAN_POINT('Ctrl Pts',(15.0055435354005,0.260708010403211,4.59658262768273));
#36761=CARTESIAN_POINT('Ctrl Pts',(15.0291576515504,-0.0537065278721878,
4.64883488988255));
#36762=CARTESIAN_POINT('Ctrl Pts',(15.0527717677003,-0.355236031271534,
4.54560815721762));
#36763=CARTESIAN_POINT('Ctrl Pts',(15.0763858838501,-0.571652475026301,
4.31158258982903));
#36764=CARTESIAN_POINT('Ctrl Pts',(15.09212862795,-0.624530364890795,4.10584538053252));
#36765=CARTESIAN_POINT('Ctrl Pts',(15.1,-0.624993681275899,4.00281040303152));
#36766=CARTESIAN_POINT('Ctrl Pts',(15.1,-0.624993681275899,4.00281040303152));
#36767=CARTESIAN_POINT('Ctrl Pts',(15.1,-0.617358358083874,4.02914127082806));
#36768=CARTESIAN_POINT('Ctrl Pts',(15.1,-0.607931963506944,4.05484759228836));
#36769=CARTESIAN_POINT('Ctrl Pts',(15.1,-0.596773861259576,4.07974656001827));
#36770=CARTESIAN_POINT('Ctrl Pts',(15.1,-0.585871522029423,4.10407480030985));
#36771=CARTESIAN_POINT('Ctrl Pts',(15.1,-0.573314772633929,4.12763281365198));
#36772=CARTESIAN_POINT('Ctrl Pts',(15.1,-0.559143639302279,4.1502040881484));
#36773=CARTESIAN_POINT('Ctrl Pts',(15.1,-0.549626121151564,4.16536325076984));
#36774=CARTESIAN_POINT('Ctrl Pts',(15.1,-0.539380106047495,4.18007635520315));
#36775=CARTESIAN_POINT('Ctrl Pts',(15.1,-0.528417753985571,4.19426420824267));
#36776=CARTESIAN_POINT('Ctrl Pts',(15.1,-0.523814643226911,4.2002217124899));
#36777=CARTESIAN_POINT('Ctrl Pts',(15.1,-0.519084627089791,4.20608691507751));
#36778=CARTESIAN_POINT('Ctrl Pts',(15.1,-0.514239086396905,4.21184190560023));
#36779=CARTESIAN_POINT('Ctrl Pts',(15.1,-0.50085552272952,4.2277374035328));
#36780=CARTESIAN_POINT('Ctrl Pts',(15.1,-0.486572803760524,4.24281789068328));
#36781=CARTESIAN_POINT('Ctrl Pts',(15.1,-0.4714177983537,4.25697008589974));
#36782=CARTESIAN_POINT('Ctrl Pts',(15.1,-0.457151696655403,4.27029219637033));
#36783=CARTESIAN_POINT('Ctrl Pts',(15.1,-0.442112042545397,4.28279146400573));
#36784=CARTESIAN_POINT('Ctrl Pts',(15.1,-0.426369607892924,4.29437520287289));
#36785=CARTESIAN_POINT('Ctrl Pts',(15.1,-0.419074661497203,4.29974303548351));
#36786=CARTESIAN_POINT('Ctrl Pts',(15.1,-0.411628924918527,4.30491398987477));
#36787=CARTESIAN_POINT('Ctrl Pts',(15.1,-0.404040271526401,4.30987739070861));
#36788=CARTESIAN_POINT('Ctrl Pts',(15.1,-0.398073367501634,4.31378007737535));
#36789=CARTESIAN_POINT('Ctrl Pts',(15.1,-0.392026704362881,4.31754881952869));
#36790=CARTESIAN_POINT('Ctrl Pts',(15.1,-0.385904261325812,4.32117966642505));
#36791=CARTESIAN_POINT('Ctrl Pts',(15.1,-0.366868686798561,4.33246850264191));
#36792=CARTESIAN_POINT('Ctrl Pts',(15.1,-0.347097727375919,4.34242824684389));
#36793=CARTESIAN_POINT('Ctrl Pts',(15.1,-0.326713262272485,4.3509180109496));
#36794=CARTESIAN_POINT('Ctrl Pts',(15.1,-0.308010762698638,4.35870726657947));
#36795=CARTESIAN_POINT('Ctrl Pts',(15.1,-0.288791261952878,4.36525839133365));
#36796=CARTESIAN_POINT('Ctrl Pts',(15.1,-0.269173508333929,4.37043259773196));
#36797=CARTESIAN_POINT('Ctrl Pts',(12.5,-0.186196943290592,3.58169363627332));
#36798=CARTESIAN_POINT('Ctrl Pts',(12.5,-0.170588484282379,3.56594316788148));
#36799=CARTESIAN_POINT('Ctrl Pts',(12.5,-0.153797667832464,3.55144458439849));
#36800=CARTESIAN_POINT('Ctrl Pts',(12.5,-0.136060690067392,3.53823162417247));
#36801=CARTESIAN_POINT('Ctrl Pts',(12.5,-0.117990710310259,3.5247705978929));
#36802=CARTESIAN_POINT('Ctrl Pts',(12.5,-0.0989385549429972,3.51264262455394));
#36803=CARTESIAN_POINT('Ctrl Pts',(12.5,-0.0790990435859813,3.5018744512649));
#36804=CARTESIAN_POINT('Ctrl Pts',(12.5,-0.0668145727052721,3.49520688224936));
#36805=CARTESIAN_POINT('Ctrl Pts',(12.5,-0.054227138249592,3.4890605701039));
#36806=CARTESIAN_POINT('Ctrl Pts',(12.5,-0.0413735013057162,3.4834433907237));
#36807=CARTESIAN_POINT('Ctrl Pts',(12.5,-0.0353493612034326,3.48081077586818));
#36808=CARTESIAN_POINT('Ctrl Pts',(12.5,-0.0292710672153644,3.47829647656688));
#36809=CARTESIAN_POINT('Ctrl Pts',(12.5,-0.0231507758853709,3.47590397706369));
#36810=CARTESIAN_POINT('Ctrl Pts',(12.5,-0.00211397253512804,3.467680423829));
#36811=CARTESIAN_POINT('Ctrl Pts',(12.5,0.0194422610390746,3.46088402724794));
#36812=CARTESIAN_POINT('Ctrl Pts',(12.5,0.0413436963816045,3.45552737346533));
#36813=CARTESIAN_POINT('Ctrl Pts',(12.5,0.0650920698750741,3.44971899548849));
#36814=CARTESIAN_POINT('Ctrl Pts',(12.5,0.089246474293393,3.44560199012534));
#36815=CARTESIAN_POINT('Ctrl Pts',(12.5,0.113633446029948,3.44311473184586));
#36816=CARTESIAN_POINT('Ctrl Pts',(12.5,0.123118497624279,3.44214733936417));
#36817=CARTESIAN_POINT('Ctrl Pts',(12.5,0.132642564327611,3.44142688205345));
#36818=CARTESIAN_POINT('Ctrl Pts',(12.5,0.142169452875131,3.44095138714122));
#36819=CARTESIAN_POINT('Ctrl Pts',(12.5,0.170359862108328,3.43954438042575));
#36820=CARTESIAN_POINT('Ctrl Pts',(12.5,0.19861482332424,3.44027367679077));
#36821=CARTESIAN_POINT('Ctrl Pts',(12.5,0.226679319731597,3.44302987267532));
#36822=CARTESIAN_POINT('Ctrl Pts',(12.5,0.254743816138955,3.44578606855986));
#36823=CARTESIAN_POINT('Ctrl Pts',(12.5,0.282619254593541,3.45056842907764));
#36824=CARTESIAN_POINT('Ctrl Pts',(12.5,0.310093463203745,3.45730861053194));
#36825=CARTESIAN_POINT('Ctrl Pts',(15.0699957084852,-1.05870731373636E-5,
4.45788944868556));
#36826=CARTESIAN_POINT('Ctrl Pts',(15.0634386537186,0.0628625045491076,
4.45782850550181));
#36827=CARTESIAN_POINT('Ctrl Pts',(15.0568815989521,0.125761012144406,4.44477074790967));
#36828=CARTESIAN_POINT('Ctrl Pts',(15.0503245441856,0.183365120595825,4.41959809737683));
#36829=CARTESIAN_POINT('Ctrl Pts',(15.0424531721356,0.252515583017112,4.38937975928409));
#36830=CARTESIAN_POINT('Ctrl Pts',(15.0345818000857,0.314036477612831,4.34170308552782));
#36831=CARTESIAN_POINT('Ctrl Pts',(15.0267104280357,0.360556892971808,4.28228266426341));
#36832=CARTESIAN_POINT('Ctrl Pts',(15.0188390559858,0.407077308330786,4.222862242999));
#36833=CARTESIAN_POINT('Ctrl Pts',(15.0109676839358,0.438597244453022,4.15169807422645));
#36834=CARTESIAN_POINT('Ctrl Pts',(15.0030963118859,0.45133921416074,4.07731692107955));
#36835=CARTESIAN_POINT('Ctrl Pts',(14.9952249398359,0.464081183868457,4.00293576793266));
#36836=CARTESIAN_POINT('Ctrl Pts',(14.9873535677859,0.458045187161657,3.92533763041141));
#36837=CARTESIAN_POINT('Ctrl Pts',(14.979482195736,0.433954739621328,3.85382131653551));
#36838=CARTESIAN_POINT('Ctrl Pts',(14.971610823686,0.409864292080999,3.78230500265962));
#36839=CARTESIAN_POINT('Ctrl Pts',(14.9637394516361,0.367719393707138,3.71687051242907));
#36840=CARTESIAN_POINT('Ctrl Pts',(14.9558680795861,0.312570095196614,3.66535860215541));
#36841=CARTESIAN_POINT('Ctrl Pts',(14.9479967075362,0.257420796686091,3.61384669188175));
#36842=CARTESIAN_POINT('Ctrl Pts',(14.9401253354862,0.189267098038905,3.57625736156498));
#36843=CARTESIAN_POINT('Ctrl Pts',(14.9322539634362,0.116275803938161,3.55709495786573));
#36844=CARTESIAN_POINT('Ctrl Pts',(14.9243825913863,0.0432845098374172,
3.53793255416647));
#36845=CARTESIAN_POINT('Ctrl Pts',(14.9165112193363,-0.0345443797168851,
3.53719707708475));
#36846=CARTESIAN_POINT('Ctrl Pts',(14.9086398472864,-0.107884770736704,
3.55497662303181));
#36847=CARTESIAN_POINT('Ctrl Pts',(14.9007684752364,-0.181225161756525,
3.57275616897888));
#36848=CARTESIAN_POINT('Ctrl Pts',(14.8928971031865,-0.250077054241862,
3.60905073795473));
#36849=CARTESIAN_POINT('Ctrl Pts',(14.8850257311365,-0.306190019513209,
3.65951122309406));
#36850=CARTESIAN_POINT('Ctrl Pts',(14.8771543590866,-0.362302984784554,
3.70997170823338));
#36851=CARTESIAN_POINT('Ctrl Pts',(14.8692829870366,-0.405677022841909,
3.77459810953617));
#36852=CARTESIAN_POINT('Ctrl Pts',(14.8614116149867,-0.431114693744839,
3.84564633596564));
#36853=CARTESIAN_POINT('Ctrl Pts',(14.8535402429367,-0.45655236464777,3.91669456239511));
#36854=CARTESIAN_POINT('Ctrl Pts',(14.8456688708867,-0.464053668396277,
3.99416461395126));
#36855=CARTESIAN_POINT('Ctrl Pts',(14.8377974988368,-0.452719732759917,
4.06877337558629));
#36856=CARTESIAN_POINT('Ctrl Pts',(14.8299261267868,-0.441385797123556,
4.14338213722132));
#36857=CARTESIAN_POINT('Ctrl Pts',(14.8220547547369,-0.411216622102327,
4.21512960893523));
#36858=CARTESIAN_POINT('Ctrl Pts',(14.8141833826869,-0.365827335221939,
4.27541839855419));
#36859=CARTESIAN_POINT('Ctrl Pts',(14.806312010637,-0.32043804834155,4.33570718817315));
#36860=CARTESIAN_POINT('Ctrl Pts',(14.798440638587,-0.259828649602004,4.38453729569717));
#36861=CARTESIAN_POINT('Ctrl Pts',(14.7905692665371,-0.191261870645823,
4.41605748429924));
#36862=CARTESIAN_POINT('Ctrl Pts',(14.7837114138531,-0.131523763221734,
4.44351912740692));
#36863=CARTESIAN_POINT('Ctrl Pts',(14.7768535611691,-0.065745536276614,
4.45784152413683));
#36864=CARTESIAN_POINT('Ctrl Pts',(14.7699957084852,8.6346448269735E-6,
4.45789857801605));
#36865=CARTESIAN_POINT('Ctrl Pts',(12.5,0.310062960217722,4.54266560670548));
#36866=CARTESIAN_POINT('Ctrl Pts',(12.50787137205,0.220600394030941,4.59378185169648));
#36867=CARTESIAN_POINT('Ctrl Pts',(12.5236141161499,0.0159878432799406,
4.65085692712531));
#36868=CARTESIAN_POINT('Ctrl Pts',(12.5472282322997,-0.294892507759568,
4.580447501361));
#36869=CARTESIAN_POINT('Ctrl Pts',(12.5708423484496,-0.535054221536356,
4.37092866956447));
#36870=CARTESIAN_POINT('Ctrl Pts',(12.5944564645995,-0.647009713430093,
4.07251155115386));
#36871=CARTESIAN_POINT('Ctrl Pts',(12.6180705807493,-0.603894380709874,
3.75671714932517));
#36872=CARTESIAN_POINT('Ctrl Pts',(12.6416846968992,-0.416056506175611,
3.49922677321964));
#36873=CARTESIAN_POINT('Ctrl Pts',(12.6652988130491,-0.128505496873939,
3.36175035317655));
#36874=CARTESIAN_POINT('Ctrl Pts',(12.6889129291989,0.189841674427298,3.37723482234205));
#36875=CARTESIAN_POINT('Ctrl Pts',(12.7125270453488,0.462692468193658,3.54196933898577));
#36876=CARTESIAN_POINT('Ctrl Pts',(12.7361411614987,0.624655556881011,3.81647407445394));
#36877=CARTESIAN_POINT('Ctrl Pts',(12.7597552776485,0.636915702199809,4.13496208375113));
#36878=CARTESIAN_POINT('Ctrl Pts',(12.7833693937984,0.496534514683115,4.42110548633398));
#36879=CARTESIAN_POINT('Ctrl Pts',(12.8069835099483,0.237155397994168,4.60632802944461));
#36880=CARTESIAN_POINT('Ctrl Pts',(12.8305976260981,-0.0790596718614395,
4.64623983861064));
#36881=CARTESIAN_POINT('Ctrl Pts',(12.854211742248,-0.376327535803878,4.5312757721487));
#36882=CARTESIAN_POINT('Ctrl Pts',(12.8778258583979,-0.583405888470749,
4.28898776831928));
#36883=CARTESIAN_POINT('Ctrl Pts',(12.9014399745477,-0.650666957548692,
3.97744183415536));
#36884=CARTESIAN_POINT('Ctrl Pts',(12.9250540906976,-0.561991161265395,
3.67130212143154));
#36885=CARTESIAN_POINT('Ctrl Pts',(12.9486682068475,-0.338630270727757,
3.44393714350224));
#36886=CARTESIAN_POINT('Ctrl Pts',(12.9722823229973,-0.0341142786054444,
3.34983650006563));
#36887=CARTESIAN_POINT('Ctrl Pts',(12.9958964391472,0.278577437919422,3.41155206540036));
#36888=CARTESIAN_POINT('Ctrl Pts',(13.0195105552971,0.524506132150044,3.61429327464512));
#36889=CARTESIAN_POINT('Ctrl Pts',(13.0431246714469,0.644733280558021,3.90947178565704));
#36890=CARTESIAN_POINT('Ctrl Pts',(13.0667387875968,0.61044561006836,4.22634601343335));
#36891=CARTESIAN_POINT('Ctrl Pts',(13.0903529037467,0.429860399609997,4.4889748434194));
#36892=CARTESIAN_POINT('Ctrl Pts',(13.1139670198965,0.146256151980267,4.63441744826062));
#36893=CARTESIAN_POINT('Ctrl Pts',(13.1375811360464,-0.172399400609521,
4.62781749523177));
#36894=CARTESIAN_POINT('Ctrl Pts',(13.1611952521963,-0.449738236712957,
4.47075670902068));
#36895=CARTESIAN_POINT('Ctrl Pts',(13.1848093683461,-0.619294173608025,
4.2008758003961));
#36896=CARTESIAN_POINT('Ctrl Pts',(13.208423484496,-0.64043195068177,3.88285360784221));
#36897=CARTESIAN_POINT('Ctrl Pts',(13.2320376006459,-0.508085752511173,
3.59290636366459));
#36898=CARTESIAN_POINT('Ctrl Pts',(13.2556517167957,-0.253973266794505,
3.40052194335125));
#36899=CARTESIAN_POINT('Ctrl Pts',(13.2792658329456,0.0610056803032868,
3.3518066124833));
#36900=CARTESIAN_POINT('Ctrl Pts',(13.3028799490955,0.361364191435218,3.45843533922715));
#36901=CARTESIAN_POINT('Ctrl Pts',(13.3264940652453,0.575119258511334,3.69485380694));
#36902=CARTESIAN_POINT('Ctrl Pts',(13.3501081813952,0.65104299168552,4.00440268404554));
#36903=CARTESIAN_POINT('Ctrl Pts',(13.3737222975451,0.570939739771795,4.31289642727099));
#36904=CARTESIAN_POINT('Ctrl Pts',(13.3973364136949,0.354006804717113,4.54640236352309));
#36905=CARTESIAN_POINT('Ctrl Pts',(13.4209505298448,0.0522336745508671,
4.6489591696652));
#36906=CARTESIAN_POINT('Ctrl Pts',(13.4445646459947,-0.26205761933777,4.59598839317277));
#36907=CARTESIAN_POINT('Ctrl Pts',(13.4681787621445,-0.513544980480383,
4.40018484937968));
#36908=CARTESIAN_POINT('Ctrl Pts',(13.4917928782944,-0.64195771209056,4.10847422061066));
#36909=CARTESIAN_POINT('Ctrl Pts',(13.5154069944443,-0.616520809113462,
3.79076698974655));
#36910=CARTESIAN_POINT('Ctrl Pts',(13.5390211105941,-0.443330402422436,
3.52320390633144));
#36911=CARTESIAN_POINT('Ctrl Pts',(13.562635226744,-0.163892778617988,3.36990832590288));
#36912=CARTESIAN_POINT('Ctrl Pts',(13.5862493428939,0.154822890495328,3.36761860145296));
#36913=CARTESIAN_POINT('Ctrl Pts',(13.6098634590437,0.43643417612693,3.51688348138565));
#36914=CARTESIAN_POINT('Ctrl Pts',(13.6334775751936,0.613450973283793,3.78193059814177));
#36915=CARTESIAN_POINT('Ctrl Pts',(13.6570916913435,0.643449974253473,4.09923956510808));
#36916=CARTESIAN_POINT('Ctrl Pts',(13.6807058074933,0.519241709620395,4.39276507945606));
#36917=CARTESIAN_POINT('Ctrl Pts',(13.7043199236432,0.270593554659618,4.59216170834183));
#36918=CARTESIAN_POINT('Ctrl Pts',(13.7279340397931,-0.0429042293685969,
4.64964266158552));
#36919=CARTESIAN_POINT('Ctrl Pts',(13.7515481559429,-0.346119716157775,
4.55143222859795));
#36920=CARTESIAN_POINT('Ctrl Pts',(13.7751622720928,-0.566385203513325,
4.32106722332061));
#36921=CARTESIAN_POINT('Ctrl Pts',(13.7987763882427,-0.650912534047929,
4.01375622291695));
#36922=CARTESIAN_POINT('Ctrl Pts',(13.8223905043925,-0.57944414457563,3.70314844792952));
#36923=CARTESIAN_POINT('Ctrl Pts',(13.8460046205424,-0.369107932149097,
3.46368321387984));
#36924=CARTESIAN_POINT('Ctrl Pts',(13.8696187366923,-0.0703124342978696,
3.35275003110641));
#36925=CARTESIAN_POINT('Ctrl Pts',(13.8932328528421,0.245333927901481,3.3969348091043));
#36926=CARTESIAN_POINT('Ctrl Pts',(13.916846968992,0.502184306426786,3.58564835824111));
#36927=CARTESIAN_POINT('Ctrl Pts',(13.9404610851419,0.638682720042094,3.87366416276737));
#36928=CARTESIAN_POINT('Ctrl Pts',(13.9640752012917,0.62211637371287,4.19195723015293));
#36929=CARTESIAN_POINT('Ctrl Pts',(13.9876893174416,0.456455507660852,4.46424641105313));
#36930=CARTESIAN_POINT('Ctrl Pts',(14.0113034335915,0.181401901656729,4.62527570776815));
#36931=CARTESIAN_POINT('Ctrl Pts',(14.0349175497413,-0.137125932879425,
4.63645332836083));
#36932=CARTESIAN_POINT('Ctrl Pts',(14.0585316658912,-0.422790583021024,
4.49510047824495));
#36933=CARTESIAN_POINT('Ctrl Pts',(14.0821457820411,-0.60713052675338,4.23509335195577));
#36934=CARTESIAN_POINT('Ctrl Pts',(14.1057598981909,-0.645967413308333,
3.91874446730605));
#36935=CARTESIAN_POINT('Ctrl Pts',(14.1293740143408,-0.529993712466286,
3.62186903671368));
#36936=CARTESIAN_POINT('Ctrl Pts',(14.1529881304907,-0.287003328966194,
3.41561532377041));
#36937=CARTESIAN_POINT('Ctrl Pts',(14.1766022466405,0.0247694002478971,
3.34941346658496));
#36938=CARTESIAN_POINT('Ctrl Pts',(14.2002163627904,0.330605970264406,3.43912920108534));
#36939=CARTESIAN_POINT('Ctrl Pts',(14.2238304789403,0.557210518047066,3.66326152695696));
#36940=CARTESIAN_POINT('Ctrl Pts',(14.2474445950901,0.650275686248857,3.96809557204375));
#36941=CARTESIAN_POINT('Ctrl Pts',(14.27105871124,0.587497759452106,4.28057573538778));
#36942=CARTESIAN_POINT('Ctrl Pts',(14.2946728273899,0.383921904832036,4.52581397056352));
#36943=CARTESIAN_POINT('Ctrl Pts',(14.3182869435397,0.088336493108731,4.64503722732482));
#36944=CARTESIAN_POINT('Ctrl Pts',(14.3419010596896,-0.22841937412829,4.6096728222354));
#36945=CARTESIAN_POINT('Ctrl Pts',(14.3655151758395,-0.490432948250941,
4.42819608115853));
#36946=CARTESIAN_POINT('Ctrl Pts',(14.3891292919893,-0.634910852255616,
4.14409916841427));
#36947=CARTESIAN_POINT('Ctrl Pts',(14.4127434081392,-0.627227950688033,
3.82546788683648));
#36948=CARTESIAN_POINT('Ctrl Pts',(14.4363575242891,-0.469225504392149,
3.54866444115539));
#36949=CARTESIAN_POINT('Ctrl Pts',(14.4599716404389,-0.198769899531221,
3.38002670405092));
#36950=CARTESIAN_POINT('Ctrl Pts',(14.4835857565888,0.11932229545683,3.35996988316441));
#36951=CARTESIAN_POINT('Ctrl Pts',(14.5071998727387,0.408818071695872,3.49330073524378));
#36952=CARTESIAN_POINT('Ctrl Pts',(14.5308139888885,0.600337751131954,3.74806559342675));
#36953=CARTESIAN_POINT('Ctrl Pts',(14.5544281050384,0.647982309355475,4.06320828594604));
#36954=CARTESIAN_POINT('Ctrl Pts',(14.5780422211883,0.540333396317157,4.36320267272319));
#36955=CARTESIAN_POINT('Ctrl Pts',(14.6016563373381,0.303189823409542,4.57615301060753));
#36956=CARTESIAN_POINT('Ctrl Pts',(14.625270453488,-0.00661530128860875,
4.65102426869959));
#36957=CARTESIAN_POINT('Ctrl Pts',(14.6488845696379,-0.314835022974042,
4.56987302880665));
#36958=CARTESIAN_POINT('Ctrl Pts',(14.6724986857877,-0.547602339746838,
4.35214775046202));
#36959=CARTESIAN_POINT('Ctrl Pts',(14.6961128019376,-0.649132943719538,
4.05002781234082));
#36960=CARTESIAN_POINT('Ctrl Pts',(14.7197269180875,-0.595094318970103,
3.73591836064326));
#36961=CARTESIAN_POINT('Ctrl Pts',(14.7433410342373,-0.398437197867616,
3.48509791236843));
#36962=CARTESIAN_POINT('Ctrl Pts',(14.7669551503872,-0.1062918289807,3.35767733339665));
#36963=CARTESIAN_POINT('Ctrl Pts',(14.7905692665371,0.211327117384507,3.38419385377023));
#36964=CARTESIAN_POINT('Ctrl Pts',(14.8141833826869,0.478300047385911,3.5582926020622));
#36965=CARTESIAN_POINT('Ctrl Pts',(14.8377974988368,0.630645044771057,3.83824960712979));
#36966=CARTESIAN_POINT('Ctrl Pts',(14.8614116149867,0.631851559871185,4.15697121131127));
#36967=CARTESIAN_POINT('Ctrl Pts',(14.8850257311365,0.481630465478622,4.4380735902585));
#36968=CARTESIAN_POINT('Ctrl Pts',(14.9086398472864,0.215983244330552,4.61418854455152));
#36969=CARTESIAN_POINT('Ctrl Pts',(14.9322539634363,-0.101425794369151,
4.64310902247508));
#36970=CARTESIAN_POINT('Ctrl Pts',(14.9558680795861,-0.394527586443172,
4.517903766532));
#36971=CARTESIAN_POINT('Ctrl Pts',(14.979482195736,-0.593077772790822,4.26857965265179));
#36972=CARTESIAN_POINT('Ctrl Pts',(15.0030963118859,-0.649493436571599,
3.95488773069898));
#36973=CARTESIAN_POINT('Ctrl Pts',(15.0267104280357,-0.550252000240565,
3.65200904506483));
#36974=CARTESIAN_POINT('Ctrl Pts',(15.0503245441856,-0.319142060764588,
3.43252503194012));
#36975=CARTESIAN_POINT('Ctrl Pts',(15.0739386603355,-0.0115409051696555,
3.34904846156061));
#36976=CARTESIAN_POINT('Ctrl Pts',(15.0975527764853,0.298810377697559,3.42155963907315));
#36977=CARTESIAN_POINT('Ctrl Pts',(15.1211668926352,0.537575400322941,3.63273573589665));
#36978=CARTESIAN_POINT('Ctrl Pts',(15.1369096367351,0.610790903144771,3.83214323401692));
#36979=CARTESIAN_POINT('Ctrl Pts',(15.1447810087851,0.621570310124627,3.93461384266089));
#36980=CARTESIAN_POINT('Ctrl Pts',(12.4850729970716,0.282426015030316,4.49429601229446));
#36981=CARTESIAN_POINT('Ctrl Pts',(12.4929443691216,0.200937545576316,4.54085609598193));
#36982=CARTESIAN_POINT('Ctrl Pts',(12.5086871132215,0.0145627935155885,
4.59284387968754));
#36983=CARTESIAN_POINT('Ctrl Pts',(12.5323012293714,-0.268607755567932,
4.52871028073968));
#36984=CARTESIAN_POINT('Ctrl Pts',(12.5559153455213,-0.487363055256749,
4.3378665608173));
#36985=CARTESIAN_POINT('Ctrl Pts',(12.5795294616711,-0.589339580973024,
4.06604835489435));
#36986=CARTESIAN_POINT('Ctrl Pts',(12.603143577821,-0.550067261575934,3.77840176074865));
#36987=CARTESIAN_POINT('Ctrl Pts',(12.6267576939709,-0.378972002925158,
3.54386236016666));
#36988=CARTESIAN_POINT('Ctrl Pts',(12.6503718101207,-0.117051373585908,
3.41863967169675));
#36989=CARTESIAN_POINT('Ctrl Pts',(12.6739859262706,0.172920453180012,3.43274395851062));
#36990=CARTESIAN_POINT('Ctrl Pts',(12.6976000424204,0.42145114619533,3.58279513857084));
#36991=CARTESIAN_POINT('Ctrl Pts',(12.7212141585703,0.568977924911017,3.83283235195095));
#36992=CARTESIAN_POINT('Ctrl Pts',(12.7448282747202,0.580145282610399,4.12293246335278));
#36993=CARTESIAN_POINT('Ctrl Pts',(12.76844239087,0.45227673827436,4.38357095065208));
#36994=CARTESIAN_POINT('Ctrl Pts',(12.7920565070199,0.216016946852954,4.55228399108678));
#36995=CARTESIAN_POINT('Ctrl Pts',(12.8156706231698,-0.0720128197761896,
4.58863832766248));
#36996=CARTESIAN_POINT('Ctrl Pts',(12.8392847393196,-0.34278420811256,4.48392139165784));
#36997=CARTESIAN_POINT('Ctrl Pts',(12.8628988554695,-0.531404976945056,
4.26322932523642));
#36998=CARTESIAN_POINT('Ctrl Pts',(12.8865129716194,-0.592670842732518,
3.97945251867098));
#36999=CARTESIAN_POINT('Ctrl Pts',(12.9101270877692,-0.51189901575794,3.70060005900794));
#37000=CARTESIAN_POINT('Ctrl Pts',(12.9337412039191,-0.308447025930223,
3.49350087944474));
#37001=CARTESIAN_POINT('Ctrl Pts',(12.957355320069,-0.0310735592390789,
3.40778774002645));
#37002=CARTESIAN_POINT('Ctrl Pts',(12.9809694362188,0.253746902286204,3.46400239130434));
#37003=CARTESIAN_POINT('Ctrl Pts',(13.0045835523687,0.477755152237737,3.64867260076509));
#37004=CARTESIAN_POINT('Ctrl Pts',(13.0281976685186,0.587266054150949,3.91754086716214));
#37005=CARTESIAN_POINT('Ctrl Pts',(13.0518117846685,0.556034558024266,4.20617103876933));
#37006=CARTESIAN_POINT('Ctrl Pts',(13.0754259008183,0.391545509324759,4.44539088570928));
#37007=CARTESIAN_POINT('Ctrl Pts',(13.0990400169682,0.133219853633759,4.57786970637232));
#37008=CARTESIAN_POINT('Ctrl Pts',(13.122654133118,-0.157032867368526,4.57185802915678));
#37009=CARTESIAN_POINT('Ctrl Pts',(13.1462682492679,-0.409651568547275,
4.42879659435664));
#37010=CARTESIAN_POINT('Ctrl Pts',(13.1698823654178,-0.564094419600429,
4.1829710707208));
#37011=CARTESIAN_POINT('Ctrl Pts',(13.1934964815676,-0.583348116144335,
3.89329525626321));
#37012=CARTESIAN_POINT('Ctrl Pts',(13.2171105977175,-0.462798375770677,
3.62919197644995));
#37013=CARTESIAN_POINT('Ctrl Pts',(13.2407247138674,-0.231335782947555,
3.45395542080054));
#37014=CARTESIAN_POINT('Ctrl Pts',(13.2643388300172,0.055568040665587,3.40958224975729));
#37015=CARTESIAN_POINT('Ctrl Pts',(13.2879529461671,0.329154596505292,3.50670680265737));
#37016=CARTESIAN_POINT('Ctrl Pts',(13.311567062317,0.523856961936024,3.72205250428141));
#37017=CARTESIAN_POINT('Ctrl Pts',(13.3351811784668,0.593013359693284,4.00401025814095));
#37018=CARTESIAN_POINT('Ctrl Pts',(13.3587952946167,0.520049977633468,4.28500692572024));
#37019=CARTESIAN_POINT('Ctrl Pts',(13.3824094107666,0.322452998189994,4.49769969952106));
#37020=CARTESIAN_POINT('Ctrl Pts',(13.4060235269164,0.0475779130258999,
4.59111527567571));
#37021=CARTESIAN_POINT('Ctrl Pts',(13.4296376430663,-0.238699550200797,
4.5428659610613));
#37022=CARTESIAN_POINT('Ctrl Pts',(13.4532517592162,-0.467771004553565,
4.36451503980497));
#37023=CARTESIAN_POINT('Ctrl Pts',(13.476865875366,-0.584737881352888,4.09880555174689));
#37024=CARTESIAN_POINT('Ctrl Pts',(13.5004799915159,-0.561568254327815,
3.80941662539381));
#37025=CARTESIAN_POINT('Ctrl Pts',(13.5240941076658,-0.403814885886516,
3.56570233148043));
#37026=CARTESIAN_POINT('Ctrl Pts',(13.5477082238157,-0.149284468950505,
3.42607049712074));
#37027=CARTESIAN_POINT('Ctrl Pts',(13.5713223399655,0.141023010189178,3.42398486344345));
#37028=CARTESIAN_POINT('Ctrl Pts',(13.5949364561154,0.39753334322815,3.55994526707815));
#37029=CARTESIAN_POINT('Ctrl Pts',(13.6185505722652,0.55877204319843,3.8013678508274));
#37030=CARTESIAN_POINT('Ctrl Pts',(13.6421646884151,0.586097133215014,4.09039401187145));
#37031=CARTESIAN_POINT('Ctrl Pts',(13.665778804565,0.47295996523623,4.35775661870721));
#37032=CARTESIAN_POINT('Ctrl Pts',(13.6893929207148,0.24647464915429,4.53938036140496));
#37033=CARTESIAN_POINT('Ctrl Pts',(13.7130070368647,-0.0390800323908759,
4.59173784568287));
#37034=CARTESIAN_POINT('Ctrl Pts',(13.7366211530146,-0.315268912124245,
4.50228123595558));
#37035=CARTESIAN_POINT('Ctrl Pts',(13.7602352691644,-0.515901402373503,
4.29244943148197));
#37036=CARTESIAN_POINT('Ctrl Pts',(13.7838493853143,-0.59289453017979,4.01253008491428));
#37037=CARTESIAN_POINT('Ctrl Pts',(13.8074635014642,-0.527796356489121,
3.72960781627073));
#37038=CARTESIAN_POINT('Ctrl Pts',(13.831077617614,-0.336208111796874,3.51148691674935));
#37039=CARTESIAN_POINT('Ctrl Pts',(13.8546917337639,-0.0640452526541193,
3.4104415783338));
#37040=CARTESIAN_POINT('Ctrl Pts',(13.8783058499138,0.223466497127862,3.45068801978614));
#37041=CARTESIAN_POINT('Ctrl Pts',(13.9019199660636,0.457422945247278,3.62258090124322));
#37042=CARTESIAN_POINT('Ctrl Pts',(13.9255340822135,0.581754800262342,3.88492489705937));
#37043=CARTESIAN_POINT('Ctrl Pts',(13.9491481983634,0.566665067602596,4.17484744237197));
#37044=CARTESIAN_POINT('Ctrl Pts',(13.9727623145132,0.415770106744681,4.42286658094793));
#37045=CARTESIAN_POINT('Ctrl Pts',(13.9963764306631,0.165232945489059,4.56954279968241));
#37046=CARTESIAN_POINT('Ctrl Pts',(14.019990546813,-0.124903441395439,4.57972412169294));
#37047=CARTESIAN_POINT('Ctrl Pts',(14.0436046629628,-0.385105849054417,
4.45097052228405));
#37048=CARTESIAN_POINT('Ctrl Pts',(14.0672187791127,-0.553014959135429,
4.21413869785145));
#37049=CARTESIAN_POINT('Ctrl Pts',(14.0908328952626,-0.58839018453545,3.92598704378684));
#37050=CARTESIAN_POINT('Ctrl Pts',(14.1144470114124,-0.482753606228458,
3.65557310990793));
#37051=CARTESIAN_POINT('Ctrl Pts',(14.1380611275623,-0.261421765577673,
3.46770347791168));
#37052=CARTESIAN_POINT('Ctrl Pts',(14.1616752437122,0.0225616210391343,
3.40740241293002));
#37053=CARTESIAN_POINT('Ctrl Pts',(14.185289359862,0.301137958114838,3.48912148496193));
#37054=CARTESIAN_POINT('Ctrl Pts',(14.2089034760119,0.507544487205137,3.69327614952086));
#37055=CARTESIAN_POINT('Ctrl Pts',(14.2325175921618,0.592314446747875,3.97093932005559));
#37056=CARTESIAN_POINT('Ctrl Pts',(14.2561317083116,0.535132125826274,4.25556708484021));
#37057=CARTESIAN_POINT('Ctrl Pts',(14.2797458244615,0.349701665714674,4.47894641865396));
#37058=CARTESIAN_POINT('Ctrl Pts',(14.3033599406114,0.0804627670229728,
4.58754290912926));
#37059=CARTESIAN_POINT('Ctrl Pts',(14.3269740567612,-0.208059593914322,
4.55533065134682));
#37060=CARTESIAN_POINT('Ctrl Pts',(14.3505881729111,-0.44671902479684,4.39002953712461));
#37061=CARTESIAN_POINT('Ctrl Pts',(14.374202289061,-0.578319131624566,4.13125512920294));
#37062=CARTESIAN_POINT('Ctrl Pts',(14.3978164052108,-0.571321032683373,
3.84102451585645));
#37063=CARTESIAN_POINT('Ctrl Pts',(14.4214305213607,-0.427401871100662,
3.58889348396707));
#37064=CARTESIAN_POINT('Ctrl Pts',(14.4450446375106,-0.181052875819672,
3.43528699049651));
#37065=CARTESIAN_POINT('Ctrl Pts',(14.4686587536604,0.108686701521778,3.41701790091169));
#37066=CARTESIAN_POINT('Ctrl Pts',(14.4922728698103,0.372378754238714,3.53846452970905));
#37067=CARTESIAN_POINT('Ctrl Pts',(14.5158869859602,0.546827646247725,3.77052134686598));
#37068=CARTESIAN_POINT('Ctrl Pts',(14.53950110211,0.59022548618159,4.05757432072539));
#37069=CARTESIAN_POINT('Ctrl Pts',(14.5631152182599,0.492171679592087,4.3308292078278));
#37070=CARTESIAN_POINT('Ctrl Pts',(14.5867293344098,0.276165503816305,4.52479857226205));
#37071=CARTESIAN_POINT('Ctrl Pts',(14.6103434505596,-0.00602565743375084,
4.59299630554951));
#37072=CARTESIAN_POINT('Ctrl Pts',(14.6339575667095,-0.286772727926288,
4.51907834617235));
#37073=CARTESIAN_POINT('Ctrl Pts',(14.6575716828594,-0.49879271786407,4.32075964763751));
#37074=CARTESIAN_POINT('Ctrl Pts',(14.6811857990092,-0.591273560669336,
4.04556866666751));
#37075=CARTESIAN_POINT('Ctrl Pts',(14.7047999151591,-0.542051578672567,
3.75945683743125));
#37076=CARTESIAN_POINT('Ctrl Pts',(14.728414031309,-0.362923162297683,3.53099285177933));
#37077=CARTESIAN_POINT('Ctrl Pts',(14.7520281474588,-0.0968176839575538,
3.41492969374656));
#37078=CARTESIAN_POINT('Ctrl Pts',(14.7756422636087,0.192490826988301,3.43908270827084));
#37079=CARTESIAN_POINT('Ctrl Pts',(14.7992563797586,0.435667569828913,3.59766345479839));
#37080=CARTESIAN_POINT('Ctrl Pts',(14.8228704959084,0.574433549780463,3.85266695881428));
#37081=CARTESIAN_POINT('Ctrl Pts',(14.8464846120583,0.575532524168,4.14297984400973));
#37082=CARTESIAN_POINT('Ctrl Pts',(14.8700987282082,0.438701136655627,4.39902663091346));
#37083=CARTESIAN_POINT('Ctrl Pts',(14.893712844358,0.196731937819222,4.55944387228049));
#37084=CARTESIAN_POINT('Ctrl Pts',(14.9173269605079,-0.0923853752310475,
4.58578657160514));
#37085=CARTESIAN_POINT('Ctrl Pts',(14.9409410766578,-0.359362027571537,
4.47174127747511));
#37086=CARTESIAN_POINT('Ctrl Pts',(14.9645551928076,-0.540214773976066,
4.24464025294543));
#37087=CARTESIAN_POINT('Ctrl Pts',(14.9881693089575,-0.59160192159185,3.95890873763601));
#37088=CARTESIAN_POINT('Ctrl Pts',(15.0117834251074,-0.501206205285789,
3.68302663884805));
#37089=CARTESIAN_POINT('Ctrl Pts',(15.0353975412572,-0.290695865081771,
3.48310596742652));
#37090=CARTESIAN_POINT('Ctrl Pts',(15.0590116574071,-0.0105122258222001,
3.40706994202017));
#37091=CARTESIAN_POINT('Ctrl Pts',(15.082625773557,0.272176412698783,3.47311795657709));
#37092=CARTESIAN_POINT('Ctrl Pts',(15.1062398897068,0.489659512974156,3.66547122397039));
#37093=CARTESIAN_POINT('Ctrl Pts',(15.1219826338067,0.5563490739778,3.84710486709154));
#37094=CARTESIAN_POINT('Ctrl Pts',(15.1298540058567,0.566167676482186,3.94044192881839));
#37095=CARTESIAN_POINT('Ctrl Pts',(12.4701459941433,0.254789069842909,4.44592641788345));
#37096=CARTESIAN_POINT('Ctrl Pts',(12.4780173661933,0.181274697121691,4.48793034026739));
#37097=CARTESIAN_POINT('Ctrl Pts',(12.4937601102932,0.0131377437512366,
4.53483083224977));
#37098=CARTESIAN_POINT('Ctrl Pts',(12.517374226443,-0.242323003376296,4.47697306011837));
#37099=CARTESIAN_POINT('Ctrl Pts',(12.5409883425929,-0.439671888977142,
4.30480445207012));
#37100=CARTESIAN_POINT('Ctrl Pts',(12.5646024587428,-0.531669448515955,
4.05958515863483));
#37101=CARTESIAN_POINT('Ctrl Pts',(12.5882165748926,-0.496240142441994,
3.80008637217214));
#37102=CARTESIAN_POINT('Ctrl Pts',(12.6118306910425,-0.341887499674706,
3.58849794711368));
#37103=CARTESIAN_POINT('Ctrl Pts',(12.6354448071924,-0.105597250297878,
3.47552899021694));
#37104=CARTESIAN_POINT('Ctrl Pts',(12.6590589233422,0.155999231932725,3.4882530946792));
#37105=CARTESIAN_POINT('Ctrl Pts',(12.6826730394921,0.380209824197002,3.62362093815591));
#37106=CARTESIAN_POINT('Ctrl Pts',(12.706287155642,0.513300292941022,3.84919062944795));
#37107=CARTESIAN_POINT('Ctrl Pts',(12.7299012717918,0.52337486302099,4.11090284295443));
#37108=CARTESIAN_POINT('Ctrl Pts',(12.7535153879417,0.408018961865605,4.34603641497018));
#37109=CARTESIAN_POINT('Ctrl Pts',(12.7771295040916,0.194878495711741,4.49823995272895));
#37110=CARTESIAN_POINT('Ctrl Pts',(12.8007436202414,-0.0649659676909401,
4.53103681671432));
#37111=CARTESIAN_POINT('Ctrl Pts',(12.8243577363913,-0.30924088042124,4.43656701116699));
#37112=CARTESIAN_POINT('Ctrl Pts',(12.8479718525412,-0.479404065419363,
4.23747088215356));
#37113=CARTESIAN_POINT('Ctrl Pts',(12.871585968691,-0.534674727916345,3.9814632031866));
#37114=CARTESIAN_POINT('Ctrl Pts',(12.8952000848409,-0.461806870250484,
3.72989799658434));
#37115=CARTESIAN_POINT('Ctrl Pts',(12.9188142009908,-0.278263781132688,
3.54306461538724));
#37116=CARTESIAN_POINT('Ctrl Pts',(12.9424283171406,-0.0280328398727138,
3.46573897998727));
#37117=CARTESIAN_POINT('Ctrl Pts',(12.9660424332905,0.228916366652986,3.51645271720832));
#37118=CARTESIAN_POINT('Ctrl Pts',(12.9896565494404,0.431004172325429,3.68305192688505));
#37119=CARTESIAN_POINT('Ctrl Pts',(13.0132706655902,0.529798827743877,3.92560994866724));
#37120=CARTESIAN_POINT('Ctrl Pts',(13.0368847817401,0.501623505980173,4.1859960641053));
#37121=CARTESIAN_POINT('Ctrl Pts',(13.06049889789,0.353230619039521,4.40180692799916));
#37122=CARTESIAN_POINT('Ctrl Pts',(13.0841130140398,0.120183555287252,4.52132196448402));
#37123=CARTESIAN_POINT('Ctrl Pts',(13.1077271301897,-0.14166633412753,4.51589856308179));
#37124=CARTESIAN_POINT('Ctrl Pts',(13.1313412463396,-0.369564900381594,
4.38683647969259));
#37125=CARTESIAN_POINT('Ctrl Pts',(13.1549553624894,-0.508894665592834,
4.16506634104549));
#37126=CARTESIAN_POINT('Ctrl Pts',(13.1785694786393,-0.5262642816069,3.9037369046842));
#37127=CARTESIAN_POINT('Ctrl Pts',(13.2021835947892,-0.417510999030181,
3.66547758923531));
#37128=CARTESIAN_POINT('Ctrl Pts',(13.225797710939,-0.208698299100604,3.50738889824983));
#37129=CARTESIAN_POINT('Ctrl Pts',(13.2494118270889,0.0501304010278875,
3.46735788703128));
#37130=CARTESIAN_POINT('Ctrl Pts',(13.2730259432388,0.296945001575366,3.55497826608759));
#37131=CARTESIAN_POINT('Ctrl Pts',(13.2966400593886,0.472594665360713,3.74925120162283));
#37132=CARTESIAN_POINT('Ctrl Pts',(13.3202541755385,0.534983727701048,4.00361783223636));
#37133=CARTESIAN_POINT('Ctrl Pts',(13.3438682916884,0.469160215495142,4.25711742416948));
#37134=CARTESIAN_POINT('Ctrl Pts',(13.3674824078382,0.290899191662876,4.44899703551904));
#37135=CARTESIAN_POINT('Ctrl Pts',(13.3910965239881,0.0429221515009326,
4.53327138168622));
#37136=CARTESIAN_POINT('Ctrl Pts',(13.414710640138,-0.215341481063824,4.48974352894983));
#37137=CARTESIAN_POINT('Ctrl Pts',(13.4383247562878,-0.421997028626747,
4.32884523023027));
#37138=CARTESIAN_POINT('Ctrl Pts',(13.4619388724377,-0.527518050615216,
4.08913688288313));
#37139=CARTESIAN_POINT('Ctrl Pts',(13.4855529885876,-0.506615699542168,
3.82806626104107));
#37140=CARTESIAN_POINT('Ctrl Pts',(13.5091671047374,-0.364299369350597,
3.60820075662942));
#37141=CARTESIAN_POINT('Ctrl Pts',(13.5327812208873,-0.134676159283021,
3.48223266833859));
#37142=CARTESIAN_POINT('Ctrl Pts',(13.5563953370372,0.127223129883027,3.48035112543394));
#37143=CARTESIAN_POINT('Ctrl Pts',(13.580009453187,0.35863251032937,3.60300705277064));
#37144=CARTESIAN_POINT('Ctrl Pts',(13.6036235693369,0.504093113113068,3.82080510351303));
#37145=CARTESIAN_POINT('Ctrl Pts',(13.6272376854868,0.528744292176554,4.08154845863482));
#37146=CARTESIAN_POINT('Ctrl Pts',(13.6508518016366,0.426678220852065,4.32274815795836));
#37147=CARTESIAN_POINT('Ctrl Pts',(13.6744659177865,0.222355743648963,4.48659901446809));
#37148=CARTESIAN_POINT('Ctrl Pts',(13.6980800339364,-0.0352558354131549,
4.53383302978021));
#37149=CARTESIAN_POINT('Ctrl Pts',(13.7216941500862,-0.284418108090716,
4.45313024331322));
#37150=CARTESIAN_POINT('Ctrl Pts',(13.7453082662361,-0.465417601233682,
4.26383163964332));
#37151=CARTESIAN_POINT('Ctrl Pts',(13.768922382386,-0.534876526311652,4.01130394691162));
#37152=CARTESIAN_POINT('Ctrl Pts',(13.7925364985358,-0.476148568402614,
3.75606718461195));
#37153=CARTESIAN_POINT('Ctrl Pts',(13.8161506146857,-0.303308291444651,
3.55929061961886));
#37154=CARTESIAN_POINT('Ctrl Pts',(13.8397647308356,-0.0577780710103693,
3.46813312556118));
#37155=CARTESIAN_POINT('Ctrl Pts',(13.8633788469854,0.201599066354243,3.50444123046797));
#37156=CARTESIAN_POINT('Ctrl Pts',(13.8869929631353,0.412661584067771,3.65951344424533));
#37157=CARTESIAN_POINT('Ctrl Pts',(13.9106070792852,0.52482688048259,3.89618563135138));
#37158=CARTESIAN_POINT('Ctrl Pts',(13.934221195435,0.511213761492322,4.157737654591));
#37159=CARTESIAN_POINT('Ctrl Pts',(13.9578353115849,0.375084705828511,4.38148675084272));
#37160=CARTESIAN_POINT('Ctrl Pts',(13.9814494277348,0.149063989321389,4.51380989159668));
#37161=CARTESIAN_POINT('Ctrl Pts',(14.0050635438846,-0.112680949911453,
4.52299491502504));
#37162=CARTESIAN_POINT('Ctrl Pts',(14.0286776600345,-0.347421115087809,
4.40684056632315));
#37163=CARTESIAN_POINT('Ctrl Pts',(14.0522917761844,-0.498899391517477,
4.19318404374712));
#37164=CARTESIAN_POINT('Ctrl Pts',(14.0759058923342,-0.530812955762567,
3.93322962026762));
#37165=CARTESIAN_POINT('Ctrl Pts',(14.0995200084841,-0.435513499990629,
3.68927718310219));
#37166=CARTESIAN_POINT('Ctrl Pts',(14.123134124634,-0.235840202189154,3.51979163205294));
#37167=CARTESIAN_POINT('Ctrl Pts',(14.1467482407838,0.020353841830372,3.46539135927508));
#37168=CARTESIAN_POINT('Ctrl Pts',(14.1703623569337,0.271669945965271,3.53911376883853));
#37169=CARTESIAN_POINT('Ctrl Pts',(14.1939764730836,0.457878456363209,3.72329077208477));
#37170=CARTESIAN_POINT('Ctrl Pts',(14.2175905892334,0.534353207246894,3.97378306806742));
#37171=CARTESIAN_POINT('Ctrl Pts',(14.2412047053833,0.482766492200443,4.23055843429265));
#37172=CARTESIAN_POINT('Ctrl Pts',(14.2648188215332,0.315481426597312,4.4320788667444));
#37173=CARTESIAN_POINT('Ctrl Pts',(14.288432937683,0.0725890409372144,4.53004859093371));
#37174=CARTESIAN_POINT('Ctrl Pts',(14.3120470538329,-0.187699813700353,
4.50098848045824));
#37175=CARTESIAN_POINT('Ctrl Pts',(14.3356611699828,-0.40300510134274,4.35186299309067));
#37176=CARTESIAN_POINT('Ctrl Pts',(14.3592752861326,-0.521727410993515,
4.11841108999162));
#37177=CARTESIAN_POINT('Ctrl Pts',(14.3828894022825,-0.515414114678713,
3.85658114487643));
#37178=CARTESIAN_POINT('Ctrl Pts',(14.4065035184324,-0.385578237809175,
3.62912252677875));
#37179=CARTESIAN_POINT('Ctrl Pts',(14.4301176345822,-0.163335852108122,
3.49054727694211));
#37180=CARTESIAN_POINT('Ctrl Pts',(14.4537317507321,0.0980511075867261,
3.47406591865897));
#37181=CARTESIAN_POINT('Ctrl Pts',(14.477345866882,0.335939436781555,3.58362832417432));
#37182=CARTESIAN_POINT('Ctrl Pts',(14.5009599830318,0.493317541363497,3.79297710030521));
#37183=CARTESIAN_POINT('Ctrl Pts',(14.5245740991817,0.532468663007706,4.05194035550473));
#37184=CARTESIAN_POINT('Ctrl Pts',(14.5481882153316,0.444009962867018,4.2984557429324));
#37185=CARTESIAN_POINT('Ctrl Pts',(14.5718023314814,0.249141184223067,4.47344413391656));
#37186=CARTESIAN_POINT('Ctrl Pts',(14.5954164476313,-0.00543601357889273,
4.53496834239941));
#37187=CARTESIAN_POINT('Ctrl Pts',(14.6190305637812,-0.258710432878536,
4.46828366353805));
#37188=CARTESIAN_POINT('Ctrl Pts',(14.642644679931,-0.449983095981302,4.28937154481299));
#37189=CARTESIAN_POINT('Ctrl Pts',(14.6662587960809,-0.533414177619135,
4.0411095209942));
#37190=CARTESIAN_POINT('Ctrl Pts',(14.6898729122308,-0.489008838375032,
3.78299531421925));
#37191=CARTESIAN_POINT('Ctrl Pts',(14.7134870283806,-0.327409126727749,
3.57688779119022));
#37192=CARTESIAN_POINT('Ctrl Pts',(14.7371011445305,-0.0873435389344073,
3.47218205409647));
#37193=CARTESIAN_POINT('Ctrl Pts',(14.7607152606804,0.173654536592096,3.49397156277145));
#37194=CARTESIAN_POINT('Ctrl Pts',(14.7843293768302,0.393035092271916,3.63703430753458));
#37195=CARTESIAN_POINT('Ctrl Pts',(14.8079434929801,0.518222054789869,3.86708431049878));
#37196=CARTESIAN_POINT('Ctrl Pts',(14.8315576091299,0.519213488464815,4.12898847670818));
#37197=CARTESIAN_POINT('Ctrl Pts',(14.8551717252798,0.395771807832633,4.35997967156842));
#37198=CARTESIAN_POINT('Ctrl Pts',(14.8787858414297,0.177480631307892,4.50469920000947));
#37199=CARTESIAN_POINT('Ctrl Pts',(14.9023999575796,-0.0833449560929437,
4.52846412073519));
#37200=CARTESIAN_POINT('Ctrl Pts',(14.9260140737294,-0.324196468699902,
4.42557878841823));
#37201=CARTESIAN_POINT('Ctrl Pts',(14.9496281898793,-0.487351775161311,
4.22070085323907));
#37202=CARTESIAN_POINT('Ctrl Pts',(14.9732423060292,-0.533710406612102,
3.96292974457304));
#37203=CARTESIAN_POINT('Ctrl Pts',(14.996856422179,-0.452160410331013,3.71404423263127));
#37204=CARTESIAN_POINT('Ctrl Pts',(15.0204705383289,-0.262249669398955,
3.53368690291293));
#37205=CARTESIAN_POINT('Ctrl Pts',(15.0440846544788,-0.0094835464747447,
3.46509142247974));
#37206=CARTESIAN_POINT('Ctrl Pts',(15.0676987706286,0.245542447700007,3.52467627408104));
#37207=CARTESIAN_POINT('Ctrl Pts',(15.0913128867785,0.441743625625371,3.69820671204414));
#37208=CARTESIAN_POINT('Ctrl Pts',(15.1070556308784,0.501907244810829,3.86206650016617));
#37209=CARTESIAN_POINT('Ctrl Pts',(15.1149270029284,0.510765042839744,3.94627001497588));
#37210=CARTESIAN_POINT('Ctrl Pts',(12.4552189912149,0.227152124655503,4.39755682347243));
#37211=CARTESIAN_POINT('Ctrl Pts',(12.4630903632649,0.161611848667067,4.43500458455284));
#37212=CARTESIAN_POINT('Ctrl Pts',(12.4788331073648,0.0117126939868845,
4.476817784812));
#37213=CARTESIAN_POINT('Ctrl Pts',(12.5024472235147,-0.216038251184659,
4.42523583949706));
#37214=CARTESIAN_POINT('Ctrl Pts',(12.5260613396645,-0.391980722697534,
4.27174234332294));
#37215=CARTESIAN_POINT('Ctrl Pts',(12.5496754558144,-0.473999316058885,
4.05312196237532));
#37216=CARTESIAN_POINT('Ctrl Pts',(12.5732895719643,-0.442413023308054,
3.82177098359562));
#37217=CARTESIAN_POINT('Ctrl Pts',(12.5969036881141,-0.304802996424253,
3.6331335340607));
#37218=CARTESIAN_POINT('Ctrl Pts',(12.620517804264,-0.0941431270098475,
3.53241830873714));
#37219=CARTESIAN_POINT('Ctrl Pts',(12.6441319204139,0.139078010685439,3.54376223084778));
#37220=CARTESIAN_POINT('Ctrl Pts',(12.6677460365637,0.338968502198674,3.66444673774097));
#37221=CARTESIAN_POINT('Ctrl Pts',(12.6913601527136,0.457622660971028,3.86554890694496));
#37222=CARTESIAN_POINT('Ctrl Pts',(12.7149742688635,0.46660444343158,4.09887322255608));
#37223=CARTESIAN_POINT('Ctrl Pts',(12.7385883850133,0.36376118545685,4.30850187928827));
#37224=CARTESIAN_POINT('Ctrl Pts',(12.7622025011632,0.173740044570527,4.44419591437112));
#37225=CARTESIAN_POINT('Ctrl Pts',(12.7858166173131,-0.0579191156056905,
4.47343530576616));
#37226=CARTESIAN_POINT('Ctrl Pts',(12.809430733463,-0.275697552729921,4.38921263067613));
#37227=CARTESIAN_POINT('Ctrl Pts',(12.8330448496128,-0.42740315389367,4.2117124390707));
#37228=CARTESIAN_POINT('Ctrl Pts',(12.8566589657627,-0.476678613100171,
3.98347388770222));
#37229=CARTESIAN_POINT('Ctrl Pts',(12.8802730819125,-0.411714724743029,
3.75919593416074));
#37230=CARTESIAN_POINT('Ctrl Pts',(12.9038871980624,-0.248080536335154,
3.59262835132974));
#37231=CARTESIAN_POINT('Ctrl Pts',(12.9275013142123,-0.0249921205063485,
3.52369021994808));
#37232=CARTESIAN_POINT('Ctrl Pts',(12.9511154303621,0.204085831019768,3.5689030431123));
#37233=CARTESIAN_POINT('Ctrl Pts',(12.974729546512,0.384253192413122,3.71743125300502));
#37234=CARTESIAN_POINT('Ctrl Pts',(12.9983436626619,0.472331601336806,3.93367903017235));
#37235=CARTESIAN_POINT('Ctrl Pts',(13.0219577788117,0.44721245393608,4.16582108944128));
#37236=CARTESIAN_POINT('Ctrl Pts',(13.0455718949616,0.314915728754283,4.35822297028905));
#37237=CARTESIAN_POINT('Ctrl Pts',(13.0691860111115,0.107147256940744,4.46477422259573));
#37238=CARTESIAN_POINT('Ctrl Pts',(13.0928001272613,-0.126299800886535,
4.4599390970068));
#37239=CARTESIAN_POINT('Ctrl Pts',(13.1164142434112,-0.329478232215912,
4.34487636502855));
#37240=CARTESIAN_POINT('Ctrl Pts',(13.1400283595611,-0.453694911585238,
4.14716161137019));
#37241=CARTESIAN_POINT('Ctrl Pts',(13.1636424757109,-0.469180447069464,
3.9141785531052));
#37242=CARTESIAN_POINT('Ctrl Pts',(13.1872565918608,-0.372223622289685,
3.70176320202068));
#37243=CARTESIAN_POINT('Ctrl Pts',(13.2108707080107,-0.186060815253654,
3.56082237569912));
#37244=CARTESIAN_POINT('Ctrl Pts',(13.2344848241605,0.0446927613901878,
3.52513352430527));
#37245=CARTESIAN_POINT('Ctrl Pts',(13.2580989403104,0.26473540664544,3.60324972951781));
#37246=CARTESIAN_POINT('Ctrl Pts',(13.2817130564603,0.421332368785403,3.77644989896424));
#37247=CARTESIAN_POINT('Ctrl Pts',(13.3053271726101,0.476954095708811,4.00322540633176));
#37248=CARTESIAN_POINT('Ctrl Pts',(13.32894128876,0.418270453356816,4.22922792261873));
#37249=CARTESIAN_POINT('Ctrl Pts',(13.3525554049099,0.259345385135757,4.40029437151701));
#37250=CARTESIAN_POINT('Ctrl Pts',(13.3761695210597,0.0382663899759653,
4.47542748769673));
#37251=CARTESIAN_POINT('Ctrl Pts',(13.3997836372096,-0.19198341192685,4.43662109683837));
#37252=CARTESIAN_POINT('Ctrl Pts',(13.4233977533595,-0.376223052699929,
4.29317542065556));
#37253=CARTESIAN_POINT('Ctrl Pts',(13.4470118695093,-0.470298219877544,
4.07946821401937));
#37254=CARTESIAN_POINT('Ctrl Pts',(13.4706259856592,-0.451663144756522,
3.84671589668833));
#37255=CARTESIAN_POINT('Ctrl Pts',(13.4942401018091,-0.324783852814677,
3.65069918177841));
#37256=CARTESIAN_POINT('Ctrl Pts',(13.5178542179589,-0.120067849615538,
3.53839483955645));
#37257=CARTESIAN_POINT('Ctrl Pts',(13.5414683341088,0.113423249576877,3.53671738742444));
#37258=CARTESIAN_POINT('Ctrl Pts',(13.5650824502587,0.319731677430589,3.64606883846313));
#37259=CARTESIAN_POINT('Ctrl Pts',(13.5886965664085,0.449414183027706,3.84024235619866));
#37260=CARTESIAN_POINT('Ctrl Pts',(13.6123106825584,0.471391451138094,4.07270290539818));
#37261=CARTESIAN_POINT('Ctrl Pts',(13.6359247987083,0.380396476467901,4.28773969720951));
#37262=CARTESIAN_POINT('Ctrl Pts',(13.6595389148581,0.198236838143636,4.43381766753122));
#37263=CARTESIAN_POINT('Ctrl Pts',(13.683153031008,-0.0314316384354341,
4.47592821387755));
#37264=CARTESIAN_POINT('Ctrl Pts',(13.7067671471579,-0.253567304057185,
4.40397925067086));
#37265=CARTESIAN_POINT('Ctrl Pts',(13.7303812633077,-0.414933800093862,
4.23521384780468));
#37266=CARTESIAN_POINT('Ctrl Pts',(13.7539953794576,-0.476858522443512,
4.01007780890896));
#37267=CARTESIAN_POINT('Ctrl Pts',(13.7776094956075,-0.424500780316106,
3.78252655295316));
#37268=CARTESIAN_POINT('Ctrl Pts',(13.8012236117573,-0.270408471092428,
3.60709432248837));
#37269=CARTESIAN_POINT('Ctrl Pts',(13.8248377279072,-0.0515108893666192,
3.52582467278856));
#37270=CARTESIAN_POINT('Ctrl Pts',(13.8484518440571,0.179731635580624,3.55819444114981));
#37271=CARTESIAN_POINT('Ctrl Pts',(13.8720659602069,0.367900222888263,3.69644598724744));
#37272=CARTESIAN_POINT('Ctrl Pts',(13.8956800763568,0.467898960702838,3.90744636564338));
#37273=CARTESIAN_POINT('Ctrl Pts',(13.9192941925067,0.455762455382048,4.14062786681004));
#37274=CARTESIAN_POINT('Ctrl Pts',(13.9429083086565,0.33439930491234,4.34010692073752));
#37275=CARTESIAN_POINT('Ctrl Pts',(13.9665224248064,0.132895033153719,4.45807698351094));
#37276=CARTESIAN_POINT('Ctrl Pts',(13.9901365409563,-0.100458458427467,
4.46626570835715));
#37277=CARTESIAN_POINT('Ctrl Pts',(14.0137506571061,-0.309736381121202,
4.36271061036225));
#37278=CARTESIAN_POINT('Ctrl Pts',(14.037364773256,-0.444783823899526,4.1722293896428));
#37279=CARTESIAN_POINT('Ctrl Pts',(14.0609788894059,-0.473235726989685,
3.94047219674841));
#37280=CARTESIAN_POINT('Ctrl Pts',(14.0845930055557,-0.388273393752801,
3.72298125629644));
#37281=CARTESIAN_POINT('Ctrl Pts',(14.1082071217056,-0.210258638800633,
3.5718797861942));
#37282=CARTESIAN_POINT('Ctrl Pts',(14.1318212378555,0.0181460626216094,
3.52338030562014));
#37283=CARTESIAN_POINT('Ctrl Pts',(14.1554353540053,0.242201933815703,3.58910605271512));
#37284=CARTESIAN_POINT('Ctrl Pts',(14.1790494701552,0.40821242552128,3.75330539464867));
#37285=CARTESIAN_POINT('Ctrl Pts',(14.2026635863051,0.476391967745912,3.97662681607925));
#37286=CARTESIAN_POINT('Ctrl Pts',(14.2262777024549,0.430400858574612,4.20554978374509));
#37287=CARTESIAN_POINT('Ctrl Pts',(14.2498918186048,0.28126118747995,4.38521131483484));
#37288=CARTESIAN_POINT('Ctrl Pts',(14.2735059347547,0.0647153148514563,
4.47255427273816));
#37289=CARTESIAN_POINT('Ctrl Pts',(14.2971200509045,-0.167340033486385,
4.44664630956965));
#37290=CARTESIAN_POINT('Ctrl Pts',(14.3207341670544,-0.359291177888639,
4.31369644905674));
#37291=CARTESIAN_POINT('Ctrl Pts',(14.3443482832043,-0.465135690362464,
4.10556705078029));
#37292=CARTESIAN_POINT('Ctrl Pts',(14.3679623993541,-0.459507196674052,
3.87213777389641));
#37293=CARTESIAN_POINT('Ctrl Pts',(14.391576515504,-0.343754604517688,3.66935156959044));
#37294=CARTESIAN_POINT('Ctrl Pts',(14.4151906316539,-0.145618828396573,
3.5458075633877));
#37295=CARTESIAN_POINT('Ctrl Pts',(14.4388047478037,0.0874155136516737,
3.53111393640625));
#37296=CARTESIAN_POINT('Ctrl Pts',(14.4624188639536,0.299500119324396,3.6287921186396));
#37297=CARTESIAN_POINT('Ctrl Pts',(14.4860329801035,0.439807436479269,3.81543285374444));
#37298=CARTESIAN_POINT('Ctrl Pts',(14.5096470962533,0.474711839833821,4.04630639028407));
#37299=CARTESIAN_POINT('Ctrl Pts',(14.5332612124032,0.395848246141948,4.26608227803701));
#37300=CARTESIAN_POINT('Ctrl Pts',(14.5568753285531,0.22211686462983,4.42208969557108));
#37301=CARTESIAN_POINT('Ctrl Pts',(14.5804894447029,-0.00484636972403486,
4.47694037924932));
#37302=CARTESIAN_POINT('Ctrl Pts',(14.6041035608528,-0.230648137830783,
4.41748898090375));
#37303=CARTESIAN_POINT('Ctrl Pts',(14.6277176770027,-0.401173474098533,
4.25798344198848));
#37304=CARTESIAN_POINT('Ctrl Pts',(14.6513317931525,-0.475554794568933,
4.03665037532088));
#37305=CARTESIAN_POINT('Ctrl Pts',(14.6749459093024,-0.435966098077497,
3.80653379100725));
#37306=CARTESIAN_POINT('Ctrl Pts',(14.6985600254523,-0.291895091157815,
3.62278273060111));
#37307=CARTESIAN_POINT('Ctrl Pts',(14.7221741416021,-0.077869393911261,
3.52943441444639));
#37308=CARTESIAN_POINT('Ctrl Pts',(14.745788257752,0.15481824619589,3.54886041727207));
#37309=CARTESIAN_POINT('Ctrl Pts',(14.7694023739019,0.350402614714918,3.67640516027076));
#37310=CARTESIAN_POINT('Ctrl Pts',(14.7930164900517,0.462010559799276,3.88150166218328));
#37311=CARTESIAN_POINT('Ctrl Pts',(14.8166306062016,0.46289445276163,4.11499710940664));
#37312=CARTESIAN_POINT('Ctrl Pts',(14.8402447223515,0.352842479009638,4.32093271222338));
#37313=CARTESIAN_POINT('Ctrl Pts',(14.8638588385013,0.158229324796562,4.44995452773844));
#37314=CARTESIAN_POINT('Ctrl Pts',(14.8874729546512,-0.07430453695484,4.47114166986524));
#37315=CARTESIAN_POINT('Ctrl Pts',(14.9110870708011,-0.289030909828268,
4.37941629936134));
#37316=CARTESIAN_POINT('Ctrl Pts',(14.9347011869509,-0.434488776346555,
4.1967614535327));
#37317=CARTESIAN_POINT('Ctrl Pts',(14.9583153031008,-0.475818891632353,
3.96695075151007));
#37318=CARTESIAN_POINT('Ctrl Pts',(14.9819294192507,-0.403114615376237,
3.74506182641449));
#37319=CARTESIAN_POINT('Ctrl Pts',(15.0055435354005,-0.233803473716137,
3.58426783839933));
#37320=CARTESIAN_POINT('Ctrl Pts',(15.0291576515504,-0.00845486712728951,
3.5231129029393));
#37321=CARTESIAN_POINT('Ctrl Pts',(15.0527717677003,0.218908482701231,3.57623459158499));
#37322=CARTESIAN_POINT('Ctrl Pts',(15.0763858838501,0.393827738276586,3.73094220011788));
#37323=CARTESIAN_POINT('Ctrl Pts',(15.09212862795,0.447465415643859,3.87702813324079));
#37324=CARTESIAN_POINT('Ctrl Pts',(15.1,0.455362409197302,3.95209810113337));
#37325=CARTESIAN_POINT('',(15.1,0.455362409197302,3.95209810113338));
#37326=CARTESIAN_POINT('Ctrl Pts',(15.1,0.455362409197302,3.95209810113337));
#37327=CARTESIAN_POINT('Ctrl Pts',(15.1,0.461198486074795,3.93070554260298));
#37328=CARTESIAN_POINT('Ctrl Pts',(15.1,0.46535922191849,3.9089149747703));
#37329=CARTESIAN_POINT('Ctrl Pts',(15.1,0.467933495509747,3.88694781877637));
#37330=CARTESIAN_POINT('Ctrl Pts',(15.1,0.470556099470815,3.86456824322593));
#37331=CARTESIAN_POINT('Ctrl Pts',(15.1,0.471533159003394,3.84200460508655));
#37332=CARTESIAN_POINT('Ctrl Pts',(15.1,0.470938919222204,3.8194389967166));
#37333=CARTESIAN_POINT('Ctrl Pts',(15.1,0.470570970565677,3.80546654730098));
#37334=CARTESIAN_POINT('Ctrl Pts',(15.1,0.469600118414825,3.7914923521806));
#37335=CARTESIAN_POINT('Ctrl Pts',(15.1,0.468037922355437,3.77755218535593));
#37336=CARTESIAN_POINT('Ctrl Pts',(15.1,0.467305764617198,3.77101881782393));
#37337=CARTESIAN_POINT('Ctrl Pts',(15.1,0.466444065557791,3.76449770946228));
#37338=CARTESIAN_POINT('Ctrl Pts',(15.1,0.465455885979624,3.7580011302485));
#37339=CARTESIAN_POINT('Ctrl Pts',(15.1,0.462059294618766,3.73567095330476));
#37340=CARTESIAN_POINT('Ctrl Pts',(15.1,0.45716703427379,3.71360451488159));
#37341=CARTESIAN_POINT('Ctrl Pts',(15.1,0.450855318277529,3.69195899424001));
#37342=CARTESIAN_POINT('Ctrl Pts',(15.1,0.444011336009419,3.66848810937402));
#37343=CARTESIAN_POINT('Ctrl Pts',(15.1,0.435499564516811,3.64551127788848));
#37344=CARTESIAN_POINT('Ctrl Pts',(15.1,0.425460105602329,3.62314791088594));
#37345=CARTESIAN_POINT('Ctrl Pts',(15.1,0.421555366121865,3.61444992000866));
#37346=CARTESIAN_POINT('Ctrl Pts',(15.1,0.417417266816347,3.60584160863805));
#37347=CARTESIAN_POINT('Ctrl Pts',(15.1,0.413065612826793,3.5973533346642));
#37348=CARTESIAN_POINT('Ctrl Pts',(15.1,0.400188909388694,3.57223622128044));
#37349=CARTESIAN_POINT('Ctrl Pts',(15.1,0.385429835973237,3.54813135585314));
#37350=CARTESIAN_POINT('Ctrl Pts',(15.1,0.369010648251791,3.52520488756047));
#37351=CARTESIAN_POINT('Ctrl Pts',(15.1,0.352591460530346,3.50227841926781));
#37352=CARTESIAN_POINT('Ctrl Pts',(15.1,0.334512091502091,3.48052876229398));
#37353=CARTESIAN_POINT('Ctrl Pts',(15.1,0.31493781544227,3.46010549098216));
#37354=CARTESIAN_POINT('Ctrl Pts',(14.8800042915148,-1.01702808208336E-5,
4.45785711824254));
#37355=CARTESIAN_POINT('Ctrl Pts',(14.8824938458936,-0.0238866377941533,
4.45787702641871));
#37356=CARTESIAN_POINT('Ctrl Pts',(14.8849834002724,-0.0477600743578134,
4.45604121816599));
#37357=CARTESIAN_POINT('Ctrl Pts',(14.8874729546512,-0.0713366221418418,
4.45232291776013));
#37358=CARTESIAN_POINT('Ctrl Pts',(14.8953443267012,-0.145879994579315,
4.44056654636394));
#37359=CARTESIAN_POINT('Ctrl Pts',(14.9032156987511,-0.217455452203791,
4.40999142286264));
#37360=CARTESIAN_POINT('Ctrl Pts',(14.9110870708011,-0.277486158769077,
4.36426138680722));
#37361=CARTESIAN_POINT('Ctrl Pts',(14.918958442851,-0.337516865334364,4.31853135075179));
#37362=CARTESIAN_POINT('Ctrl Pts',(14.926829814901,-0.38600282084046,4.25764640214225));
#37363=CARTESIAN_POINT('Ctrl Pts',(14.9347011869509,-0.417134151141141,
4.18890214416703));
#37364=CARTESIAN_POINT('Ctrl Pts',(14.9425725590009,-0.448265481441821,
4.12015788619182));
#37365=CARTESIAN_POINT('Ctrl Pts',(14.9504439310508,-0.462042186537087,
4.04355431885095));
#37366=CARTESIAN_POINT('Ctrl Pts',(14.9583153031008,-0.456813159708701,
3.96827104766458));
#37367=CARTESIAN_POINT('Ctrl Pts',(14.9661866751508,-0.451584132880315,
3.89298777647821));
#37368=CARTESIAN_POINT('Ctrl Pts',(14.9740580472007,-0.427349374128277,
3.81902480144635));
#37369=CARTESIAN_POINT('Ctrl Pts',(14.9819294192507,-0.387013471142241,
3.7552443159279));
#37370=CARTESIAN_POINT('Ctrl Pts',(14.9898007913006,-0.346677568156205,
3.69146383040944));
#37371=CARTESIAN_POINT('Ctrl Pts',(14.9976721633506,-0.290240520936171,
3.63786583440439));
#37372=CARTESIAN_POINT('Ctrl Pts',(15.0055435354005,-0.224463896228013,
3.60087434715852));
#37373=CARTESIAN_POINT('Ctrl Pts',(15.0134149074505,-0.158687271519854,
3.56388285991266));
#37374=CARTESIAN_POINT('Ctrl Pts',(15.0212862795004,-0.0835710693235713,
3.54349788142598));
#37375=CARTESIAN_POINT('Ctrl Pts',(15.0291576515504,-0.00811907658734153,
3.54215900695692));
#37376=CARTESIAN_POINT('Ctrl Pts',(15.0370290236004,0.067332916148885,3.54082013248786));
#37377=CARTESIAN_POINT('Ctrl Pts',(15.0449003956503,0.143120699425059,3.55852736203643));
#37378=CARTESIAN_POINT('Ctrl Pts',(15.0527717677003,0.210167800325704,3.59316557823286));
#37379=CARTESIAN_POINT('Ctrl Pts',(15.0606431397502,0.27721490122635,3.62780379442929));
#37380=CARTESIAN_POINT('Ctrl Pts',(15.0685145118002,0.335521319751467,3.67937299727358));
#37381=CARTESIAN_POINT('Ctrl Pts',(15.0763858838501,0.378083948355844,3.74167908197646));
#37382=CARTESIAN_POINT('Ctrl Pts',(15.0842572559001,0.420646576960222,3.80398516667934));
#37383=CARTESIAN_POINT('Ctrl Pts',(15.09212862795,0.447465415643859,3.87702813324079));
#37384=CARTESIAN_POINT('Ctrl Pts',(15.1,0.455362409197302,3.95209810113337));
#37385=CARTESIAN_POINT('Ctrl Pts',(12.5,0.310062960217722,4.54266560670548));
#37386=CARTESIAN_POINT('Ctrl Pts',(12.5,0.283442099593322,4.54921865641189));
#37387=CARTESIAN_POINT('Ctrl Pts',(12.5,0.256466577744696,4.55390832200786));
#37388=CARTESIAN_POINT('Ctrl Pts',(12.5,0.229324391633413,4.55669460918752));
#37389=CARTESIAN_POINT('Ctrl Pts',(12.5,0.202804350211112,4.55941702996513));
#37390=CARTESIAN_POINT('Ctrl Pts',(12.5,0.176124140498118,4.56032157710196));
#37391=CARTESIAN_POINT('Ctrl Pts',(12.5,0.149491279718871,4.55933465732487));
#37392=CARTESIAN_POINT('Ctrl Pts',(12.5,0.131604301980395,4.55867182909064));
#37393=CARTESIAN_POINT('Ctrl Pts',(12.5,0.113739373486447,4.5571550748263));
#37394=CARTESIAN_POINT('Ctrl Pts',(12.5,0.0959711573489174,4.5547553284502));
#37395=CARTESIAN_POINT('Ctrl Pts',(12.5,0.0885102514788159,4.55374767063663));
#37396=CARTESIAN_POINT('Ctrl Pts',(12.5,0.0810658284660142,4.55258395860043));
#37397=CARTESIAN_POINT('Ctrl Pts',(12.5,0.0736590895785168,4.55126509319275));
#37398=CARTESIAN_POINT('Ctrl Pts',(12.5,0.0532014046082737,4.54762233847462));
#37399=CARTESIAN_POINT('Ctrl Pts',(12.5,0.0329999615976937,4.54279338637244));
#37400=CARTESIAN_POINT('Ctrl Pts',(12.5,0.0131662989716721,4.53674486487483));
#37401=CARTESIAN_POINT('Ctrl Pts',(12.5,-0.00550403753485725,4.53105111411095));
#37402=CARTESIAN_POINT('Ctrl Pts',(12.5,-0.0238485481480196,4.52427602479051));
#37403=CARTESIAN_POINT('Ctrl Pts',(12.5,-0.0417515783368052,4.51643454453567));
#37404=CARTESIAN_POINT('Ctrl Pts',(12.5,-0.0500477299146631,4.51280085190917));
#37405=CARTESIAN_POINT('Ctrl Pts',(12.5,-0.058248775177811,4.50893813195896));
#37406=CARTESIAN_POINT('Ctrl Pts',(12.5,-0.0663415323109863,4.50484786558969));
#37407=CARTESIAN_POINT('Ctrl Pts',(12.5,-0.0727048112135971,4.50163171746301));
#37408=CARTESIAN_POINT('Ctrl Pts',(12.5,-0.0789919703630761,4.49827952355299));
#37409=CARTESIAN_POINT('Ctrl Pts',(12.5,-0.085197598682301,4.4947927546146));
#37410=CARTESIAN_POINT('Ctrl Pts',(12.5,-0.104491803581693,4.48395188067351));
#37411=CARTESIAN_POINT('Ctrl Pts',(12.5,-0.123002674071495,4.47180959856144));
#37412=CARTESIAN_POINT('Ctrl Pts',(12.5,-0.140547257611399,4.45840101528927));
#37413=CARTESIAN_POINT('Ctrl Pts',(12.5,-0.156644205929787,4.44609879839914));
#37414=CARTESIAN_POINT('Ctrl Pts',(12.5,-0.17192740174072,4.43272977950413));
#37415=CARTESIAN_POINT('Ctrl Pts',(12.5,-0.186217277007305,4.41832740439832));
#37416=CARTESIAN_POINT('Origin',(15.1,0.,4.));
#37417=CARTESIAN_POINT('',(15.1,-1.16619037896906,2.5));
#37418=CARTESIAN_POINT('',(15.1,1.16619037896906,2.5));
#37419=CARTESIAN_POINT('',(15.1,1.25,2.5));
#37420=CARTESIAN_POINT('Origin',(15.1,0.,4.));
#37421=CARTESIAN_POINT('Origin',(15.1,0.,4.));
#37422=CARTESIAN_POINT('',(15.1,2.75545529808154E-17,5.725));
#37423=CARTESIAN_POINT('Origin',(15.1,0.,5.5));
#37424=CARTESIAN_POINT('',(15.1,1.5,4.225));
#37425=CARTESIAN_POINT('Origin',(15.1,1.5,4.));
#37426=CARTESIAN_POINT('',(15.1,-1.5,4.225));
#37427=CARTESIAN_POINT('Origin',(15.1,-1.5,4.));
#37428=CARTESIAN_POINT('Origin',(14.4,-1.5,4.));
#37429=CARTESIAN_POINT('',(14.5,-1.5,4.225));
#37430=CARTESIAN_POINT('Origin',(14.5,-1.5,4.));
#37431=CARTESIAN_POINT('',(14.4,-1.5,4.225));
#37432=CARTESIAN_POINT('Origin',(14.4,1.5,4.));
#37433=CARTESIAN_POINT('',(14.5,1.5,4.225));
#37434=CARTESIAN_POINT('Origin',(14.5,1.5,4.));
#37435=CARTESIAN_POINT('',(14.4,1.5,4.225));
#37436=CARTESIAN_POINT('Origin',(14.4,0.,5.5));
#37437=CARTESIAN_POINT('',(14.5,-2.75545529808154E-17,5.725));
#37438=CARTESIAN_POINT('Origin',(14.5,0.,5.5));
#37439=CARTESIAN_POINT('',(14.4,-2.75545529808154E-17,5.725));
#37440=CARTESIAN_POINT('Origin',(14.4,2.5,2.5));
#37441=CARTESIAN_POINT('',(14.5,1.16619037896906,2.5));
#37442=CARTESIAN_POINT('',(14.5,-1.16619037896906,2.5));
#37443=CARTESIAN_POINT('',(14.5,1.25,2.5));
#37444=CARTESIAN_POINT('',(14.5,1.16619037896906,2.5));
#37445=CARTESIAN_POINT('',(14.5,-1.16619037896906,2.5));
#37446=CARTESIAN_POINT('Origin',(14.5,0.,4.));
#37447=CARTESIAN_POINT('Origin',(14.5,0.,4.));
#37448=CARTESIAN_POINT('',(14.5,-1.34711147906209E-16,5.1));
#37449=CARTESIAN_POINT('Origin',(14.5,0.,4.));
#37450=CARTESIAN_POINT('Origin',(14.5,0.,4.));
#37451=CARTESIAN_POINT('Origin',(12.5,0.,4.));
#37452=CARTESIAN_POINT('Origin',(12.5,0.,4.));
#37453=CARTESIAN_POINT('',(12.5,-1.34711147906209E-16,5.1));
#37454=CARTESIAN_POINT('',(12.5,-1.34711147906209E-16,5.1));
#37455=CARTESIAN_POINT('Origin',(12.5,0.,4.));
#37456=CARTESIAN_POINT('Origin',(12.5,0.,4.));
#37457=CARTESIAN_POINT('',(0.,0.,0.));
#37458=CARTESIAN_POINT('Origin',(0.3,0.4,0.));
#37459=CARTESIAN_POINT('',(-0.3,0.4,-3.67394039744206E-17));
#37460=CARTESIAN_POINT('Origin',(0.,0.4,0.));
#37461=CARTESIAN_POINT('Origin',(0.,0.375,0.));
#37462=CARTESIAN_POINT('',(-0.35,0.35,-4.28626379701573E-17));
#37463=CARTESIAN_POINT('Origin',(0.,0.35,0.));
#37464=CARTESIAN_POINT('',(-0.325,0.375,-3.9801020972289E-17));
#37465=CARTESIAN_POINT('Origin',(0.,0.19,0.));
#37466=CARTESIAN_POINT('',(-0.35,0.03,-4.28626379701574E-17));
#37467=CARTESIAN_POINT('Origin',(0.,0.03,0.));
#37468=CARTESIAN_POINT('',(-0.35,0.19,-4.28626379701574E-17));
#37469=CARTESIAN_POINT('Origin',(0.,0.0149999999999999,0.));
#37470=CARTESIAN_POINT('',(-0.32,-3.29597460435593E-17,-3.91886975727153E-17));
#37471=CARTESIAN_POINT('Origin',(0.,0.,0.));
#37472=CARTESIAN_POINT('',(-0.335,0.0149999999999999,-4.10256677714363E-17));
#37473=CARTESIAN_POINT('Origin',(0.22,0.,0.));
#37474=CARTESIAN_POINT('',(-0.22,-6.93889390390723E-18,-2.69422295812418E-17));
#37475=CARTESIAN_POINT('Origin',(0.,0.,0.));
#37476=CARTESIAN_POINT('Origin',(0.,-0.02,0.));
#37477=CARTESIAN_POINT('',(-0.1954,-0.0492,2.39295984553393E-17));
#37478=CARTESIAN_POINT('Origin',(0.,-0.0492,0.));
#37479=CARTESIAN_POINT('',(-0.21,-0.02,-2.57175827820944E-17));
#37480=CARTESIAN_POINT('Origin',(0.,-0.8,0.));
#37481=CARTESIAN_POINT('',(-0.1954,-1.5646,2.39295984553393E-17));
#37482=CARTESIAN_POINT('Origin',(0.,-1.5646,0.));
#37483=CARTESIAN_POINT('',(-0.1954,-0.8,-2.39295984553393E-17));
#37484=CARTESIAN_POINT('Origin',(0.,-1.58,0.));
#37485=CARTESIAN_POINT('',(-0.16,-1.6,-1.95943487863577E-17));
#37486=CARTESIAN_POINT('Origin',(0.,-1.6,0.));
#37487=CARTESIAN_POINT('',(-0.18,-1.58,-2.20436423846524E-17));
#37488=CARTESIAN_POINT('Origin',(0.,-1.6,0.));
#37489=CARTESIAN_POINT('Origin',(0.0866025403784439,-0.4,-0.15));
#37490=CARTESIAN_POINT('',(0.173205080756888,-0.4,0.));
#37491=CARTESIAN_POINT('',(0.0866025403784439,-0.4,-0.15));
#37492=CARTESIAN_POINT('',(0.173205080756888,-0.4,0.));
#37493=CARTESIAN_POINT('',(0.0866025403784439,-0.64,-0.15));
#37494=CARTESIAN_POINT('',(0.0866025403784439,-0.4,-0.15));
#37495=CARTESIAN_POINT('',(0.173205080756888,-0.64,0.));
#37496=CARTESIAN_POINT('',(0.173205080756888,-0.64,0.));
#37497=CARTESIAN_POINT('',(0.173205080756888,-0.4,0.));
#37498=CARTESIAN_POINT('Origin',(-0.0866025403784438,-0.4,-0.15));
#37499=CARTESIAN_POINT('',(-0.0866025403784438,-0.4,-0.15));
#37500=CARTESIAN_POINT('',(0.0866025403784439,-0.4,-0.15));
#37501=CARTESIAN_POINT('',(-0.0866025403784438,-0.64,-0.15));
#37502=CARTESIAN_POINT('',(-0.0866025403784438,-0.4,-0.15));
#37503=CARTESIAN_POINT('',(0.0866025403784439,-0.64,-0.15));
#37504=CARTESIAN_POINT('Origin',(-0.173205080756888,-0.4,-2.77555756156289E-17));
#37505=CARTESIAN_POINT('',(-0.173205080756888,-0.4,-2.12115047744981E-17));
#37506=CARTESIAN_POINT('',(-0.0866025403784438,-0.4,-0.15));
#37507=CARTESIAN_POINT('',(-0.173205080756888,-0.64,-2.77555756156289E-17));
#37508=CARTESIAN_POINT('',(-0.173205080756888,-0.4,-2.12115047744981E-17));
#37509=CARTESIAN_POINT('',(-0.0866025403784438,-0.64,-0.15));
#37510=CARTESIAN_POINT('Origin',(-0.0866025403784439,-0.4,0.15));
#37511=CARTESIAN_POINT('',(-0.0866025403784439,-0.4,0.15));
#37512=CARTESIAN_POINT('',(-0.173205080756888,-0.4,-2.12115047744981E-17));
#37513=CARTESIAN_POINT('',(-0.0866025403784439,-0.64,0.15));
#37514=CARTESIAN_POINT('',(-0.0866025403784439,-0.4,0.15));
#37515=CARTESIAN_POINT('',(-0.173205080756888,-0.64,-2.12115047744981E-17));
#37516=CARTESIAN_POINT('Origin',(0.0866025403784439,-0.4,0.15));
#37517=CARTESIAN_POINT('',(0.0866025403784439,-0.4,0.15));
#37518=CARTESIAN_POINT('',(-0.0866025403784439,-0.4,0.15));
#37519=CARTESIAN_POINT('',(0.0866025403784439,-0.64,0.15));
#37520=CARTESIAN_POINT('',(0.0866025403784439,-0.4,0.15));
#37521=CARTESIAN_POINT('',(-0.0866025403784439,-0.64,0.15));
#37522=CARTESIAN_POINT('Origin',(0.173205080756888,-0.4,0.));
#37523=CARTESIAN_POINT('',(0.0866025403784439,-0.4,0.15));
#37524=CARTESIAN_POINT('',(0.0866025403784439,-0.64,0.15));
#37525=CARTESIAN_POINT('Origin',(0.,-0.4,-2.77555756156289E-17));
#37526=CARTESIAN_POINT('Origin',(0.,-0.64,-2.77555756156289E-17));
#37527=CARTESIAN_POINT('',(0.,0.,0.));
#37528=CARTESIAN_POINT('Origin',(0.375,0.5,0.));
#37529=CARTESIAN_POINT('',(-0.375,0.5,-4.59242549680257E-17));
#37530=CARTESIAN_POINT('Origin',(0.,0.5,0.));
#37531=CARTESIAN_POINT('Origin',(0.,0.475,0.));
#37532=CARTESIAN_POINT('',(-0.425,0.45,-5.20474889637625E-17));
#37533=CARTESIAN_POINT('Origin',(0.,0.45,0.));
#37534=CARTESIAN_POINT('',(-0.4,0.475,-4.89858719658941E-17));
#37535=CARTESIAN_POINT('Origin',(0.,0.24,0.));
#37536=CARTESIAN_POINT('',(-0.425,0.0299999999999998,-5.20474889637625E-17));
#37537=CARTESIAN_POINT('Origin',(0.,0.0299999999999998,0.));
#37538=CARTESIAN_POINT('',(-0.425,0.24,-5.20474889637625E-17));
#37539=CARTESIAN_POINT('Origin',(0.,0.0150000000000001,0.));
#37540=CARTESIAN_POINT('',(-0.395,4.85722573273506E-17,-4.83735485663204E-17));
#37541=CARTESIAN_POINT('Origin',(0.,0.,0.));
#37542=CARTESIAN_POINT('',(-0.41,0.0150000000000001,-5.02105187650415E-17));
#37543=CARTESIAN_POINT('Origin',(0.27,0.,0.));
#37544=CARTESIAN_POINT('',(-0.27,0.,-3.30654635769785E-17));
#37545=CARTESIAN_POINT('Origin',(0.,0.,0.));
#37546=CARTESIAN_POINT('Origin',(0.,-0.02,0.));
#37547=CARTESIAN_POINT('',(-0.24505,-0.0498999999999999,3.00099698131059E-17));
#37548=CARTESIAN_POINT('Origin',(0.,-0.0498999999999999,0.));
#37549=CARTESIAN_POINT('',(-0.26,-0.02,-3.18408167778312E-17));
#37550=CARTESIAN_POINT('Origin',(0.,-0.995,0.));
#37551=CARTESIAN_POINT('',(-0.24505,-1.95495,3.00099698131059E-17));
#37552=CARTESIAN_POINT('Origin',(0.,-1.95495,0.));
#37553=CARTESIAN_POINT('',(-0.24505,-0.995,-3.00099698131059E-17));
#37554=CARTESIAN_POINT('Origin',(0.,-1.975,0.));
#37555=CARTESIAN_POINT('',(-0.2,-2.,-2.44929359829471E-17));
#37556=CARTESIAN_POINT('Origin',(0.,-2.,0.));
#37557=CARTESIAN_POINT('',(-0.225,-1.975,-2.75545529808154E-17));
#37558=CARTESIAN_POINT('Origin',(0.,-2.,0.));
#37559=CARTESIAN_POINT('Origin',(0.115470053837925,-0.5,-0.2));
#37560=CARTESIAN_POINT('',(0.23094010767585,-0.5,0.));
#37561=CARTESIAN_POINT('',(0.115470053837925,-0.5,-0.2));
#37562=CARTESIAN_POINT('',(0.23094010767585,-0.5,0.));
#37563=CARTESIAN_POINT('',(0.115470053837925,-0.8,-0.2));
#37564=CARTESIAN_POINT('',(0.115470053837925,-0.5,-0.2));
#37565=CARTESIAN_POINT('',(0.23094010767585,-0.8,0.));
#37566=CARTESIAN_POINT('',(0.23094010767585,-0.8,0.));
#37567=CARTESIAN_POINT('',(0.23094010767585,-0.5,0.));
#37568=CARTESIAN_POINT('Origin',(-0.115470053837925,-0.5,-0.2));
#37569=CARTESIAN_POINT('',(-0.115470053837925,-0.5,-0.2));
#37570=CARTESIAN_POINT('',(0.115470053837925,-0.5,-0.2));
#37571=CARTESIAN_POINT('',(-0.115470053837925,-0.8,-0.2));
#37572=CARTESIAN_POINT('',(-0.115470053837925,-0.5,-0.2));
#37573=CARTESIAN_POINT('',(0.115470053837925,-0.8,-0.2));
#37574=CARTESIAN_POINT('Origin',(-0.23094010767585,-0.5,-2.77555756156289E-17));
#37575=CARTESIAN_POINT('',(-0.23094010767585,-0.5,-2.82820063659975E-17));
#37576=CARTESIAN_POINT('',(-0.115470053837925,-0.5,-0.2));
#37577=CARTESIAN_POINT('',(-0.23094010767585,-0.8,-2.77555756156289E-17));
#37578=CARTESIAN_POINT('',(-0.23094010767585,-0.5,-2.82820063659975E-17));
#37579=CARTESIAN_POINT('',(-0.115470053837925,-0.8,-0.2));
#37580=CARTESIAN_POINT('Origin',(-0.115470053837925,-0.5,0.2));
#37581=CARTESIAN_POINT('',(-0.115470053837925,-0.5,0.2));
#37582=CARTESIAN_POINT('',(-0.23094010767585,-0.5,-2.82820063659975E-17));
#37583=CARTESIAN_POINT('',(-0.115470053837925,-0.8,0.2));
#37584=CARTESIAN_POINT('',(-0.115470053837925,-0.5,0.2));
#37585=CARTESIAN_POINT('',(-0.23094010767585,-0.8,-2.82820063659975E-17));
#37586=CARTESIAN_POINT('Origin',(0.115470053837925,-0.5,0.2));
#37587=CARTESIAN_POINT('',(0.115470053837925,-0.5,0.2));
#37588=CARTESIAN_POINT('',(-0.115470053837925,-0.5,0.2));
#37589=CARTESIAN_POINT('',(0.115470053837925,-0.8,0.2));
#37590=CARTESIAN_POINT('',(0.115470053837925,-0.5,0.2));
#37591=CARTESIAN_POINT('',(-0.115470053837925,-0.8,0.2));
#37592=CARTESIAN_POINT('Origin',(0.23094010767585,-0.5,0.));
#37593=CARTESIAN_POINT('',(0.115470053837925,-0.5,0.2));
#37594=CARTESIAN_POINT('',(0.115470053837925,-0.8,0.2));
#37595=CARTESIAN_POINT('Origin',(0.,-0.5,0.));
#37596=CARTESIAN_POINT('Origin',(0.,-0.8,0.));
#37597=CARTESIAN_POINT('',(0.,0.,0.));
#37598=CARTESIAN_POINT('',(0.,0.,0.));
#37599=CARTESIAN_POINT('',(0.,0.,0.));
#37600=CARTESIAN_POINT('',(13.5,-6.,2.8));
#37601=CARTESIAN_POINT('',(12.,-7.9,7.2));
#37602=CARTESIAN_POINT('',(12.,-7.9,7.3));
#37603=CARTESIAN_POINT('',(12.,-4.1,7.2));
#37604=CARTESIAN_POINT('',(12.,-4.1,7.3));
#37605=CARTESIAN_POINT('',(15.,-7.9,7.2));
#37606=CARTESIAN_POINT('',(15.,-7.9,7.3));
#37607=CARTESIAN_POINT('',(15.,-4.1,7.2));
#37608=CARTESIAN_POINT('',(15.,-4.1,7.3));
#37609=CARTESIAN_POINT('',(0.,0.,0.));
#37610=CARTESIAN_POINT('',(15.1,-1.5,4.));
#37611=CARTESIAN_POINT('',(15.1,1.5,4.));
#37612=CARTESIAN_POINT('',(15.1,0.,5.5));
#37613=CARTESIAN_POINT('',(12.5,-1.5,7.2));
#37614=CARTESIAN_POINT('',(12.5,1.5,7.2));
#37615=CARTESIAN_POINT('',(14.,-1.5,7.2));
#37616=CARTESIAN_POINT('',(14.,1.5,7.2));
#37617=CARTESIAN_POINT('',(0.,0.,0.));
#37618=CARTESIAN_POINT('',(0.,0.,0.));
#37619=CARTESIAN_POINT('Origin',(4.,0.,4.));
#37620=CARTESIAN_POINT('',(4.12884541125756,8.40637486662632E-6,4.59405635738975));
#37621=CARTESIAN_POINT('',(4.02115458874249,-9.26662433349265E-6,4.59413599269206));
#37622=CARTESIAN_POINT('',(4.,-7.27562663373442E-17,4.5941));
#37623=CARTESIAN_POINT('',(4.,0.254721014554615,3.46322028700965));
#37624=CARTESIAN_POINT('Ctrl Pts',(4.12884541125756,8.40637486662632E-6,
4.59405635738975));
#37625=CARTESIAN_POINT('Ctrl Pts',(4.12564700130467,0.0398130654959074,
4.59407663624518));
#37626=CARTESIAN_POINT('Ctrl Pts',(4.12244859135178,0.079613792300143,4.59013569217808));
#37627=CARTESIAN_POINT('Ctrl Pts',(4.11925018139889,0.118599576779877,4.58219388355888));
#37628=CARTESIAN_POINT('Ctrl Pts',(4.11129754205509,0.215535206692688,4.56244709042845));
#37629=CARTESIAN_POINT('Ctrl Pts',(4.10334490271129,0.30743256945264,4.51796551073728));
#37630=CARTESIAN_POINT('Ctrl Pts',(4.09539226336748,0.383054411795556,4.45418672179759));
#37631=CARTESIAN_POINT('Ctrl Pts',(4.08743962402367,0.458676254138472,4.3904079328579));
#37632=CARTESIAN_POINT('Ctrl Pts',(4.07948698467986,0.518022576064352,4.30733193466969));
#37633=CARTESIAN_POINT('Ctrl Pts',(4.07153434533606,0.553840407547632,4.21511760274296));
#37634=CARTESIAN_POINT('Ctrl Pts',(4.06358170599225,0.589658239030912,4.12290327081622));
#37635=CARTESIAN_POINT('Ctrl Pts',(4.05562906664845,0.601947580071592,4.02155060515096));
#37636=CARTESIAN_POINT('Ctrl Pts',(4.04767642730464,0.589200356533535,3.92344812692479));
#37637=CARTESIAN_POINT('Ctrl Pts',(4.03972378796084,0.576453132995478,3.82534564869861));
#37638=CARTESIAN_POINT('Ctrl Pts',(4.03177114861703,0.538669344878685,3.73049335791153));
#37639=CARTESIAN_POINT('Ctrl Pts',(4.02381850927322,0.480479105222089,3.65049437695417));
#37640=CARTESIAN_POINT('Ctrl Pts',(4.01587900618215,0.422384984811151,3.57062753914914));
#37641=CARTESIAN_POINT('Ctrl Pts',(4.00793950309107,0.343951772361455,3.50556498199611));
#37642=CARTESIAN_POINT('Ctrl Pts',(4.,0.254721014554615,3.46322028700965));
#37643=CARTESIAN_POINT('',(4.,0.254694598474614,4.53673594206822));
#37644=CARTESIAN_POINT('Origin',(4.,0.,4.));
#37645=CARTESIAN_POINT('Ctrl Pts',(3.99999999999998,0.254694598474614,4.53673594206822));
#37646=CARTESIAN_POINT('Ctrl Pts',(4.00705152958082,0.175425736340139,4.5743509952638));
#37647=CARTESIAN_POINT('Ctrl Pts',(4.01410305916165,0.0876996967667308,
4.59405101338575));
#37648=CARTESIAN_POINT('Ctrl Pts',(4.02115458874249,-9.26662433349265E-6,
4.59413599269206));
#37649=CARTESIAN_POINT('Origin',(4.,0.,4.));
#37650=CARTESIAN_POINT('',(4.42884541125756,-2.46302091461148E-6,4.59415045696459));
#37651=CARTESIAN_POINT('',(4.32115458874249,3.58587963140688E-6,4.59404994535016));
#37652=CARTESIAN_POINT('',(4.,-7.27562663373442E-17,4.5941));
#37653=CARTESIAN_POINT('Ctrl Pts',(4.42884541125756,-2.46302091461148E-6,
4.59415045696459));
#37654=CARTESIAN_POINT('Ctrl Pts',(4.42107867343035,0.0966117732708647,
4.59412799973471));
#37655=CARTESIAN_POINT('Ctrl Pts',(4.41331193560314,0.193236775309615,4.57009608476161));
#37656=CARTESIAN_POINT('Ctrl Pts',(4.40554519777592,0.278573173318151,4.52479781884576));
#37657=CARTESIAN_POINT('Ctrl Pts',(4.39759255843212,0.36595214906825,4.47841531183407));
#37658=CARTESIAN_POINT('Ctrl Pts',(4.38963991908831,0.441495654419193,4.40973622444741));
#37659=CARTESIAN_POINT('Ctrl Pts',(4.3816872797445,0.495967466205845,4.32715751007026));
#37660=CARTESIAN_POINT('Ctrl Pts',(4.3737346404007,0.550439277992498,4.24457879569311));
#37661=CARTESIAN_POINT('Ctrl Pts',(4.36578200105689,0.58383939621486,4.14810045432546));
#37662=CARTESIAN_POINT('Ctrl Pts',(4.35782936171309,0.59208420294366,4.04951827803692));
#37663=CARTESIAN_POINT('Ctrl Pts',(4.34987672236928,0.600329009672459,3.95093610174838));
#37664=CARTESIAN_POINT('Ctrl Pts',(4.34192408302547,0.583418504907695,3.85025009053894));
#37665=CARTESIAN_POINT('Ctrl Pts',(4.33397144368167,0.54342022548472,3.75977047903001));
#37666=CARTESIAN_POINT('Ctrl Pts',(4.32601880433786,0.503421946061746,3.66929086752108));
#37667=CARTESIAN_POINT('Ctrl Pts',(4.31806616499406,0.440335891980562,3.58901765571266));
#37668=CARTESIAN_POINT('Ctrl Pts',(4.31011352565025,0.361875197644003,3.52876534000234));
#37669=CARTESIAN_POINT('Ctrl Pts',(4.30216088630644,0.283414503307443,3.46851302429202));
#37670=CARTESIAN_POINT('Ctrl Pts',(4.29420824696263,0.189579168715509,3.4282816046798));
#37671=CARTESIAN_POINT('Ctrl Pts',(4.28625560761883,0.0918418319479975,
3.41298991457491));
#37672=CARTESIAN_POINT('Ctrl Pts',(4.27830296827502,-0.00589550481951406,
3.39769822447003));
#37673=CARTESIAN_POINT('Ctrl Pts',(4.27035032893122,-0.107534843762603,
3.4073462638725));
#37674=CARTESIAN_POINT('Ctrl Pts',(4.26239768958741,-0.200649373295791,
3.44075443909651));
#37675=CARTESIAN_POINT('Ctrl Pts',(4.25444505024361,-0.293763902828979,
3.47416261432052));
#37676=CARTESIAN_POINT('Ctrl Pts',(4.24649241089979,-0.378353622952266,
3.53133092536608));
#37677=CARTESIAN_POINT('Ctrl Pts',(4.23853977155599,-0.444076322467606,
3.60526974769923));
#37678=CARTESIAN_POINT('Ctrl Pts',(4.23058713221218,-0.509799021982947,
3.67920857003239));
#37679=CARTESIAN_POINT('Ctrl Pts',(4.22263449286838,-0.556654700890342,
3.76991790365313));
#37680=CARTESIAN_POINT('Ctrl Pts',(4.21468185352458,-0.578914549750806,
3.86630733464992));
#37681=CARTESIAN_POINT('Ctrl Pts',(4.20672921418077,-0.601174398611269,
3.96269676564671));
#37682=CARTESIAN_POINT('Ctrl Pts',(4.19877657483696,-0.598838417424802,
4.06476629401955));
#37683=CARTESIAN_POINT('Ctrl Pts',(4.19082393549315,-0.5721923335546,4.16003645884502));
#37684=CARTESIAN_POINT('Ctrl Pts',(4.18287129614934,-0.545546249684398,
4.25530662367048));
#37685=CARTESIAN_POINT('Ctrl Pts',(4.17491865680554,-0.494590063130461,
4.34377742494856));
#37686=CARTESIAN_POINT('Ctrl Pts',(4.16696601746173,-0.425553631634784,
4.41463223618795));
#37687=CARTESIAN_POINT('Ctrl Pts',(4.15901337811793,-0.356517200139107,
4.48548704742733));
#37688=CARTESIAN_POINT('Ctrl Pts',(4.15106073877413,-0.269400523701689,
4.53872586862801));
#37689=CARTESIAN_POINT('Ctrl Pts',(4.14310809943032,-0.174855236950146,
4.56783927594351));
#37690=CARTESIAN_POINT('Ctrl Pts',(4.1383538700394,-0.118334381217266,4.5852437891806));
#37691=CARTESIAN_POINT('Ctrl Pts',(4.13359964064848,-0.0591586432141876,
4.59402621418361));
#37692=CARTESIAN_POINT('Ctrl Pts',(4.12884541125756,8.40637486662632E-6,
4.59405635738975));
#37693=CARTESIAN_POINT('Ctrl Pts',(4.02115458874249,-9.26662433349265E-6,
4.59413599269206));
#37694=CARTESIAN_POINT('Ctrl Pts',(4.02205569850546,-0.0112175303500608,
4.59414685213492));
#37695=CARTESIAN_POINT('Ctrl Pts',(4.02295680826843,-0.0224255152200988,
4.5938373961197));
#37696=CARTESIAN_POINT('Ctrl Pts',(4.0238579180314,-0.0336155370699344,
4.59320407706013));
#37697=CARTESIAN_POINT('Ctrl Pts',(4.03181055737521,-0.132371772633995,
4.58761479340425));
#37698=CARTESIAN_POINT('Ctrl Pts',(4.03976319671902,-0.229728915328813,
4.55680066053817));
#37699=CARTESIAN_POINT('Ctrl Pts',(4.04771583606282,-0.31374319278985,4.50455967689729));
#37700=CARTESIAN_POINT('Ctrl Pts',(4.05566847540663,-0.397757470250888,
4.4523186932564));
#37701=CARTESIAN_POINT('Ctrl Pts',(4.06362111475043,-0.468428882478145,
4.37865085884071));
#37702=CARTESIAN_POINT('Ctrl Pts',(4.07157375409424,-0.517135915630147,
4.29254879227412));
#37703=CARTESIAN_POINT('Ctrl Pts',(4.07952639343804,-0.565842948782149,
4.20644672570752));
#37704=CARTESIAN_POINT('Ctrl Pts',(4.08747903278185,-0.592585602858896,
4.10791042699003));
#37705=CARTESIAN_POINT('Ctrl Pts',(4.09543167212566,-0.594084460855775,
4.00899459728238));
#37706=CARTESIAN_POINT('Ctrl Pts',(4.10338431146947,-0.595583318852653,
3.91007876757474));
#37707=CARTESIAN_POINT('Ctrl Pts',(4.11133695081327,-0.571838380769662,
3.81078340687695));
#37708=CARTESIAN_POINT('Ctrl Pts',(4.11928959015708,-0.525757920758293,
3.72324489380985));
#37709=CARTESIAN_POINT('Ctrl Pts',(4.12724222950088,-0.479677460746923,
3.63570638074275));
#37710=CARTESIAN_POINT('Ctrl Pts',(4.13519486884469,-0.411261478807175,
3.55992471530633));
#37711=CARTESIAN_POINT('Ctrl Pts',(4.1431475081885,-0.328872047298013,3.50516726345229));
#37712=CARTESIAN_POINT('Ctrl Pts',(4.1511001475323,-0.246482615788851,3.45040981159825));
#37713=CARTESIAN_POINT('Ctrl Pts',(4.15905278687611,-0.150119734710276,
3.41667657332659));
#37714=CARTESIAN_POINT('Ctrl Pts',(4.16700542621992,-0.0515665150750243,
3.40809082437526));
#37715=CARTESIAN_POINT('Ctrl Pts',(4.17495806556372,0.0469867045602276,
3.39950507542393));
#37716=CARTESIAN_POINT('Ctrl Pts',(4.18291070490753,0.147730262752155,3.41606681579293));
#37717=CARTESIAN_POINT('Ctrl Pts',(4.19086334425134,0.238347648045887,3.45575171487277));
#37718=CARTESIAN_POINT('Ctrl Pts',(4.19881598359514,0.32896503333962,3.49543661395261));
#37719=CARTESIAN_POINT('Ctrl Pts',(4.20676862293895,0.409456245735157,3.55824467174328));
#37720=CARTESIAN_POINT('Ctrl Pts',(4.21472126228276,0.469979735422806,3.63649644709345));
#37721=CARTESIAN_POINT('Ctrl Pts',(4.22267390162656,0.530503225110456,3.71474822244363));
#37722=CARTESIAN_POINT('Ctrl Pts',(4.23062654097037,0.571058992090217,3.80844371535332));
#37723=CARTESIAN_POINT('Ctrl Pts',(4.23857918031417,0.586688754827568,3.90612753493601));
#37724=CARTESIAN_POINT('Ctrl Pts',(4.24653181965798,0.602318517564919,4.0038113545187));
#37725=CARTESIAN_POINT('Ctrl Pts',(4.25448445900178,0.593022276059861,4.10548350077438));
#37726=CARTESIAN_POINT('Ctrl Pts',(4.26243709834559,0.559936509464549,4.19871308474845));
#37727=CARTESIAN_POINT('Ctrl Pts',(4.2703897376894,0.526850742869238,4.29194266872251));
#37728=CARTESIAN_POINT('Ctrl Pts',(4.27834237703321,0.469975451183674,4.37672969041494));
#37729=CARTESIAN_POINT('Ctrl Pts',(4.28629501637701,0.396264473279151,4.44270782630825));
#37730=CARTESIAN_POINT('Ctrl Pts',(4.29424765572082,0.322553495374627,4.50868596220156));
#37731=CARTESIAN_POINT('Ctrl Pts',(4.30220029506462,0.232006831251144,4.55585521229574));
#37732=CARTESIAN_POINT('Ctrl Pts',(4.31015293440843,0.135695012128791,4.57844846968215));
#37733=CARTESIAN_POINT('Ctrl Pts',(4.31382015251978,0.0912825306677821,
4.58886694826517));
#37734=CARTESIAN_POINT('Ctrl Pts',(4.31748737063114,0.0456441298716245,
4.59405951624442));
#37735=CARTESIAN_POINT('Ctrl Pts',(4.32115458874249,3.58587963140688E-6,
4.59404994535016));
#37736=CARTESIAN_POINT('Origin',(4.,0.,4.));
#37737=CARTESIAN_POINT('',(4.72884541125756,-4.67700812217808E-6,4.59405084457266));
#37738=CARTESIAN_POINT('',(4.62115458874249,3.7232086238465E-6,4.59414939806979));
#37739=CARTESIAN_POINT('',(4.,-7.27562663373442E-17,4.5941));
#37740=CARTESIAN_POINT('Ctrl Pts',(4.72884541125756,-4.67700812217808E-6,
4.59405084457266));
#37741=CARTESIAN_POINT('Ctrl Pts',(4.72446298489983,0.0545367878429411,
4.59403588702548));
#37742=CARTESIAN_POINT('Ctrl Pts',(4.7200805585421,0.10908225468116,4.58659074407712));
#37743=CARTESIAN_POINT('Ctrl Pts',(4.71569813218437,0.16154350694756,4.57176871113812));
#37744=CARTESIAN_POINT('Ctrl Pts',(4.70774549284056,0.256743148594298,4.54487167450041));
#37745=CARTESIAN_POINT('Ctrl Pts',(4.69979285349676,0.345079446524661,4.4936824501733));
#37746=CARTESIAN_POINT('Ctrl Pts',(4.69184021415295,0.415752085200636,4.42445961801412));
#37747=CARTESIAN_POINT('Ctrl Pts',(4.68388757480915,0.486424723876611,4.35523678585494));
#37748=CARTESIAN_POINT('Ctrl Pts',(4.67593493546534,0.539433703298198,4.26798034586369));
#37749=CARTESIAN_POINT('Ctrl Pts',(4.66798229612153,0.568297953762936,4.17335858623793));
#37750=CARTESIAN_POINT('Ctrl Pts',(4.66002965677773,0.597162204227674,4.07873682661218));
#37751=CARTESIAN_POINT('Ctrl Pts',(4.65207701743392,0.601881725735563,3.97674974735193));
#37752=CARTESIAN_POINT('Ctrl Pts',(4.64412437809011,0.581879492504365,3.87986665793328));
#37753=CARTESIAN_POINT('Ctrl Pts',(4.63617173874631,0.561877259273167,3.78298356851463));
#37754=CARTESIAN_POINT('Ctrl Pts',(4.6282190994025,0.517153271302883,3.69120446893757));
#37755=CARTESIAN_POINT('Ctrl Pts',(4.6202664600587,0.453175645250056,3.61575060413089));
#37756=CARTESIAN_POINT('Ctrl Pts',(4.61231382071489,0.389198019197228,3.5402967393242));
#37757=CARTESIAN_POINT('Ctrl Pts',(4.60436118137108,0.305966755061857,3.48116810928789));
#37758=CARTESIAN_POINT('Ctrl Pts',(4.59640854202727,0.213658008474022,3.4455939943611));
#37759=CARTESIAN_POINT('Ctrl Pts',(4.58845590268347,0.121349261886187,3.41001987943431));
#37760=CARTESIAN_POINT('Ctrl Pts',(4.58050326333966,0.0199630328458878,
3.39800027961704));
#37761=CARTESIAN_POINT('Ctrl Pts',(4.57255062399586,-0.0781048312986516,
3.41100475468789));
#37762=CARTESIAN_POINT('Ctrl Pts',(4.56459798465205,-0.17617269544319,3.42400922975875));
#37763=CARTESIAN_POINT('Ctrl Pts',(4.55664534530825,-0.270922194691968,
3.46203777971774));
#37764=CARTESIAN_POINT('Ctrl Pts',(4.54869270596444,-0.350768912290741,
3.52044089639904));
#37765=CARTESIAN_POINT('Ctrl Pts',(4.54074006662063,-0.430615629889515,
3.57884401308035));
#37766=CARTESIAN_POINT('Ctrl Pts',(4.53278742727683,-0.495559565838284,
3.65762169648397));
#37767=CARTESIAN_POINT('Ctrl Pts',(4.52483478793302,-0.537660439465301,
3.74714230187364));
#37768=CARTESIAN_POINT('Ctrl Pts',(4.51688214858921,-0.579761313092318,
3.8366629072633));
#37769=CARTESIAN_POINT('Ctrl Pts',(4.50892950924541,-0.599019124397585,
3.936926434639));
#37770=CARTESIAN_POINT('Ctrl Pts',(4.5009768699016,-0.593079343631488,4.03567430223551));
#37771=CARTESIAN_POINT('Ctrl Pts',(4.49302423055779,-0.587139562865391,
4.13442216983203));
#37772=CARTESIAN_POINT('Ctrl Pts',(4.48507159121399,-0.556002190027932,
4.23165437764937));
#37773=CARTESIAN_POINT('Ctrl Pts',(4.47711895187018,-0.503474193090318,
4.31548296397124));
#37774=CARTESIAN_POINT('Ctrl Pts',(4.46916631252638,-0.450946196152703,
4.39931155029312));
#37775=CARTESIAN_POINT('Ctrl Pts',(4.46121367318257,-0.377027575114933,
4.46973651511953));
#37776=CARTESIAN_POINT('Ctrl Pts',(4.45326103383876,-0.290755888038263,
4.51814744739689));
#37777=CARTESIAN_POINT('Ctrl Pts',(4.44530839449495,-0.204484200961595,
4.56655837967425));
#37778=CARTESIAN_POINT('Ctrl Pts',(4.43735575515115,-0.105859447846027,
4.59295527940255));
#37779=CARTESIAN_POINT('Ctrl Pts',(4.42940311580734,-0.00693984821361558,
4.59411076594835));
#37780=CARTESIAN_POINT('Ctrl Pts',(4.42921721429075,-0.0046274959494805,
4.59413777669183));
#37781=CARTESIAN_POINT('Ctrl Pts',(4.42903131277416,-0.00231498256911503,
4.59415099449182));
#37782=CARTESIAN_POINT('Ctrl Pts',(4.42884541125756,-2.46302091461148E-6,
4.59415045696459));
#37783=CARTESIAN_POINT('Ctrl Pts',(4.32115458874249,3.58587963140688E-6,
4.59404994535016));
#37784=CARTESIAN_POINT('Ctrl Pts',(4.32544000997495,-0.0533308355660028,
4.59403876103764));
#37785=CARTESIAN_POINT('Ctrl Pts',(4.3297254312074,-0.106668183692779,4.58692369872924));
#37786=CARTESIAN_POINT('Ctrl Pts',(4.33401085243985,-0.158055593105036,
4.57274269264177));
#37787=CARTESIAN_POINT('Ctrl Pts',(4.34196349178366,-0.253417405095285,
4.54642639353635));
#37788=CARTESIAN_POINT('Ctrl Pts',(4.34991613112746,-0.342064054954561,
4.49577653064689));
#37789=CARTESIAN_POINT('Ctrl Pts',(4.35786877047127,-0.413157291282808,
4.42698573291487));
#37790=CARTESIAN_POINT('Ctrl Pts',(4.36582140981507,-0.484250527611055,
4.35819493518285));
#37791=CARTESIAN_POINT('Ctrl Pts',(4.37377404915888,-0.537790350408272,
4.27126320260829));
#37792=CARTESIAN_POINT('Ctrl Pts',(4.38172668850269,-0.567230782432438,
4.17681912699824));
#37793=CARTESIAN_POINT('Ctrl Pts',(4.3896793278465,-0.596671214456604,4.0823750513882));
#37794=CARTESIAN_POINT('Ctrl Pts',(4.3976319671903,-0.602012255707717,3.98041863274268));
#37795=CARTESIAN_POINT('Ctrl Pts',(4.40558460653411,-0.582600893642323,
3.88341542999892));
#37796=CARTESIAN_POINT('Ctrl Pts',(4.41353724587791,-0.563189531576929,
3.78641222725516));
#37797=CARTESIAN_POINT('Ctrl Pts',(4.42148988522172,-0.519025766195027,
3.69436224041317));
#37798=CARTESIAN_POINT('Ctrl Pts',(4.42944252456553,-0.455509217992651,
3.61851983504546));
#37799=CARTESIAN_POINT('Ctrl Pts',(4.43739516390933,-0.391992669790276,
3.54267742967776));
#37800=CARTESIAN_POINT('Ctrl Pts',(4.44534780325314,-0.309123338767427,
3.48304260578434));
#37801=CARTESIAN_POINT('Ctrl Pts',(4.45330044259694,-0.217033129998519,
3.44690653227429));
#37802=CARTESIAN_POINT('Ctrl Pts',(4.46125308194075,-0.12494292122961,3.41077045876423));
#37803=CARTESIAN_POINT('Ctrl Pts',(4.46920572128456,-0.0236318347146405,
3.39813313563753));
#37804=CARTESIAN_POINT('Ctrl Pts',(4.47715836062837,0.074513469760962,3.41053964803971));
#37805=CARTESIAN_POINT('Ctrl Pts',(4.48511099997217,0.172658774236564,3.42294616044189));
#37806=CARTESIAN_POINT('Ctrl Pts',(4.49306363931598,0.2676382966728,3.46039650837296));
#37807=CARTESIAN_POINT('Ctrl Pts',(4.50101627865978,0.34783949666059,3.51831187658845));
#37808=CARTESIAN_POINT('Ctrl Pts',(4.50896891800359,0.428040696648381,3.57622724480394));
#37809=CARTESIAN_POINT('Ctrl Pts',(4.51692155734739,0.493463574187728,3.65460763330386));
#37810=CARTESIAN_POINT('Ctrl Pts',(4.5248741966912,0.536109291561612,3.74386997215216));
#37811=CARTESIAN_POINT('Ctrl Pts',(4.53282683603501,0.578755008935497,3.83313231100046));
#37812=CARTESIAN_POINT('Ctrl Pts',(4.54077947537881,0.598623566143919,3.93327660019715));
#37813=CARTESIAN_POINT('Ctrl Pts',(4.54873211472262,0.593285761408823,4.03205883640902));
#37814=CARTESIAN_POINT('Ctrl Pts',(4.55668475406643,0.587947956673727,4.1308410726209));
#37815=CARTESIAN_POINT('Ctrl Pts',(4.56463739341024,0.557403789995114,4.22826125584796));
#37816=CARTESIAN_POINT('Ctrl Pts',(4.57259003275404,0.505387701781775,4.31240844187621));
#37817=CARTESIAN_POINT('Ctrl Pts',(4.58054267209785,0.453371613568435,4.39655562790445));
#37818=CARTESIAN_POINT('Ctrl Pts',(4.58849531144165,0.37988360382037,4.46742981673387));
#37819=CARTESIAN_POINT('Ctrl Pts',(4.59644795078546,0.293908582600447,4.51636567348148));
#37820=CARTESIAN_POINT('Ctrl Pts',(4.60440059012926,0.207933561380525,4.56530153022909));
#37821=CARTESIAN_POINT('Ctrl Pts',(4.61235322947307,0.109471528688745,4.59229905489488));
#37822=CARTESIAN_POINT('Ctrl Pts',(4.62030586881688,0.01056080905581,4.59405743239568));
#37823=CARTESIAN_POINT('Ctrl Pts',(4.62058877545875,0.00704216595801619,
4.59411998479525));
#37824=CARTESIAN_POINT('Ctrl Pts',(4.62087168210062,0.00352295504485493,
4.59415059693914));
#37825=CARTESIAN_POINT('Ctrl Pts',(4.62115458874249,3.7232086238465E-6,
4.59414939806979));
#37826=CARTESIAN_POINT('Origin',(4.,0.,4.));
#37827=CARTESIAN_POINT('',(5.02884541125756,1.1583539301252E-5,4.59413174414479));
#37828=CARTESIAN_POINT('',(4.92115458874249,-9.52916733652962E-6,4.59405847898621));
#37829=CARTESIAN_POINT('',(4.,-7.27562663373442E-17,4.5941));
#37830=CARTESIAN_POINT('Ctrl Pts',(5.02884541125756,1.1583539301252E-5,
4.59413174414479));
#37831=CARTESIAN_POINT('Ctrl Pts',(5.02784729636931,0.0124287555737821,
4.59414271605904));
#37832=CARTESIAN_POINT('Ctrl Pts',(5.02684918148107,0.024845254523583,4.59376142828251));
#37833=CARTESIAN_POINT('Ctrl Pts',(5.02585106659282,0.0372368329321061,
4.59298328977014));
#37834=CARTESIAN_POINT('Ctrl Pts',(5.01789842724901,0.135968707532707,4.58678334723719));
#37835=CARTESIAN_POINT('Ctrl Pts',(5.00994578790521,0.233118536601742,4.55538989360237));
#37836=CARTESIAN_POINT('Ctrl Pts',(5.0019931485614,0.316808430381418,4.50264120614281));
#37837=CARTESIAN_POINT('Ctrl Pts',(4.9940405092176,0.400498324161095,4.44989251868324));
#37838=CARTESIAN_POINT('Ctrl Pts',(4.98608786987379,0.470728282651411,4.37578859739892));
#37839=CARTESIAN_POINT('Ctrl Pts',(4.97813523052998,0.518911736914097,4.289389655942));
#37840=CARTESIAN_POINT('Ctrl Pts',(4.97018259118617,0.567095191176782,4.20299071448508));
#37841=CARTESIAN_POINT('Ctrl Pts',(4.96222995184237,0.593232141211837,4.10429675285556));
#37842=CARTESIAN_POINT('Ctrl Pts',(4.95427731249856,0.594126988899363,4.00537445204741));
#37843=CARTESIAN_POINT('Ctrl Pts',(4.94632467315476,0.595021836586889,3.90645215123927));
#37844=CARTESIAN_POINT('Ctrl Pts',(4.93837203381095,0.570674581926886,3.80730151125251));
#37845=CARTESIAN_POINT('Ctrl Pts',(4.93041939446714,0.524062008404491,3.72004504823011));
#37846=CARTESIAN_POINT('Ctrl Pts',(4.92246675512334,0.477449434882097,3.6327885852077));
#37847=CARTESIAN_POINT('Ctrl Pts',(4.91451411577953,0.408571542497308,3.55742629914966));
#37848=CARTESIAN_POINT('Ctrl Pts',(4.90656147643572,0.325849591692228,3.50317225594031));
#37849=CARTESIAN_POINT('Ctrl Pts',(4.89860883709192,0.243127640887147,3.44891821273095));
#37850=CARTESIAN_POINT('Ctrl Pts',(4.89065619774811,0.146561631661773,3.41577241237029));
#37851=CARTESIAN_POINT('Ctrl Pts',(4.88270355840431,0.0479580738465473,
3.40778738038914));
#37852=CARTESIAN_POINT('Ctrl Pts',(4.8747509190605,-0.0506454839686783,
3.39980234840799));
#37853=CARTESIAN_POINT('Ctrl Pts',(4.86679827971669,-0.151286590373755,
3.41697808480634));
#37854=CARTESIAN_POINT('Ctrl Pts',(4.85884564037289,-0.241660499406316,
3.45721462188069));
#37855=CARTESIAN_POINT('Ctrl Pts',(4.85089300102908,-0.332034408438876,
3.49745115895503));
#37856=CARTESIAN_POINT('Ctrl Pts',(4.84294036168527,-0.41214112009892,3.56074849670536));
#37857=CARTESIAN_POINT('Ctrl Pts',(4.83498772234147,-0.472186497854497,
3.63936767349926));
#37858=CARTESIAN_POINT('Ctrl Pts',(4.82703508299766,-0.532231875610076,
3.71798685029316));
#37859=CARTESIAN_POINT('Ctrl Pts',(4.81908244365386,-0.572215919461187,
3.81192786613063));
#37860=CARTESIAN_POINT('Ctrl Pts',(4.81112980431005,-0.587250035475296,
3.9097051523746));
#37861=CARTESIAN_POINT('Ctrl Pts',(4.80317716496624,-0.602284151489406,
4.00748243861856));
#37862=CARTESIAN_POINT('Ctrl Pts',(4.79522452562244,-0.592368339666514,
4.10909599526903));
#37863=CARTESIAN_POINT('Ctrl Pts',(4.78727188627863,-0.558714943052599,
4.20212218107662));
#37864=CARTESIAN_POINT('Ctrl Pts',(4.77931924693482,-0.525061546438685,
4.2951483668842));
#37865=CARTESIAN_POINT('Ctrl Pts',(4.77136660759101,-0.467670565033749,
4.37958718184891));
#37866=CARTESIAN_POINT('Ctrl Pts',(4.76341396824721,-0.393558827964045,
4.44511483080773));
#37867=CARTESIAN_POINT('Ctrl Pts',(4.7554613289034,-0.319447090894342,4.51064247976655));
#37868=CARTESIAN_POINT('Ctrl Pts',(4.7475086895596,-0.228614598159871,4.55725896271948));
#37869=CARTESIAN_POINT('Ctrl Pts',(4.73955605021579,-0.13216685911108,4.5792647797218));
#37870=CARTESIAN_POINT('Ctrl Pts',(4.73598583722972,-0.0888681559330128,
4.58914394690572));
#37871=CARTESIAN_POINT('Ctrl Pts',(4.73241562424364,-0.0444377444908,4.59406302997518));
#37872=CARTESIAN_POINT('Ctrl Pts',(4.72884541125756,-4.67700812217808E-6,
4.59405084457266));
#37873=CARTESIAN_POINT('Ctrl Pts',(4.62115458874249,3.7232086238465E-6,
4.59414939806979));
#37874=CARTESIAN_POINT('Ctrl Pts',(4.62882432144443,-0.0954043143036648,
4.59411689615543));
#37875=CARTESIAN_POINT('Ctrl Pts',(4.63649405414636,-0.190827729806029,
4.57070400848325));
#37876=CARTESIAN_POINT('Ctrl Pts',(4.6441637868483,-0.275369369969159,4.52648596729292));
#37877=CARTESIAN_POINT('Ctrl Pts',(4.65211642619211,-0.363029422787103,
4.48063689435358));
#37878=CARTESIAN_POINT('Ctrl Pts',(4.66006906553591,-0.438990121848901,
4.4124195181391));
#37879=CARTESIAN_POINT('Ctrl Pts',(4.66802170487971,-0.493964237128006,
4.33017434199545));
#37880=CARTESIAN_POINT('Ctrl Pts',(4.67597434422352,-0.548938352407109,
4.24792916585179));
#37881=CARTESIAN_POINT('Ctrl Pts',(4.68392698356733,-0.582925883903521,
4.15165618977896));
#37882=CARTESIAN_POINT('Ctrl Pts',(4.69187962291114,-0.591771392992132,
4.05312609631255));
#37883=CARTESIAN_POINT('Ctrl Pts',(4.69983226225494,-0.600616902080743,
3.95459600284613));
#37884=CARTESIAN_POINT('Ctrl Pts',(4.70778490159875,-0.584320388761555,
3.85380879198612));
#37885=CARTESIAN_POINT('Ctrl Pts',(4.71573754094256,-0.544874323741249,
3.76308707295491));
#37886=CARTESIAN_POINT('Ctrl Pts',(4.72369018028636,-0.505428258720944,
3.6723653539237));
#37887=CARTESIAN_POINT('Ctrl Pts',(4.73164281963017,-0.442832641999522,
3.59170912672127));
#37888=CARTESIAN_POINT('Ctrl Pts',(4.73959545897397,-0.364740640256699,
3.53097971363863));
#37889=CARTESIAN_POINT('Ctrl Pts',(4.74754809831778,-0.286648638513876,
3.47025030055599));
#37890=CARTESIAN_POINT('Ctrl Pts',(4.75550073766158,-0.193060251749651,
3.42944770159313));
#37891=CARTESIAN_POINT('Ctrl Pts',(4.76345337700539,-0.095417934894009,
3.41356059019365));
#37892=CARTESIAN_POINT('Ctrl Pts',(4.7714060163492,0.00222438196163176,
3.39767347879416));
#37893=CARTESIAN_POINT('Ctrl Pts',(4.77935865569301,0.10392062890869,3.40670185495805));
#37894=CARTESIAN_POINT('Ctrl Pts',(4.78731129503681,0.19723705468272,3.43954187673519));
#37895=CARTESIAN_POINT('Ctrl Pts',(4.79526393438062,0.290553480456751,3.47238189851233));
#37896=CARTESIAN_POINT('Ctrl Pts',(4.80321657372443,0.375490085057754,3.52903356590271));
#37897=CARTESIAN_POINT('Ctrl Pts',(4.81116921306823,0.441662211759978,3.60257044098769));
#37898=CARTESIAN_POINT('Ctrl Pts',(4.81912185241204,0.507834338462201,3.67610731607267));
#37899=CARTESIAN_POINT('Ctrl Pts',(4.82707449175584,0.555241987265645,3.76652939885225));
#37900=CARTESIAN_POINT('Ctrl Pts',(4.83502713109965,0.57808892742485,3.86278135818256));
#37901=CARTESIAN_POINT('Ctrl Pts',(4.84297977044346,0.600935867584054,3.95903331751286));
#37902=CARTESIAN_POINT('Ctrl Pts',(4.85093240978726,0.599222099099018,4.0611151533939));
#37903=CARTESIAN_POINT('Ctrl Pts',(4.85888504913107,0.573157153508111,4.15654597106253));
#37904=CARTESIAN_POINT('Ctrl Pts',(4.86683768847488,0.547092207917203,4.25197678873116));
#37905=CARTESIAN_POINT('Ctrl Pts',(4.87479032781868,0.496676085220424,4.34075658818739));
#37906=CARTESIAN_POINT('Ctrl Pts',(4.88274296716249,0.428072843071251,4.41203082979109));
#37907=CARTESIAN_POINT('Ctrl Pts',(4.89069560650629,0.359469600922078,4.48330507139479));
#37908=CARTESIAN_POINT('Ctrl Pts',(4.8986482458501,0.272679239320511,4.53707375514596));
#37909=CARTESIAN_POINT('Ctrl Pts',(4.90660088519391,0.178313062033339,4.56676292714126));
#37910=CARTESIAN_POINT('Ctrl Pts',(4.9114521197101,0.120748216373203,4.58487378690922));
#37911=CARTESIAN_POINT('Ctrl Pts',(4.9163033542263,0.0603642649825261,4.59402420038378));
#37912=CARTESIAN_POINT('Ctrl Pts',(4.92115458874249,-9.52916733652962E-6,
4.59405847898621));
#37913=CARTESIAN_POINT('Origin',(4.,0.,4.));
#37914=CARTESIAN_POINT('',(5.32884541125756,-1.45357002139801E-5,4.59407911932661));
#37915=CARTESIAN_POINT('',(5.22115458874249,1.46139895546772E-5,4.59411444380891));
#37916=CARTESIAN_POINT('',(4.,-7.27562663373442E-17,4.5941));
#37917=CARTESIAN_POINT('Ctrl Pts',(5.32884541125756,-1.45357002139801E-5,
4.59407911932661));
#37918=CARTESIAN_POINT('Ctrl Pts',(5.32327896849499,0.0692531541268509,
4.59401614001471));
#37919=CARTESIAN_POINT('Ctrl Pts',(5.31771252573242,0.138542285837495,4.5819075943171));
#37920=CARTESIAN_POINT('Ctrl Pts',(5.31214608296985,0.203593590158122,4.55818044906639));
#37921=CARTESIAN_POINT('Ctrl Pts',(5.30419344362604,0.296530782575621,4.5242820624512));
#37922=CARTESIAN_POINT('Ctrl Pts',(5.29624080428224,0.380818089806801,4.46666879957728));
#37923=CARTESIAN_POINT('Ctrl Pts',(5.28828816493843,0.446150240572578,4.39238466650784));
#37924=CARTESIAN_POINT('Ctrl Pts',(5.28033552559462,0.511482391338355,4.3181005334384));
#37925=CARTESIAN_POINT('Ctrl Pts',(5.27238288625081,0.557859385638729,4.22714553017344));
#37926=CARTESIAN_POINT('Ctrl Pts',(5.26443024690701,0.579611004278495,4.13064014464439));
#37927=CARTESIAN_POINT('Ctrl Pts',(5.2564776075632,0.601362622918262,4.03413475911534));
#37928=CARTESIAN_POINT('Ctrl Pts',(5.2485249682194,0.598488865897423,3.93207899132219));
#37929=CARTESIAN_POINT('Ctrl Pts',(5.24057232887559,0.571341089151559,3.8369505488493));
#37930=CARTESIAN_POINT('Ctrl Pts',(5.23261968953179,0.544193312405696,3.74182210637642));
#37931=CARTESIAN_POINT('Ctrl Pts',(5.22466705018798,0.492771515934809,3.65362098922379));
#37932=CARTESIAN_POINT('Ctrl Pts',(5.21671441084417,0.423362714708271,3.58313098523844));
#37933=CARTESIAN_POINT('Ctrl Pts',(5.20876177150037,0.353953913481732,3.51264098125308));
#37934=CARTESIAN_POINT('Ctrl Pts',(5.20080913215656,0.266558107499543,3.45986209043499));
#37935=CARTESIAN_POINT('Ctrl Pts',(5.19285649281275,0.171860624350003,3.43124725102074));
#37936=CARTESIAN_POINT('Ctrl Pts',(5.18490385346895,0.0771631412004631,
3.40263241160649));
#37937=CARTESIAN_POINT('Ctrl Pts',(5.17695121412514,-0.0248360191164267,
3.39818162359609));
#37938=CARTESIAN_POINT('Ctrl Pts',(5.16899857478133,-0.121666070051256,
3.41843905644231));
#37939=CARTESIAN_POINT('Ctrl Pts',(5.16104593543753,-0.218496120986084,
3.43869648928852));
#37940=CARTESIAN_POINT('Ctrl Pts',(5.15309329609372,-0.310157062538852,
3.48366214299137));
#37941=CARTESIAN_POINT('Ctrl Pts',(5.14514065674991,-0.385442096207774,
3.54783835396576));
#37942=CARTESIAN_POINT('Ctrl Pts',(5.13718801740611,-0.460727129876697,
3.61201456494015));
#37943=CARTESIAN_POINT('Ctrl Pts',(5.1292353780623,-0.519636255661773,3.6954013331861));
#37944=CARTESIAN_POINT('Ctrl Pts',(5.1212827387185,-0.554967030609594,3.78780349058054));
#37945=CARTESIAN_POINT('Ctrl Pts',(5.11333009937469,-0.590297805557415,
3.88020564797498));
#37946=CARTESIAN_POINT('Ctrl Pts',(5.10537746003088,-0.60205022966798,3.98162319451792));
#37947=CARTESIAN_POINT('Ctrl Pts',(5.09742482068708,-0.588787409028971,
4.07965645386523));
#37948=CARTESIAN_POINT('Ctrl Pts',(5.08947218134327,-0.575524588389962,
4.17768971321255));
#37949=CARTESIAN_POINT('Ctrl Pts',(5.08151954199946,-0.537246523001379,
4.27233868536424));
#37950=CARTESIAN_POINT('Ctrl Pts',(5.07356690265566,-0.47863322769376,4.35203124438164));
#37951=CARTESIAN_POINT('Ctrl Pts',(5.06561426331185,-0.42001993238614,4.43172380339905));
#37952=CARTESIAN_POINT('Ctrl Pts',(5.05766162396805,-0.341071407159484,
4.49645994928216));
#37953=CARTESIAN_POINT('Ctrl Pts',(5.04970898462424,-0.251440184480074,
4.53832480650817));
#37954=CARTESIAN_POINT('Ctrl Pts',(5.04275446016868,-0.1730583412759,4.5749353153996));
#37955=CARTESIAN_POINT('Ctrl Pts',(5.03579993571312,-0.0865070403179845,
4.59405529558476));
#37956=CARTESIAN_POINT('Ctrl Pts',(5.02884541125756,1.1583539301252E-5,
4.59413174414479));
#37957=CARTESIAN_POINT('Ctrl Pts',(4.92115458874249,-9.52916733652962E-6,
4.59405847898621));
#37958=CARTESIAN_POINT('Ctrl Pts',(4.9242559935701,-0.0386066277022544,
4.59408039337166));
#37959=CARTESIAN_POINT('Ctrl Pts',(4.92735739839772,-0.0771995748988638,
4.59037647703175));
#37960=CARTESIAN_POINT('Ctrl Pts',(4.93045880322533,-0.115049119822012,
4.58290605049323));
#37961=CARTESIAN_POINT('Ctrl Pts',(4.93841144256913,-0.212103131417409,
4.56375034161047));
#37962=CARTESIAN_POINT('Ctrl Pts',(4.94636408191294,-0.304269161635426,
4.51982926360553));
#37963=CARTESIAN_POINT('Ctrl Pts',(4.95431672125675,-0.380278658005779,
4.45651276645759));
#37964=CARTESIAN_POINT('Ctrl Pts',(4.96226936060055,-0.456288154376132,
4.39319626930964));
#37965=CARTESIAN_POINT('Ctrl Pts',(4.97022199994436,-0.516141116898821,
4.31048435301868));
#37966=CARTESIAN_POINT('Ctrl Pts',(4.97817463928816,-0.552519705724467,
4.21848967586497));
#37967=CARTESIAN_POINT('Ctrl Pts',(4.98612727863197,-0.588898294550112,
4.12649499871126));
#37968=CARTESIAN_POINT('Ctrl Pts',(4.99407991797578,-0.601802509678713,
4.0252175606948));
#37969=CARTESIAN_POINT('Ctrl Pts',(5.00203255731958,-0.589654635058918,
3.92703990798411));
#37970=CARTESIAN_POINT('Ctrl Pts',(5.00998519666339,-0.577506760439122,
3.82886225527341));
#37971=CARTESIAN_POINT('Ctrl Pts',(5.0179378360072,-0.540306796070929,3.73378438786847));
#37972=CARTESIAN_POINT('Ctrl Pts',(5.025890475351,-0.482602944251693,3.65343086999412));
#37973=CARTESIAN_POINT('Ctrl Pts',(5.03384311469481,-0.424899092432456,
3.57307735211977));
#37974=CARTESIAN_POINT('Ctrl Pts',(5.04179575403862,-0.346691353162178,
3.50744818377599));
#37975=CARTESIAN_POINT('Ctrl Pts',(5.04974839338242,-0.257541687734669,
3.46456742464414));
#37976=CARTESIAN_POINT('Ctrl Pts',(5.05770103272623,-0.16839202230716,3.42168666551229));
#37977=CARTESIAN_POINT('Ctrl Pts',(5.06565367207003,-0.0683004307224215,
3.40155431559236));
#37978=CARTESIAN_POINT('Ctrl Pts',(5.07360631141384,0.0304955267282049,
3.40663182885918));
#37979=CARTESIAN_POINT('Ctrl Pts',(5.08155895075765,0.129291484178831,3.41170934212599));
#37980=CARTESIAN_POINT('Ctrl Pts',(5.08951159010146,0.226791807495345,3.44199671857955));
#37981=CARTESIAN_POINT('Ctrl Pts',(5.09746422944526,0.311075754224562,3.49379091394262));
#37982=CARTESIAN_POINT('Ctrl Pts',(5.10541686878907,0.395359700953779,3.54558510930568));
#37983=CARTESIAN_POINT('Ctrl Pts',(5.11336950813287,0.466427271095698,3.61888612357825));
#37984=CARTESIAN_POINT('Ctrl Pts',(5.12132214747668,0.515589486279599,3.70473190942573));
#37985=CARTESIAN_POINT('Ctrl Pts',(5.12927478682048,0.564751701463499,3.79057769527322));
#37986=CARTESIAN_POINT('Ctrl Pts',(5.13722742616429,0.592008561689381,3.88896825269562));
#37987=CARTESIAN_POINT('Ctrl Pts',(5.1451800655081,0.594027544563649,3.98787399599556));
#37988=CARTESIAN_POINT('Ctrl Pts',(5.1531327048519,0.596046527437917,4.0867797392955));
#37989=CARTESIAN_POINT('Ctrl Pts',(5.16108534419571,0.572827632960568,4.18620066847299));
#37990=CARTESIAN_POINT('Ctrl Pts',(5.16903798353952,0.527209687216453,4.2739812208502));
#37991=CARTESIAN_POINT('Ctrl Pts',(5.17699062288332,0.481591741472338,4.3617617732274));
#37992=CARTESIAN_POINT('Ctrl Pts',(5.18494326222713,0.413574744461461,4.43790194880433));
#37993=CARTESIAN_POINT('Ctrl Pts',(5.19289590157094,0.331474700441294,4.49309257410834));
#37994=CARTESIAN_POINT('Ctrl Pts',(5.20084854091474,0.24937465642113,4.54828319941234));
#37995=CARTESIAN_POINT('Ctrl Pts',(5.20880118025855,0.153191565391677,4.58252427444343));
#37996=CARTESIAN_POINT('Ctrl Pts',(5.21675381960235,0.0546851202186884,
4.59162936142496));
#37997=CARTESIAN_POINT('Ctrl Pts',(5.21822074264906,0.0365148790664279,
4.59330886194775));
#37998=CARTESIAN_POINT('Ctrl Pts',(5.21968766569578,0.018265586889787,4.59413312238171));
#37999=CARTESIAN_POINT('Ctrl Pts',(5.22115458874249,1.46139895546772E-5,
4.59411444380891));
#38000=CARTESIAN_POINT('Origin',(4.,0.,4.));
#38001=CARTESIAN_POINT('',(5.62884541125756,1.52328526200479E-5,4.59408648697874));
#38002=CARTESIAN_POINT('',(5.52115458874249,-1.55733839743342E-5,4.59409663347568));
#38003=CARTESIAN_POINT('',(4.,-7.27562663373442E-17,4.5941));
#38004=CARTESIAN_POINT('Ctrl Pts',(5.62884541125756,1.52328526200479E-5,
4.59408648697874));
#38005=CARTESIAN_POINT('Ctrl Pts',(5.62666327996447,0.0271682673899915,
4.59411287463303));
#38006=CARTESIAN_POINT('Ctrl Pts',(5.62448114867138,0.054317778225707,4.59228554395034));
#38007=CARTESIAN_POINT('Ctrl Pts',(5.62229901737829,0.0812075234320336,
4.58857548522516));
#38008=CARTESIAN_POINT('Ctrl Pts',(5.61434637803449,0.179205497408217,4.57505441109036));
#38009=CARTESIAN_POINT('Ctrl Pts',(5.60639373869068,0.273753285393806,4.53652709601604));
#38010=CARTESIAN_POINT('Ctrl Pts',(5.59844109934688,0.353291132582354,4.47770402899113));
#38011=CARTESIAN_POINT('Ctrl Pts',(5.59048846000307,0.432828979770902,4.41888096196622));
#38012=CARTESIAN_POINT('Ctrl Pts',(5.58253582065927,0.497356886162411,4.33976214299073));
#38013=CARTESIAN_POINT('Ctrl Pts',(5.57458318131546,0.538985436353474,4.25002092526659));
#38014=CARTESIAN_POINT('Ctrl Pts',(5.56663054197165,0.580613986544537,4.16027970754245));
#38015=CARTESIAN_POINT('Ctrl Pts',(5.55867790262784,0.599343180535155,4.05991609106967));
#38016=CARTESIAN_POINT('Ctrl Pts',(5.55072526328404,0.592883119270616,3.96120089488413));
#38017=CARTESIAN_POINT('Ctrl Pts',(5.54277262394023,0.586423058006077,3.86248569869858));
#38018=CARTESIAN_POINT('Ctrl Pts',(5.53481998459642,0.554773741486382,3.76541892280029));
#38019=CARTESIAN_POINT('Ctrl Pts',(5.52686734525262,0.501804729712613,3.68186830256729));
#38020=CARTESIAN_POINT('Ctrl Pts',(5.51891470590881,0.448835717938844,3.5983176823343));
#38021=CARTESIAN_POINT('Ctrl Pts',(5.51096206656501,0.374547010911001,3.52828321776661));
#38022=CARTESIAN_POINT('Ctrl Pts',(5.5030094272212,0.288021414854312,3.48032757600706));
#38023=CARTESIAN_POINT('Ctrl Pts',(5.4950567878774,0.201495818797622,3.4323719342475));
#38024=CARTESIAN_POINT('Ctrl Pts',(5.48710414853359,0.102733333712086,3.40649511529609));
#38025=CARTESIAN_POINT('Ctrl Pts',(5.47915150918978,0.00380901851787326,
3.40586091270526));
#38026=CARTESIAN_POINT('Ctrl Pts',(5.47119886984597,-0.0951152966763399,
3.40522671011442));
#38027=CARTESIAN_POINT('Ctrl Pts',(5.46324623050217,-0.194201441979227,
3.42983512388417));
#38028=CARTESIAN_POINT('Ctrl Pts',(5.45529359115836,-0.281334786601535,
3.47667744027106));
#38029=CARTESIAN_POINT('Ctrl Pts',(5.44734095181456,-0.368468131223842,
3.52351975665794));
#38030=CARTESIAN_POINT('Ctrl Pts',(5.43938831247075,-0.443648675165568,
3.59259597566196));
#38031=CARTESIAN_POINT('Ctrl Pts',(5.43143567312694,-0.497684572991269,
3.67546058871077));
#38032=CARTESIAN_POINT('Ctrl Pts',(5.42348303378314,-0.551720470816969,
3.75832520175959));
#38033=CARTESIAN_POINT('Ctrl Pts',(5.41553039443933,-0.584611722526643,
3.85497820885321));
#38034=CARTESIAN_POINT('Ctrl Pts',(5.40757775509553,-0.592336924628993,
3.95360246348684));
#38035=CARTESIAN_POINT('Ctrl Pts',(5.39962511575172,-0.600062126731343,
4.05222671812048));
#38036=CARTESIAN_POINT('Ctrl Pts',(5.39167247640791,-0.582621279226368,
4.15282222029412));
#38037=CARTESIAN_POINT('Ctrl Pts',(5.3837198370641,-0.542146763261091,4.24308979978386));
#38038=CARTESIAN_POINT('Ctrl Pts',(5.3757671977203,-0.501672247295815,4.3333573792736));
#38039=CARTESIAN_POINT('Ctrl Pts',(5.36781455837649,-0.438164062870237,
4.41329703607943));
#38040=CARTESIAN_POINT('Ctrl Pts',(5.35986191903269,-0.359386950494509,
4.47313505840055));
#38041=CARTESIAN_POINT('Ctrl Pts',(5.35190927968888,-0.28060983811878,4.53297308072167));
#38042=CARTESIAN_POINT('Ctrl Pts',(5.34395664034507,-0.1865637977929,4.57270946855809));
#38043=CARTESIAN_POINT('Ctrl Pts',(5.33600400100126,-0.0887472388280498,
4.58748590729807));
#38044=CARTESIAN_POINT('Ctrl Pts',(5.33361780442003,-0.0593972924141157,
4.59191959101989));
#38045=CARTESIAN_POINT('Ctrl Pts',(5.3312316078388,-0.0297078841644672,
4.59410611700271));
#38046=CARTESIAN_POINT('Ctrl Pts',(5.32884541125756,-1.45357002139801E-5,
4.59407911932661));
#38047=CARTESIAN_POINT('Ctrl Pts',(5.22115458874249,1.46139895546772E-5,
4.59411444380891));
#38048=CARTESIAN_POINT('Ctrl Pts',(5.22764030503958,-0.0806785298274998,
4.59403186011492));
#38049=CARTESIAN_POINT('Ctrl Pts',(5.23412602133668,-0.161404528346198,
4.57747154641029));
#38050=CARTESIAN_POINT('Ctrl Pts',(5.24061173763377,-0.235476461490165,
4.54549665421293));
#38051=CARTESIAN_POINT('Ctrl Pts',(5.24856437697758,-0.32630179870949,4.50628976108741));
#38052=CARTESIAN_POINT('Ctrl Pts',(5.25651701632139,-0.407122673831612,
4.44390687590439));
#38053=CARTESIAN_POINT('Ctrl Pts',(5.26446965566519,-0.468057634114636,
4.36597515601533));
#38054=CARTESIAN_POINT('Ctrl Pts',(5.272422295009,-0.52899259439766,4.28804343612627));
#38055=CARTESIAN_POINT('Ctrl Pts',(5.28037493435281,-0.570041639841584,
4.19456288153117));
#38056=CARTESIAN_POINT('Ctrl Pts',(5.28832757369661,-0.586185965564114,
4.09696276320888));
#38057=CARTESIAN_POINT('Ctrl Pts',(5.29628021304042,-0.602330291286644,
3.99936264488659));
#38058=CARTESIAN_POINT('Ctrl Pts',(5.30423285238423,-0.59356989728778,3.89764296283709));
#38059=CARTESIAN_POINT('Ctrl Pts',(5.31218549172803,-0.560975861048054,
3.80424033358521));
#38060=CARTESIAN_POINT('Ctrl Pts',(5.32013813107184,-0.528381824808328,
3.71083770433334));
#38061=CARTESIAN_POINT('Ctrl Pts',(5.32809077041564,-0.471954146327742,
3.62575212787907));
#38062=CARTESIAN_POINT('Ctrl Pts',(5.33604340975945,-0.398591877830097,
3.55938647478623));
#38063=CARTESIAN_POINT('Ctrl Pts',(5.34399604910326,-0.325229609332449,
3.49302082169338));
#38064=CARTESIAN_POINT('Ctrl Pts',(5.35194868844707,-0.234932750817741,
3.44537509196196));
#38065=CARTESIAN_POINT('Ctrl Pts',(5.35990132779087,-0.138741323057917,
3.42227462497344));
#38066=CARTESIAN_POINT('Ctrl Pts',(5.36785396713468,-0.042549895298095,
3.39917415798493));
#38067=CARTESIAN_POINT('Ctrl Pts',(5.37580660647848,0.059536101706843,3.40061895373932));
#38068=CARTESIAN_POINT('Ctrl Pts',(5.38375924582229,0.155035264439678,3.42643236627792));
#38069=CARTESIAN_POINT('Ctrl Pts',(5.39171188516609,0.250534427172515,3.45224577881651));
#38070=CARTESIAN_POINT('Ctrl Pts',(5.3996645245099,0.339446755633248,3.5024278081393));
#38071=CARTESIAN_POINT('Ctrl Pts',(5.40761716385371,0.41090150670596,3.57084301769608));
#38072=CARTESIAN_POINT('Ctrl Pts',(5.41556980319751,0.482356257778672,3.63925822725286));
#38073=CARTESIAN_POINT('Ctrl Pts',(5.42352244254132,0.536353431463363,3.72590661704362));
#38074=CARTESIAN_POINT('Ctrl Pts',(5.43147508188513,0.566291137850326,3.82019424128906));
#38075=CARTESIAN_POINT('Ctrl Pts',(5.43942772122893,0.596228844237288,3.91448186553449));
#38076=CARTESIAN_POINT('Ctrl Pts',(5.44738036057274,0.602107083326521,4.01640872423458));
#38077=CARTESIAN_POINT('Ctrl Pts',(5.45533299991655,0.583207160329387,4.11351287069736));
#38078=CARTESIAN_POINT('Ctrl Pts',(5.46328563926035,0.564307237332252,4.21061701716013));
#38079=CARTESIAN_POINT('Ctrl Pts',(5.47123827860416,0.520629152248751,4.30289845138559));
#38080=CARTESIAN_POINT('Ctrl Pts',(5.47919091794796,0.457513145863858,4.37907451119169));
#38081=CARTESIAN_POINT('Ctrl Pts',(5.48714355729177,0.394397139478966,4.45525057099779));
#38082=CARTESIAN_POINT('Ctrl Pts',(5.49509619663558,0.311843211792683,4.51532125638452));
#38083=CARTESIAN_POINT('Ctrl Pts',(5.50304883597938,0.219944704826683,4.5519421079172));
#38084=CARTESIAN_POINT('Ctrl Pts',(5.50908408690042,0.150203009669811,4.5797336395568));
#38085=CARTESIAN_POINT('Ctrl Pts',(5.51511933782146,0.0750795109720808,
4.59401975858331));
#38086=CARTESIAN_POINT('Ctrl Pts',(5.52115458874249,-1.55733839743342E-5,
4.59409663347568));
#38087=CARTESIAN_POINT('Origin',(4.,0.,4.));
#38088=CARTESIAN_POINT('',(5.92884541125757,-1.3134308860685E-5,4.59412454375027));
#38089=CARTESIAN_POINT('',(5.82115458874249,1.31105368646138E-5,4.59407040741879));
#38090=CARTESIAN_POINT('',(4.,-7.27562663373442E-17,4.5941));
#38091=CARTESIAN_POINT('Ctrl Pts',(5.92884541125757,-1.3134308860685E-5,
4.59412454375027));
#38092=CARTESIAN_POINT('Ctrl Pts',(5.92209495209015,0.0839697382976411,
4.5940436242297));
#38093=CARTESIAN_POINT('Ctrl Pts',(5.91534449292274,0.16798613900316,4.57606223573506));
#38094=CARTESIAN_POINT('Ctrl Pts',(5.90859403375532,0.244517407380453,4.54150437939301));
#38095=CARTESIAN_POINT('Ctrl Pts',(5.90064139441152,0.334678026211646,4.50079216098422));
#38096=CARTESIAN_POINT('Ctrl Pts',(5.89268875506771,0.41445008323119,4.43707358099086));
#38097=CARTESIAN_POINT('Ctrl Pts',(5.8847361157239,0.474080337065587,4.35813908232779));
#38098=CARTESIAN_POINT('Ctrl Pts',(5.8767834763801,0.533710590899983,4.27920458366471));
#38099=CARTESIAN_POINT('Ctrl Pts',(5.86883083703629,0.573199041549232,4.18505416633191));
#38100=CARTESIAN_POINT('Ctrl Pts',(5.86087819769249,0.587717699183782,4.08719901244189));
#38101=CARTESIAN_POINT('Ctrl Pts',(5.85292555834868,0.602236356818331,3.98934385855186));
#38102=CARTESIAN_POINT('Ctrl Pts',(5.84497291900487,0.591785221438181,3.88778396810461));
#38103=CARTESIAN_POINT('Ctrl Pts',(5.83702027966107,0.557642080814915,3.79493641494568));
#38104=CARTESIAN_POINT('Ctrl Pts',(5.82906764031726,0.523498940191649,3.70208886178675));
#38105=CARTESIAN_POINT('Ctrl Pts',(5.82111500097346,0.465663794325265,3.61795364591614));
#38106=CARTESIAN_POINT('Ctrl Pts',(5.81316236162965,0.391207780605707,3.55281744653948));
#38107=CARTESIAN_POINT('Ctrl Pts',(5.80520972228584,0.31675176688615,3.48768124716281));
#38108=CARTESIAN_POINT('Ctrl Pts',(5.79725708294203,0.225674885313418,3.44154406428009));
#38109=CARTESIAN_POINT('Ctrl Pts',(5.78930444359823,0.129112523455512,3.42004679519738));
#38110=CARTESIAN_POINT('Ctrl Pts',(5.78135180425442,0.0325501615976049,
3.39854952611466));
#38111=CARTESIAN_POINT('Ctrl Pts',(5.77339916491062,-0.0694976805454773,
3.40169217083197));
#38112=CARTESIAN_POINT('Ctrl Pts',(5.76544652556681,-0.164554263536051,
3.42909049911887));
#38113=CARTESIAN_POINT('Ctrl Pts',(5.75749388622301,-0.259610846526622,
3.45648882740576));
#38114=CARTESIAN_POINT('Ctrl Pts',(5.7495412468792,-0.347676170364685,3.50814283926225));
#38115=CARTESIAN_POINT('Ctrl Pts',(5.74158860753539,-0.417983050247216,
3.57773712775495));
#38116=CARTESIAN_POINT('Ctrl Pts',(5.73363596819158,-0.488289930129746,
3.64733141624764));
#38117=CARTESIAN_POINT('Ctrl Pts',(5.72568332884778,-0.540838366056745,
3.73486598137654));
#38118=CARTESIAN_POINT('Ctrl Pts',(5.71773068950397,-0.569203595796233,
3.82963853060694));
#38119=CARTESIAN_POINT('Ctrl Pts',(5.70977805016017,-0.597568825535722,
3.92441107983734));
#38120=CARTESIAN_POINT('Ctrl Pts',(5.70182541081636,-0.6017508490877,4.02642161316923));
#38121=CARTESIAN_POINT('Ctrl Pts',(5.69387277147255,-0.581238357244447,
4.12319795341528));
#38122=CARTESIAN_POINT('Ctrl Pts',(5.68592013212875,-0.560725865401195,
4.21997429366132));
#38123=CARTESIAN_POINT('Ctrl Pts',(5.67796749278494,-0.515518858162713,
4.31151644082153));
#38124=CARTESIAN_POINT('Ctrl Pts',(5.67001485344113,-0.451144507802385,
4.38663212069642));
#38125=CARTESIAN_POINT('Ctrl Pts',(5.66206221409732,-0.386770157442057,
4.46174780057131));
#38126=CARTESIAN_POINT('Ctrl Pts',(5.65410957475352,-0.303228463959881,
4.52043701316089));
#38127=CARTESIAN_POINT('Ctrl Pts',(5.64615693540972,-0.210733537235404,
4.55552420285805));
#38128=CARTESIAN_POINT('Ctrl Pts',(5.640386427359,-0.143618370026196,4.5809837895275));
#38129=CARTESIAN_POINT('Ctrl Pts',(5.63461591930828,-0.07178924788396,4.59401670649762));
#38130=CARTESIAN_POINT('Ctrl Pts',(5.62884541125756,1.52328526200479E-5,
4.59408648697874));
#38131=CARTESIAN_POINT('Ctrl Pts',(5.52115458874249,-1.55733839743342E-5,
4.59409663347568));
#38132=CARTESIAN_POINT('Ctrl Pts',(5.52307197716526,-0.0238731473664388,
4.59412105649149));
#38133=CARTESIAN_POINT('Ctrl Pts',(5.52498936558803,-0.0477278534282068,
4.59271130989713));
#38134=CARTESIAN_POINT('Ctrl Pts',(5.5269067540108,-0.0714062077139717,
4.58984482465595));
#38135=CARTESIAN_POINT('Ctrl Pts',(5.53485939335461,-0.169615527042917,
4.57795567218339));
#38136=CARTESIAN_POINT('Ctrl Pts',(5.54281203269841,-0.264791079455087,
4.54100634955965));
#38137=CARTESIAN_POINT('Ctrl Pts',(5.55076467204222,-0.345296357402727,
4.48351441471562));
#38138=CARTESIAN_POINT('Ctrl Pts',(5.55871731138603,-0.425801635350366,
4.4260224798716));
#38139=CARTESIAN_POINT('Ctrl Pts',(5.56666995072984,-0.491636638833473,
4.34798793280729));
#38140=CARTESIAN_POINT('Ctrl Pts',(5.57462259007364,-0.534752142022197,
4.2589515597096));
#38141=CARTESIAN_POINT('Ctrl Pts',(5.58257522941745,-0.577867645210921,
4.16991518661191));
#38142=CARTESIAN_POINT('Ctrl Pts',(5.59052786876125,-0.598263648105263,
4.06987698748084));
#38143=CARTESIAN_POINT('Ctrl Pts',(5.59848050810506,-0.59344646156208,3.97106799465478));
#38144=CARTESIAN_POINT('Ctrl Pts',(5.60643314744886,-0.588629275018896,
3.87225900182873));
#38145=CARTESIAN_POINT('Ctrl Pts',(5.61438578679267,-0.558598899038186,
3.77467921530768));
#38146=CARTESIAN_POINT('Ctrl Pts',(5.62233842613648,-0.50702695609161,3.69025909300064));
#38147=CARTESIAN_POINT('Ctrl Pts',(5.63029106548029,-0.455455013145033,
3.6058389706936));
#38148=CARTESIAN_POINT('Ctrl Pts',(5.63824370482409,-0.382341503232591,
3.53457851260056));
#38149=CARTESIAN_POINT('Ctrl Pts',(5.6461963441679,-0.296625548722353,3.48519028027742));
#38150=CARTESIAN_POINT('Ctrl Pts',(5.6541489835117,-0.210909594212113,3.43580204795428));
#38151=CARTESIAN_POINT('Ctrl Pts',(5.66210162285551,-0.112591195104077,
3.40828604140104));
#38152=CARTESIAN_POINT('Ctrl Pts',(5.67005426219932,-0.0136911147678568,
3.40600646716786));
#38153=CARTESIAN_POINT('Ctrl Pts',(5.67800690154312,0.0852089655683624,
3.40372689293467));
#38154=CARTESIAN_POINT('Ctrl Pts',(5.68595954088693,0.184690727132768,3.42668375102154));
#38155=CARTESIAN_POINT('Ctrl Pts',(5.69391218023074,0.272591169676606,3.47207025288287));
#38156=CARTESIAN_POINT('Ctrl Pts',(5.70186481957454,0.360491612220445,3.51745675474419));
#38157=CARTESIAN_POINT('Ctrl Pts',(5.70981745891835,0.436810735743714,3.58527290037998));
#38158=CARTESIAN_POINT('Ctrl Pts',(5.71777009826216,0.492217487918224,3.667227242308));
#38159=CARTESIAN_POINT('Ctrl Pts',(5.72572273760596,0.547624240092733,3.74918158423602));
#38160=CARTESIAN_POINT('Ctrl Pts',(5.73367537694977,0.582118620918482,3.84527412245626));
#38161=CARTESIAN_POINT('Ctrl Pts',(5.74162801629357,0.591483222595687,3.94375623549444));
#38162=CARTESIAN_POINT('Ctrl Pts',(5.74958065563738,0.600847824272892,4.04223834853263));
#38163=CARTESIAN_POINT('Ctrl Pts',(5.75753329498119,0.585082646801554,4.14311003638875));
#38164=CARTESIAN_POINT('Ctrl Pts',(5.76548593432499,0.546115197731279,4.23403836123177));
#38165=CARTESIAN_POINT('Ctrl Pts',(5.7734385736688,0.507147748661005,4.32496668607478));
#38166=CARTESIAN_POINT('Ctrl Pts',(5.78139121301261,0.444978027991796,4.4059516479047));
#38167=CARTESIAN_POINT('Ctrl Pts',(5.78934385235641,0.367207131024688,4.46709173242012));
#38168=CARTESIAN_POINT('Ctrl Pts',(5.79729649170022,0.28943623405758,4.52823181693554));
#38169=CARTESIAN_POINT('Ctrl Pts',(5.80524913104403,0.196064160792572,4.56952702413646));
#38170=CARTESIAN_POINT('Ctrl Pts',(5.81320177038783,0.0985069184831505,
4.58592845199323));
#38171=CARTESIAN_POINT('Ctrl Pts',(5.81585270983939,0.0659871057213339,
4.59139571767544));
#38172=CARTESIAN_POINT('Ctrl Pts',(5.81850364929094,0.0330022532417819,
4.59409688335147));
#38173=CARTESIAN_POINT('Ctrl Pts',(5.82115458874249,1.31105368646138E-5,
4.59407040741879));
#38174=CARTESIAN_POINT('Origin',(4.,0.,4.));
#38175=CARTESIAN_POINT('',(6.22884541125756,-1.27841859475647E-5,4.5940334609955));
#38176=CARTESIAN_POINT('',(6.12115458874249,-9.50793186244619E-6,4.59413936148612));
#38177=CARTESIAN_POINT('',(4.,-7.27562663373442E-17,4.5941));
#38178=CARTESIAN_POINT('Ctrl Pts',(6.22884541125756,-1.27841859475647E-5,
4.5940334609955));
#38179=CARTESIAN_POINT('Ctrl Pts',(6.22547926355963,0.0418951881409122,
4.59406590912705));
#38180=CARTESIAN_POINT('Ctrl Pts',(6.2221131158617,0.0838018877146867,4.58971510200585));
#38181=CARTESIAN_POINT('Ctrl Pts',(6.21874696816377,0.124749109322564,4.58093223526196));
#38182=CARTESIAN_POINT('Ctrl Pts',(6.21079432881996,0.22148832423537,4.56018241146135));
#38183=CARTESIAN_POINT('Ctrl Pts',(6.20284168947616,0.31287214740051,4.51469474440412));
#38184=CARTESIAN_POINT('Ctrl Pts',(6.19488905013236,0.387808805213989,4.4501133836823));
#38185=CARTESIAN_POINT('Ctrl Pts',(6.18693641078855,0.462745463027469,4.38553202296047));
#38186=CARTESIAN_POINT('Ctrl Pts',(6.17898377144474,0.521234955489287,4.30185696857405));
#38187=CARTESIAN_POINT('Ctrl Pts',(6.17103113210093,0.556083161424236,4.20927485003939));
#38188=CARTESIAN_POINT('Ctrl Pts',(6.16307849275713,0.590931367359184,4.11669273150472));
#38189=CARTESIAN_POINT('Ctrl Pts',(6.15512585341332,0.602138286767263,4.0152035488218));
#38190=CARTESIAN_POINT('Ctrl Pts',(6.14717321406952,0.588356486924291,3.9172389266648));
#38191=CARTESIAN_POINT('Ctrl Pts',(6.13922057472571,0.574574687081318,3.81927430450779));
#38192=CARTESIAN_POINT('Ctrl Pts',(6.1312679353819,0.535804167987293,3.7248342428767));
#38193=CARTESIAN_POINT('Ctrl Pts',(6.12331529603809,0.476773096629474,3.64545304401991));
#38194=CARTESIAN_POINT('Ctrl Pts',(6.11536265669429,0.417742025271657,3.56607184516312));
#38195=CARTESIAN_POINT('Ctrl Pts',(6.10741001735048,0.338450401650047,3.50174950908064));
#38196=CARTESIAN_POINT('Ctrl Pts',(6.09945737800668,0.248599092144812,3.46035682177302));
#38197=CARTESIAN_POINT('Ctrl Pts',(6.09150473866287,0.158747782639575,3.41896413446539));
#38198=CARTESIAN_POINT('Ctrl Pts',(6.08355209931906,0.0583367872507115,
3.40050109593262));
#38199=CARTESIAN_POINT('Ctrl Pts',(6.07559945997526,-0.0403606640336046,
3.40722161935946));
#38200=CARTESIAN_POINT('Ctrl Pts',(6.06764682063145,-0.139058115317921,
3.4139421427863));
#38201=CARTESIAN_POINT('Ctrl Pts',(6.05969418128764,-0.23604202249769,3.44584622817275));
#38202=CARTESIAN_POINT('Ctrl Pts',(6.05174154194384,-0.319452991027635,
3.49903499090221));
#38203=CARTESIAN_POINT('Ctrl Pts',(6.04378890260003,-0.40286395955758,3.55222375363166));
#38204=CARTESIAN_POINT('Ctrl Pts',(6.03583626325623,-0.472701989437702,
3.62669719370411));
#38205=CARTESIAN_POINT('Ctrl Pts',(6.02788362391242,-0.520429378860104,
3.71334895258148));
#38206=CARTESIAN_POINT('Ctrl Pts',(6.01993098456861,-0.568156768282506,
3.80000071145885));
#38207=CARTESIAN_POINT('Ctrl Pts',(6.0119783452248,-0.593773517247188,3.89883078914114));
#38208=CARTESIAN_POINT('Ctrl Pts',(6.004025705881,-0.594147126960238,3.99775637428654));
#38209=CARTESIAN_POINT('Ctrl Pts',(5.99607306653719,-0.594520736673288,
4.09668195943193));
#38210=CARTESIAN_POINT('Ctrl Pts',(5.98812042719339,-0.569651207134705,
4.19570305204043));
#38211=CARTESIAN_POINT('Ctrl Pts',(5.98016778784958,-0.52257944308796,4.28271270390554));
#38212=CARTESIAN_POINT('Ctrl Pts',(5.97221514850578,-0.475507679041215,
4.36972235577065));
#38213=CARTESIAN_POINT('Ctrl Pts',(5.96426250916196,-0.406233680486307,
4.44472056689237));
#38214=CARTESIAN_POINT('Ctrl Pts',(5.95630986981816,-0.323226996343023,
4.49853792802592));
#38215=CARTESIAN_POINT('Ctrl Pts',(5.94835723047435,-0.240220312199739,
4.55235528915947));
#38216=CARTESIAN_POINT('Ctrl Pts',(5.94040459113055,-0.143480942468078,
4.58499180030486));
#38217=CARTESIAN_POINT('Ctrl Pts',(5.93245195178675,-0.0448366672808267,
4.59245712746544));
#38218=CARTESIAN_POINT('Ctrl Pts',(5.93124977161035,-0.0299248641651563,
4.59358564190382));
#38219=CARTESIAN_POINT('Ctrl Pts',(5.93004759143396,-0.0149695309183627,
4.59413895459864));
#38220=CARTESIAN_POINT('Ctrl Pts',(5.92884541125757,-1.3134308860685E-5,
4.59412454375027));
#38221=CARTESIAN_POINT('Ctrl Pts',(5.82115458874249,1.31105368646138E-5,
4.59407040741879));
#38222=CARTESIAN_POINT('Ctrl Pts',(5.82645628863475,-0.0659629472043463,
4.59401745734129));
#38223=CARTESIAN_POINT('Ctrl Pts',(5.831757988527,-0.131956164688202,4.58305467757793));
#38224=CARTESIAN_POINT('Ctrl Pts',(5.83705968841925,-0.194280919321303,
4.56148970414564));
#38225=CARTESIAN_POINT('Ctrl Pts',(5.84501232776306,-0.287769103462499,
4.52914187992864));
#38226=CARTESIAN_POINT('Ctrl Pts',(5.85296496710686,-0.373003060391055,
4.47293858298203));
#38227=CARTESIAN_POINT('Ctrl Pts',(5.86091760645067,-0.439561779454174,
4.39975142997742));
#38228=CARTESIAN_POINT('Ctrl Pts',(5.86887024579447,-0.506120498517293,
4.32656427697281));
#38229=CARTESIAN_POINT('Ctrl Pts',(5.87682288513828,-0.554003979714975,
4.2363932679102));
#38230=CARTESIAN_POINT('Ctrl Pts',(5.88477552448209,-0.577357812582609,
4.14026304025204));
#38231=CARTESIAN_POINT('Ctrl Pts',(5.8927281638259,-0.600711645450243,4.04413281259387));
#38232=CARTESIAN_POINT('Ctrl Pts',(5.9006808031697,-0.59953582998783,3.94204336634015));
#38233=CARTESIAN_POINT('Ctrl Pts',(5.90863344251351,-0.573974130801472,
3.84647652011691));
#38234=CARTESIAN_POINT('Ctrl Pts',(5.91658608185731,-0.548412431615114,
3.75090967389367));
#38235=CARTESIAN_POINT('Ctrl Pts',(5.92453872120112,-0.498464848704808,
3.66186542770092));
#38236=CARTESIAN_POINT('Ctrl Pts',(5.93249136054493,-0.430238144626613,
3.59023066587279));
#38237=CARTESIAN_POINT('Ctrl Pts',(5.94044399988873,-0.362011440548417,
3.51859590404466));
#38238=CARTESIAN_POINT('Ctrl Pts',(5.94839663923254,-0.275505615302329,
3.46437062658116));
#38239=CARTESIAN_POINT('Ctrl Pts',(5.95634927857635,-0.181297202577209,
3.43418458862315));
#38240=CARTESIAN_POINT('Ctrl Pts',(5.96430191792015,-0.087088789852092,
3.40399855066514));
#38241=CARTESIAN_POINT('Ctrl Pts',(5.97225455726396,0.0148222103520573,
3.39785175221263));
#38242=CARTESIAN_POINT('Ctrl Pts',(5.98020719660777,0.111975824940657,3.41649576758492));
#38243=CARTESIAN_POINT('Ctrl Pts',(5.98815983595157,0.209129439529257,3.43513978295721));
#38244=CARTESIAN_POINT('Ctrl Pts',(5.99611247529537,0.301525668502307,3.47857461215431));
#38245=CARTESIAN_POINT('Ctrl Pts',(6.00406511463918,0.377867748972965,3.54148967172874));
#38246=CARTESIAN_POINT('Ctrl Pts',(6.01201775398299,0.454209829443624,3.60440473130317));
#38247=CARTESIAN_POINT('Ctrl Pts',(6.0199703933268,0.514497761411887,3.68680002125492));
#38248=CARTESIAN_POINT('Ctrl Pts',(6.02792303267061,0.551360647735685,3.77860175380959));
#38249=CARTESIAN_POINT('Ctrl Pts',(6.03587567201441,0.588223534059482,3.87040348636426));
#38250=CARTESIAN_POINT('Ctrl Pts',(6.04382831135821,0.601661374738811,3.97161166152184));
#38251=CARTESIAN_POINT('Ctrl Pts',(6.05178095070202,0.590030977261751,4.06985190192822));
#38252=CARTESIAN_POINT('Ctrl Pts',(6.05973359004583,0.578400579784692,4.16809214233459));
#38253=CARTESIAN_POINT('Ctrl Pts',(6.06768622938964,0.541701944151245,4.26336444798975));
#38254=CARTESIAN_POINT('Ctrl Pts',(6.07563886873345,0.484422419230229,4.3440210474869));
#38255=CARTESIAN_POINT('Ctrl Pts',(6.08359150807725,0.427142894309213,4.42467764698404));
#38256=CARTESIAN_POINT('Ctrl Pts',(6.09154414742105,0.349282480100627,4.49071854032316));
#38257=CARTESIAN_POINT('Ctrl Pts',(6.09949678676486,0.26035984028865,4.53406826097581));
#38258=CARTESIAN_POINT('Ctrl Pts',(6.10671605409073,0.179637418414302,4.5734203814938));
#38259=CARTESIAN_POINT('Ctrl Pts',(6.11393532141662,0.0897989573399868,
4.59407340590587));
#38260=CARTESIAN_POINT('Ctrl Pts',(6.12115458874249,-9.50793186244619E-6,
4.59413936148612));
#38261=CARTESIAN_POINT('Origin',(4.,0.,4.));
#38262=CARTESIAN_POINT('',(6.52884541125757,2.61457539729726E-5,4.59508370962656));
#38263=CARTESIAN_POINT('',(6.42115458874249,-0.000630941829811112,4.59394485456974));
#38264=CARTESIAN_POINT('',(4.,-7.27562663373442E-17,4.5941));
#38265=CARTESIAN_POINT('Ctrl Pts',(6.52884541125757,2.61457539729726E-5,
4.59508370962656));
#38266=CARTESIAN_POINT('Ctrl Pts',(6.5129582963415,0.196771080344787,4.59506033873941));
#38267=CARTESIAN_POINT('Ctrl Pts',(6.49707118142544,0.393450480974957,4.48779253427891));
#38268=CARTESIAN_POINT('Ctrl Pts',(6.48118406650938,0.500111739713094,4.32240987211318));
#38269=CARTESIAN_POINT('Ctrl Pts',(6.46527878782176,0.606894944490356,4.15683812760557));
#38270=CARTESIAN_POINT('Ctrl Pts',(6.44937350913416,0.623454053851315,3.93301856375293));
#38271=CARTESIAN_POINT('Ctrl Pts',(6.43346823044654,0.541809843535619,3.75368369989414));
#38272=CARTESIAN_POINT('Ctrl Pts',(6.41756295175893,0.460165633219924,3.57434883603535));
#38273=CARTESIAN_POINT('Ctrl Pts',(6.40165767307132,0.280318103227576,3.43949867217041));
#38274=CARTESIAN_POINT('Ctrl Pts',(6.3857523943837,0.085604811340831,3.41110814665827));
#38275=CARTESIAN_POINT('Ctrl Pts',(6.36984711569609,-0.109108480545914,
3.38271762114613));
#38276=CARTESIAN_POINT('Ctrl Pts',(6.35394183700848,-0.318687534327053,
3.46078673398678));
#38277=CARTESIAN_POINT('Ctrl Pts',(6.33803655832087,-0.448733343985475,
3.60951691634857));
#38278=CARTESIAN_POINT('Ctrl Pts',(6.33008391897706,-0.513756248814686,
3.68388200752946));
#38279=CARTESIAN_POINT('Ctrl Pts',(6.32213127963325,-0.558895842613217,
3.77591236609064));
#38280=CARTESIAN_POINT('Ctrl Pts',(6.31417864028945,-0.579995970841135,
3.87270290659392));
#38281=CARTESIAN_POINT('Ctrl Pts',(6.30622600094564,-0.601096099069052,
3.9694934470972));
#38282=CARTESIAN_POINT('Ctrl Pts',(6.29827336160184,-0.598156761726356,
4.07104416954258));
#38283=CARTESIAN_POINT('Ctrl Pts',(6.29032072225803,-0.570614590620327,
4.16591643177432));
#38284=CARTESIAN_POINT('Ctrl Pts',(6.28236808291422,-0.543072419514299,
4.26078869400605));
#38285=CARTESIAN_POINT('Ctrl Pts',(6.27441544357042,-0.490927414644939,
4.34898249602413));
#38286=CARTESIAN_POINT('Ctrl Pts',(6.26646280422661,-0.421087730399527,
4.41916768405122));
#38287=CARTESIAN_POINT('Ctrl Pts',(6.2585101648828,-0.351248046154114,4.48935287207832));
#38288=CARTESIAN_POINT('Ctrl Pts',(6.250557525539,-0.263713682532649,4.54152944611444));
#38289=CARTESIAN_POINT('Ctrl Pts',(6.24260488619519,-0.168899197391682,
4.5696117428605));
#38290=CARTESIAN_POINT('Ctrl Pts',(6.23801839454932,-0.114217245248871,
4.58580752565092));
#38291=CARTESIAN_POINT('Ctrl Pts',(6.23343190290344,-0.0571138332845632,
4.59398924930378));
#38292=CARTESIAN_POINT('Ctrl Pts',(6.22884541125756,-1.27841859475647E-5,
4.5940334609955));
#38293=CARTESIAN_POINT('Ctrl Pts',(6.12115458874249,-9.50793186244619E-6,
4.59413936148612));
#38294=CARTESIAN_POINT('Ctrl Pts',(6.12188796076042,-0.00913273504488762,
4.59414606160884));
#38295=CARTESIAN_POINT('Ctrl Pts',(6.12262133277835,-0.0182556526135436,
4.59394031163173));
#38296=CARTESIAN_POINT('Ctrl Pts',(6.12335470479628,-0.0273686726716501,
4.59352013235631));
#38297=CARTESIAN_POINT('Ctrl Pts',(6.13130734414009,-0.126189680404606,
4.58896373511797));
#38298=CARTESIAN_POINT('Ctrl Pts',(6.13925998348389,-0.223846830455152,
4.55919239267511));
#38299=CARTESIAN_POINT('Ctrl Pts',(6.14721262282769,-0.308403173896691,
4.50784224986958));
#38300=CARTESIAN_POINT('Ctrl Pts',(6.1551652621715,-0.392959517338232,4.45649210706404));
#38301=CARTESIAN_POINT('Ctrl Pts',(6.16311790151532,-0.464415054170765,
4.38356316389581));
#38302=CARTESIAN_POINT('Ctrl Pts',(6.17107054085912,-0.514027768136376,
4.29797916579711));
#38303=CARTESIAN_POINT('Ctrl Pts',(6.17902318020293,-0.563640482101988,
4.2123951676984));
#38304=CARTESIAN_POINT('Ctrl Pts',(6.18697581954673,-0.591410373200678,
4.11415611466921));
#38305=CARTESIAN_POINT('Ctrl Pts',(6.19492845889053,-0.593952774873424,
4.0152594949342));
#38306=CARTESIAN_POINT('Ctrl Pts',(6.20288109823434,-0.59649517654617,3.9163628751992));
#38307=CARTESIAN_POINT('Ctrl Pts',(6.21083373757815,-0.573810088792972,
3.81680868875837));
#38308=CARTESIAN_POINT('Ctrl Pts',(6.21878637692196,-0.528651094032059,
3.72879442104321));
#38309=CARTESIAN_POINT('Ctrl Pts',(6.22673901626577,-0.483492099271145,
3.64078015332805));
#38310=CARTESIAN_POINT('Ctrl Pts',(6.23469165560957,-0.415859197502516,
3.56430580433857));
#38311=CARTESIAN_POINT('Ctrl Pts',(6.24264429495337,-0.334059153459168,
3.50867301156809));
#38312=CARTESIAN_POINT('Ctrl Pts',(6.25059693429718,-0.252259109415819,
3.45304021879761));
#38313=CARTESIAN_POINT('Ctrl Pts',(6.25854957364099,-0.156291923097747,
3.41824898224614));
#38314=CARTESIAN_POINT('Ctrl Pts',(6.2665022129848,-0.057819682214149,3.40864436538418));
#38315=CARTESIAN_POINT('Ctrl Pts',(6.2744548523286,0.0406525586694487,3.39903974852221));
#38316=CARTESIAN_POINT('Ctrl Pts',(6.28240749167241,0.141629854118573,3.41462175134974));
#38317=CARTESIAN_POINT('Ctrl Pts',(6.29036013101621,0.232632044389671,3.453312878872));
#38318=CARTESIAN_POINT('Ctrl Pts',(6.29831277036002,0.323634234660771,3.49200400639426));
#38319=CARTESIAN_POINT('Ctrl Pts',(6.30626540970382,0.404661319753841,3.55380425861124));
#38320=CARTESIAN_POINT('Ctrl Pts',(6.31421804904763,0.466059055789261,3.63148218419904));
#38321=CARTESIAN_POINT('Ctrl Pts',(6.32217068839144,0.527456791824679,3.70916010978684));
#38322=CARTESIAN_POINT('Ctrl Pts',(6.33012332773525,0.569225178802449,3.80271570874544));
#38323=CARTESIAN_POINT('Ctrl Pts',(6.33807596707905,0.585790493249255,3.90010619949006));
#38324=CARTESIAN_POINT('Ctrl Pts',(6.34602860642286,0.602355807696062,3.99749669023468));
#38325=CARTESIAN_POINT('Ctrl Pts',(6.35398124576666,0.593718049611903,4.09872207276531));
#38326=CARTESIAN_POINT('Ctrl Pts',(6.36193388511047,0.56173881546021,4.19248215342453));
#38327=CARTESIAN_POINT('Ctrl Pts',(6.36988652445427,0.529759581308516,4.28624223408375));
#38328=CARTESIAN_POINT('Ctrl Pts',(6.37783916379808,0.474438871089287,4.37253701287156));
#38329=CARTESIAN_POINT('Ctrl Pts',(6.38579180314189,0.401374624788453,4.4390182948332));
#38330=CARTESIAN_POINT('Ctrl Pts',(6.39757939834209,0.293077024234899,4.53755846574697));
#38331=CARTESIAN_POINT('Ctrl Pts',(6.40936699354229,0.145797072855576,4.59256860517148));
#38332=CARTESIAN_POINT('Ctrl Pts',(6.42115458874249,-0.000630941829811112,
4.59394485456974));
#38333=CARTESIAN_POINT('Origin',(4.,0.,4.));
#38334=CARTESIAN_POINT('',(6.82884541125756,0.000528213615369061,4.5937871332276));
#38335=CARTESIAN_POINT('',(6.72115458874249,0.000109070110168276,4.59505938903171));
#38336=CARTESIAN_POINT('',(4.,-7.27562663373442E-17,4.5941));
#38337=CARTESIAN_POINT('Ctrl Pts',(6.82884541125756,0.000528213615369061,
4.5937871332276));
#38338=CARTESIAN_POINT('Ctrl Pts',(6.82429524715479,0.0572034606387535,
4.59426930340541));
#38339=CARTESIAN_POINT('Ctrl Pts',(6.81974508305202,0.113754426020979,4.58681959872387));
#38340=CARTESIAN_POINT('Ctrl Pts',(6.81519491894924,0.167823213394864,4.57092612439125));
#38341=CARTESIAN_POINT('Ctrl Pts',(6.79928964026163,0.356822799356826,4.51536985589957));
#38342=CARTESIAN_POINT('Ctrl Pts',(6.78338436157403,0.515493156338912,4.35664088088147));
#38343=CARTESIAN_POINT('Ctrl Pts',(6.76747908288642,0.570983871223461,4.16762126762428));
#38344=CARTESIAN_POINT('Ctrl Pts',(6.7515738041988,0.626474586108011,3.97860165436708));
#38345=CARTESIAN_POINT('Ctrl Pts',(6.73566852551118,0.578785658895023,3.75929140287077));
#38346=CARTESIAN_POINT('Ctrl Pts',(6.71976324682357,0.449805704301045,3.61038767491097));
#38347=CARTESIAN_POINT('Ctrl Pts',(6.70385796813595,0.320825749707067,3.46148394695116));
#38348=CARTESIAN_POINT('Ctrl Pts',(6.68795268944834,0.110554767732096,3.38298674252784));
#38349=CARTESIAN_POINT('Ctrl Pts',(6.67204741076073,-0.0844443642884844,
3.4109402193496));
#38350=CARTESIAN_POINT('Ctrl Pts',(6.65614213207312,-0.279443496309066,
3.43889369617135));
#38351=CARTESIAN_POINT('Ctrl Pts',(6.64023685338551,-0.459170778375258,
3.57329785423817));
#38352=CARTESIAN_POINT('Ctrl Pts',(6.6243315746979,-0.541132009270427,3.75243704050979));
#38353=CARTESIAN_POINT('Ctrl Pts',(6.60842629601029,-0.623093240165596,
3.9315762267814));
#38354=CARTESIAN_POINT('Ctrl Pts',(6.59252101732267,-0.60728841988974,4.15545044125781));
#38355=CARTESIAN_POINT('Ctrl Pts',(6.57661573863506,-0.500919754058047,
4.32127168369798));
#38356=CARTESIAN_POINT('Ctrl Pts',(6.56069229617589,-0.394429615589227,
4.48728229340579));
#38357=CARTESIAN_POINT('Ctrl Pts',(6.54476885371673,-0.197168666623305,
4.59510713395368));
#38358=CARTESIAN_POINT('Ctrl Pts',(6.52884541125757,2.61457539729726E-5,
4.59508370962656));
#38359=CARTESIAN_POINT('Ctrl Pts',(6.42115458874249,-0.000630941829811112,
4.59394485456974));
#38360=CARTESIAN_POINT('Ctrl Pts',(6.4252722722299,-0.0517816819022344,
4.59442561076518));
#38361=CARTESIAN_POINT('Ctrl Pts',(6.42938995571731,-0.102828462800867,
4.58836159088269));
#38362=CARTESIAN_POINT('Ctrl Pts',(6.43350763920472,-0.152073274319339,
4.5753220992581));
#38363=CARTESIAN_POINT('Ctrl Pts',(6.44941291789233,-0.342290043897387,
4.52495476314113));
#38364=CARTESIAN_POINT('Ctrl Pts',(6.46531819657995,-0.5056209461254,4.37051151428857));
#38365=CARTESIAN_POINT('Ctrl Pts',(6.48122347526756,-0.56632363157735,4.18304963962536));
#38366=CARTESIAN_POINT('Ctrl Pts',(6.49712875395518,-0.627026317029301,
3.99558776496215));
#38367=CARTESIAN_POINT('Ctrl Pts',(6.51303403264279,-0.58510078570519,3.77510726448829));
#38368=CARTESIAN_POINT('Ctrl Pts',(6.5289393113304,-0.460166914262479,3.62276494217392));
#38369=CARTESIAN_POINT('Ctrl Pts',(6.54484459001801,-0.335233042819767,
3.47042261985956));
#38370=CARTESIAN_POINT('Ctrl Pts',(6.56074986870563,-0.127290831258456,
3.38621847570468));
#38371=CARTESIAN_POINT('Ctrl Pts',(6.57665514739324,0.068373869747762,3.4088573345089));
#38372=CARTESIAN_POINT('Ctrl Pts',(6.59256042608085,0.26403857075398,3.43149619331313));
#38373=CARTESIAN_POINT('Ctrl Pts',(6.60846570476847,0.447425761205104,3.56097805507645));
#38374=CARTESIAN_POINT('Ctrl Pts',(6.62437098345608,0.534230294511761,3.73782813427527));
#38375=CARTESIAN_POINT('Ctrl Pts',(6.64027626214369,0.621034827818418,3.91467821347409));
#38376=CARTESIAN_POINT('Ctrl Pts',(6.65618154083131,0.611256703980608,4.1388965101084));
#38377=CARTESIAN_POINT('Ctrl Pts',(6.67208681951892,0.509439333868548,4.30754322537844));
#38378=CARTESIAN_POINT('Ctrl Pts',(6.68799209820653,0.40762196375649,4.47618994064847));
#38379=CARTESIAN_POINT('Ctrl Pts',(6.70389737689414,0.213765347370184,4.58926507455422));
#38380=CARTESIAN_POINT('Ctrl Pts',(6.71980265558175,0.016851802420978,4.59484308232941));
#38381=CARTESIAN_POINT('Ctrl Pts',(6.72025329996867,0.0112726493937942,
4.59500112406784));
#38382=CARTESIAN_POINT('Ctrl Pts',(6.72070394435558,0.00569104238866241,
4.59507287148453));
#38383=CARTESIAN_POINT('Ctrl Pts',(6.72115458874249,0.000109070110168276,
4.59505938903171));
#38384=CARTESIAN_POINT('Origin',(4.,0.,4.));
#38385=CARTESIAN_POINT('',(7.12884541125757,-0.000233413975479213,4.59320261234329));
#38386=CARTESIAN_POINT('',(7.02115458874249,0.000491936389841303,4.5936290357477));
#38387=CARTESIAN_POINT('',(4.,-7.27562663373442E-17,4.5941));
#38388=CARTESIAN_POINT('Ctrl Pts',(7.12884541125757,-0.000233413975479213,
4.59320261234329));
#38389=CARTESIAN_POINT('Ctrl Pts',(7.11972691928047,0.113624805666132,4.59280158872514));
#38390=CARTESIAN_POINT('Ctrl Pts',(7.11060842730338,0.227688545642871,4.56127879346404));
#38391=CARTESIAN_POINT('Ctrl Pts',(7.10148993532628,0.322592019514134,4.50005536307953));
#38392=CARTESIAN_POINT('Ctrl Pts',(7.08558465663867,0.488131036726243,4.39326405099382));
#38393=CARTESIAN_POINT('Ctrl Pts',(7.06967937795105,0.595374147168556,4.19610732087965));
#38394=CARTESIAN_POINT('Ctrl Pts',(7.05377409926343,0.595079946532544,3.99911121186167));
#38395=CARTESIAN_POINT('Ctrl Pts',(7.03786882057582,0.594785745896532,3.80211510284369));
#38396=CARTESIAN_POINT('Ctrl Pts',(7.02196354188821,0.486954234182196,3.60527961492189));
#38397=CARTESIAN_POINT('Ctrl Pts',(7.0060582632006,0.321096900356496,3.49898325846904));
#38398=CARTESIAN_POINT('Ctrl Pts',(6.99015298451299,0.155239566530797,3.3926869020162));
#38399=CARTESIAN_POINT('Ctrl Pts',(6.97424770582538,-0.0686435894062663,
3.37692967703231));
#38400=CARTESIAN_POINT('Ctrl Pts',(6.95834242713776,-0.247754555527299,
3.45894666907189));
#38401=CARTESIAN_POINT('Ctrl Pts',(6.94243714845015,-0.426865521648332,
3.54096366111146));
#38402=CARTESIAN_POINT('Ctrl Pts',(6.92653186976253,-0.561204297953336,
3.72075487017451));
#38403=CARTESIAN_POINT('Ctrl Pts',(6.91062659107492,-0.589088840804576,
3.91576771430201));
#38404=CARTESIAN_POINT('Ctrl Pts',(6.89472131238731,-0.616973383655816,
4.11078055842951));
#38405=CARTESIAN_POINT('Ctrl Pts',(6.8788160336997,-0.538403693053295,4.32101503762147));
#38406=CARTESIAN_POINT('Ctrl Pts',(6.86291075501209,-0.389454440281117,
4.44994049623482));
#38407=CARTESIAN_POINT('Ctrl Pts',(6.85155564042725,-0.283116420949728,
4.54198310574898));
#38408=CARTESIAN_POINT('Ctrl Pts',(6.8402005258424,-0.140907108175025,4.59258385846765));
#38409=CARTESIAN_POINT('Ctrl Pts',(6.82884541125756,0.000528213615369061,
4.5937871332276));
#38410=CARTESIAN_POINT('Ctrl Pts',(6.72115458874249,0.000109070110168276,
4.59505938903171));
#38411=CARTESIAN_POINT('Ctrl Pts',(6.73660922304319,-0.191322006690816,
4.59459701474307));
#38412=CARTESIAN_POINT('Ctrl Pts',(6.75206385734389,-0.38318268672033,4.49389457135631));
#38413=CARTESIAN_POINT('Ctrl Pts',(6.76751849164459,-0.49122657597837,4.33588597251985));
#38414=CARTESIAN_POINT('Ctrl Pts',(6.78342377033221,-0.60242093591639,4.17326997329048));
#38415=CARTESIAN_POINT('Ctrl Pts',(6.79932904901982,-0.624839182280325,
3.94995709318712));
#38416=CARTESIAN_POINT('Ctrl Pts',(6.81523432770743,-0.548195780923551,
3.76848141254984));
#38417=CARTESIAN_POINT('Ctrl Pts',(6.83113960639504,-0.471552379566775,
3.58700573191256));
#38418=CARTESIAN_POINT('Ctrl Pts',(6.84704488508266,-0.295847330489284,
3.44736725074137));
#38419=CARTESIAN_POINT('Ctrl Pts',(6.86295016377027,-0.101752734572189,
3.41368297698799));
#38420=CARTESIAN_POINT('Ctrl Pts',(6.87885544245788,0.0923418613449005,
3.37999870323461));
#38421=CARTESIAN_POINT('Ctrl Pts',(6.8947607211455,0.304826004101594,3.45226863689903));
#38422=CARTESIAN_POINT('Ctrl Pts',(6.91066599983311,0.438133727661537,3.59730899203965));
#38423=CARTESIAN_POINT('Ctrl Pts',(6.92657127852072,0.571441451221483,3.74234934718029));
#38424=CARTESIAN_POINT('Ctrl Pts',(6.94247655720833,0.625572755584675,3.96016012379713));
#38425=CARTESIAN_POINT('Ctrl Pts',(6.95838183589594,0.57567402069499,4.15073208753033));
#38426=CARTESIAN_POINT('Ctrl Pts',(6.97428711458356,0.525775285805305,4.34130405126353));
#38427=CARTESIAN_POINT('Ctrl Pts',(6.99019239327118,0.371846511662747,4.5046372021131));
#38428=CARTESIAN_POINT('Ctrl Pts',(7.00609767195879,0.184564651688987,4.56573572985967));
#38429=CARTESIAN_POINT('Ctrl Pts',(7.01111664422002,0.125467135782336,4.58501560681028));
#38430=CARTESIAN_POINT('Ctrl Pts',(7.01613561648126,0.0630485115161635,
4.59411554829291));
#38431=CARTESIAN_POINT('Ctrl Pts',(7.02115458874249,0.000491936389841303,
4.5936290357477));
#38432=CARTESIAN_POINT('Origin',(4.,0.,4.));
#38433=CARTESIAN_POINT('',(7.42884541125756,-0.000438237927964824,4.59464495791636));
#38434=CARTESIAN_POINT('',(7.32115458874249,-0.000317338366111653,4.59328419319629));
#38435=CARTESIAN_POINT('',(4.,-7.27562663373442E-17,4.5941));
#38436=CARTESIAN_POINT('Ctrl Pts',(7.42884541125756,-0.000438237927964824,
4.59464495791636));
#38437=CARTESIAN_POINT('Ctrl Pts',(7.41515859140615,0.169409178821721,4.5932420274804));
#38438=CARTESIAN_POINT('Ctrl Pts',(7.40147177155473,0.340360224580004,4.51673272682389));
#38439=CARTESIAN_POINT('Ctrl Pts',(7.38778495170331,0.450965110664874,4.38826722161738));
#38440=CARTESIAN_POINT('Ctrl Pts',(7.37187967301569,0.579497637321094,4.23897909740477));
#38441=CARTESIAN_POINT('Ctrl Pts',(7.35597439432808,0.626535888751401,4.01952688559808));
#38442=CARTESIAN_POINT('Ctrl Pts',(7.34006911564046,0.570481892017836,3.83067375781486));
#38443=CARTESIAN_POINT('Ctrl Pts',(7.32416383695285,0.51442789528427,3.64182063003164));
#38444=CARTESIAN_POINT('Ctrl Pts',(7.30825855826524,0.355281650386831,3.48356658627189));
#38445=CARTESIAN_POINT('Ctrl Pts',(7.29235327957763,0.166116376105148,3.42857518785077));
#38446=CARTESIAN_POINT('Ctrl Pts',(7.27644800089002,-0.023048898176535,
3.37358378942964));
#38447=CARTESIAN_POINT('Ctrl Pts',(7.2605427222024,-0.242233201842457,3.42185503634715));
#38448=CARTESIAN_POINT('Ctrl Pts',(7.24463744351479,-0.390796368104757,
3.5512248149675));
#38449=CARTESIAN_POINT('Ctrl Pts',(7.22873216482718,-0.539359534367058,
3.68059459358785));
#38450=CARTESIAN_POINT('Ctrl Pts',(7.21282688613957,-0.617301563225728,
3.89106290391106));
#38451=CARTESIAN_POINT('Ctrl Pts',(7.19692160745195,-0.588834786584626,
4.08599160058025));
#38452=CARTESIAN_POINT('Ctrl Pts',(7.18101632876434,-0.560368009943526,
4.28092029724944));
#38453=CARTESIAN_POINT('Ctrl Pts',(7.16511105007672,-0.425492427802657,
4.46030938026461));
#38454=CARTESIAN_POINT('Ctrl Pts',(7.14920577138911,-0.24613717474127,4.54179097474357));
#38455=CARTESIAN_POINT('Ctrl Pts',(7.1424189846786,-0.169606239833077,4.57655919310821));
#38456=CARTESIAN_POINT('Ctrl Pts',(7.13563219796808,-0.0849767524450092,
4.59350108952231));
#38457=CARTESIAN_POINT('Ctrl Pts',(7.12884541125757,-0.000233413975479213,
4.59320261234329));
#38458=CARTESIAN_POINT('Ctrl Pts',(7.02115458874249,0.000491936389841303,
4.5936290357477));
#38459=CARTESIAN_POINT('Ctrl Pts',(7.03204089516887,-0.135195214358064,
4.59257377495492));
#38460=CARTESIAN_POINT('Ctrl Pts',(7.04292720159524,-0.271531381894462,
4.54641716720817));
#38461=CARTESIAN_POINT('Ctrl Pts',(7.05381350802162,-0.376033620593693,
4.46121547122365));
#38462=CARTESIAN_POINT('Ctrl Pts',(7.06971878670923,-0.528715087097646,
4.33673278019746));
#38463=CARTESIAN_POINT('Ctrl Pts',(7.08562406539685,-0.613443074300594,
4.1289034935015));
#38464=CARTESIAN_POINT('Ctrl Pts',(7.10152934408446,-0.591314251018945,
3.93315398851514));
#38465=CARTESIAN_POINT('Ctrl Pts',(7.11743462277207,-0.569185427737295,
3.73740448352876));
#38466=CARTESIAN_POINT('Ctrl Pts',(7.13333990145968,-0.440199793971044,
3.55373476025198));
#38467=CARTESIAN_POINT('Ctrl Pts',(7.14924518014729,-0.263582002606135,
3.46647820559892));
#38468=CARTESIAN_POINT('Ctrl Pts',(7.16515045883491,-0.0869642112412332,
3.37922165094586));
#38469=CARTESIAN_POINT('Ctrl Pts',(7.18105573752253,0.137285737722324,3.38837826491652));
#38470=CARTESIAN_POINT('Ctrl Pts',(7.19696101621014,0.306201705590428,3.48974370695041));
#38471=CARTESIAN_POINT('Ctrl Pts',(7.21286629489775,0.47511767345854,3.59110914898431));
#38472=CARTESIAN_POINT('Ctrl Pts',(7.22877157358536,0.588699660231196,3.78468341908144));
#38473=CARTESIAN_POINT('Ctrl Pts',(7.24467685227297,0.594795648982816,3.98158540759));
#38474=CARTESIAN_POINT('Ctrl Pts',(7.26058213096058,0.600891637734436,4.17848739609855));
#38475=CARTESIAN_POINT('Ctrl Pts',(7.2764874096482,0.499501628465021,4.37871710301853));
#38476=CARTESIAN_POINT('Ctrl Pts',(7.29239268833581,0.337179610128186,4.49033751492072));
#38477=CARTESIAN_POINT('Ctrl Pts',(7.30197998847137,0.239335998647354,4.5576194790522));
#38478=CARTESIAN_POINT('Ctrl Pts',(7.31156728860693,0.119353510611835,4.59270637405629));
#38479=CARTESIAN_POINT('Ctrl Pts',(7.32115458874249,-0.000317338366111653,
4.59328419319629));
#38480=CARTESIAN_POINT('Origin',(4.,0.,4.));
#38481=CARTESIAN_POINT('',(7.72884541125757,0.000455182276646732,4.59460030787683));
#38482=CARTESIAN_POINT('',(7.62115458874249,-0.000367422317862595,4.59479267874092));
#38483=CARTESIAN_POINT('',(4.,-7.27562663373442E-17,4.5941));
#38484=CARTESIAN_POINT('Ctrl Pts',(7.72884541125757,0.000455182276646732,
4.59460030787683));
#38485=CARTESIAN_POINT('Ctrl Pts',(7.72649554221944,0.0296217258780686,
4.59484761241511));
#38486=CARTESIAN_POINT('Ctrl Pts',(7.72414567318131,0.0587549042441869,
4.59288776399295));
#38487=CARTESIAN_POINT('Ctrl Pts',(7.72179580414318,0.0875427725731367,
4.58860617484604));
#38488=CARTESIAN_POINT('Ctrl Pts',(7.70589052545556,0.282395788279217,4.55962589232715));
#38489=CARTESIAN_POINT('Ctrl Pts',(7.68998524676794,0.461428877889185,4.42427810603975));
#38490=CARTESIAN_POINT('Ctrl Pts',(7.67407996808033,0.542437620895056,4.24470879335187));
#38491=CARTESIAN_POINT('Ctrl Pts',(7.65817468939272,0.623446363900926,4.065139480664));
#38492=CARTESIAN_POINT('Ctrl Pts',(7.64226941070511,0.606430760302702,3.84134864157567));
#38493=CARTESIAN_POINT('Ctrl Pts',(7.6263641320175,0.499203655448083,3.67609156159133));
#38494=CARTESIAN_POINT('Ctrl Pts',(7.61045885332988,0.391976550593464,3.51083448160699));
#38495=CARTESIAN_POINT('Ctrl Pts',(7.59455357464227,0.19453794448245,3.40411116072664));
#38496=CARTESIAN_POINT('Ctrl Pts',(7.57864829595466,-0.00245670798462758,
3.40492443279829));
#38497=CARTESIAN_POINT('Ctrl Pts',(7.56274301726704,-0.199451360451705,
3.40573770486994));
#38498=CARTESIAN_POINT('Ctrl Pts',(7.54683773857943,-0.396002059274846,
3.5140875698936));
#38499=CARTESIAN_POINT('Ctrl Pts',(7.53093245989182,-0.50186103876401,3.68022435377194));
#38500=CARTESIAN_POINT('Ctrl Pts',(7.51502718120421,-0.607720018253171,
3.84636113765028));
#38501=CARTESIAN_POINT('Ctrl Pts',(7.4991219025166,-0.622887278408357,4.07028484038331));
#38502=CARTESIAN_POINT('Ctrl Pts',(7.48321662382898,-0.540398655351294,
4.24917917107494));
#38503=CARTESIAN_POINT('Ctrl Pts',(7.46731134514137,-0.45791003229423,4.42807350176658));
#38504=CARTESIAN_POINT('Ctrl Pts',(7.45140606645375,-0.277765526024924,
4.56193846041682));
#38505=CARTESIAN_POINT('Ctrl Pts',(7.43550078776614,-0.0826798719492015,
4.58930892143267));
#38506=CARTESIAN_POINT('Ctrl Pts',(7.43328232892995,-0.0554694406452989,
4.59312653709876));
#38507=CARTESIAN_POINT('Ctrl Pts',(7.43106387009376,-0.0279683367079049,
4.5948723550368));
#38508=CARTESIAN_POINT('Ctrl Pts',(7.42884541125756,-0.000438237927964824,
4.59464495791636));
#38509=CARTESIAN_POINT('Ctrl Pts',(7.32115458874249,-0.000317338366111653,
4.59328419319629));
#38510=CARTESIAN_POINT('Ctrl Pts',(7.32747256729455,-0.0791797758050172,
4.59366497286126));
#38511=CARTESIAN_POINT('Ctrl Pts',(7.3337905458466,-0.157906876560309,4.57905936436794));
#38512=CARTESIAN_POINT('Ctrl Pts',(7.34010852439865,-0.230073660466993,
4.54880513582638));
#38513=CARTESIAN_POINT('Ctrl Pts',(7.35601380308626,-0.411750885321067,
4.47264122794544));
#38514=CARTESIAN_POINT('Ctrl Pts',(7.37191908177388,-0.551851307624962,
4.29730229529918));
#38515=CARTESIAN_POINT('Ctrl Pts',(7.38782436046149,-0.586046744500155,
4.10329655692985));
#38516=CARTESIAN_POINT('Ctrl Pts',(7.4037296391491,-0.620242181375348,3.90929081856053));
#38517=CARTESIAN_POINT('Ctrl Pts',(7.41963491783671,-0.548532632821828,
3.69661827446815));
#38518=CARTESIAN_POINT('Ctrl Pts',(7.43554019652432,-0.403844087697925,
3.56292915991696));
#38519=CARTESIAN_POINT('Ctrl Pts',(7.45144547521194,-0.259155542574025,
3.42924004536577));
#38520=CARTESIAN_POINT('Ctrl Pts',(7.46735075389955,-0.0414880008797467,
3.37453436035576));
#38521=CARTESIAN_POINT('Ctrl Pts',(7.48325603258717,0.149214809903968,3.42393064079835));
#38522=CARTESIAN_POINT('Ctrl Pts',(7.49916131127478,0.339917620687686,3.47332692124094));
#38523=CARTESIAN_POINT('Ctrl Pts',(7.51506658996239,0.50365570056084,3.62682516713614));
#38524=CARTESIAN_POINT('Ctrl Pts',(7.53097186865001,0.56524745100941,3.81394547807041));
#38525=CARTESIAN_POINT('Ctrl Pts',(7.54687714733762,0.626839201457978,4.00106578900469));
#38526=CARTESIAN_POINT('Ctrl Pts',(7.56278242602523,0.58628462248197,4.22180816497804));
#38527=CARTESIAN_POINT('Ctrl Pts',(7.57868770471284,0.462204660718925,4.3748170457164));
#38528=CARTESIAN_POINT('Ctrl Pts',(7.59284333272272,0.351774041004839,4.51099427596058));
#38529=CARTESIAN_POINT('Ctrl Pts',(7.60699896073261,0.175183620117616,4.59352033541115));
#38530=CARTESIAN_POINT('Ctrl Pts',(7.62115458874249,-0.000367422317862596,
4.59479267874092));
#38531=CARTESIAN_POINT('Origin',(4.,0.,4.));
#38532=CARTESIAN_POINT('',(8.02884541125756,0.000208508845897126,4.59318438507865));
#38533=CARTESIAN_POINT('',(7.92115458874249,0.000504499356536197,4.59443266285439));
#38534=CARTESIAN_POINT('',(4.,-7.27562663373442E-17,4.5941));
#38535=CARTESIAN_POINT('Ctrl Pts',(8.02884541125756,0.000208508845897126,
4.59318438507865));
#38536=CARTESIAN_POINT('Ctrl Pts',(8.02192721434511,0.0865993248636432,
4.5934556945658));
#38537=CARTESIAN_POINT('Ctrl Pts',(8.01500901743265,0.17288466952141,4.57582457789876));
#38538=CARTESIAN_POINT('Ctrl Pts',(8.0080908205202,0.250602156771344,4.53974023855861));
#38539=CARTESIAN_POINT('Ctrl Pts',(7.99218554183259,0.42927852421987,4.4567805482338));
#38540=CARTESIAN_POINT('Ctrl Pts',(7.97628026314498,0.562668370741438,4.27628395749428));
#38541=CARTESIAN_POINT('Ctrl Pts',(7.96037498445736,0.589524722071826,4.08112686462655));
#38542=CARTESIAN_POINT('Ctrl Pts',(7.94446970576975,0.616381073402214,3.88596977175883));
#38543=CARTESIAN_POINT('Ctrl Pts',(7.92856442708213,0.536703929541425,3.67615217676291));
#38544=CARTESIAN_POINT('Ctrl Pts',(7.91265914839452,0.387077664089382,3.54801344261061));
#38545=CARTESIAN_POINT('Ctrl Pts',(7.89675386970691,0.237451398637336,3.41987470845831));
#38546=CARTESIAN_POINT('Ctrl Pts',(7.88084859101929,0.0178760115940344,
3.37341483514963));
#38547=CARTESIAN_POINT('Ctrl Pts',(7.86494331233168,-0.170828768780714,
3.42996623095257));
#38548=CARTESIAN_POINT('Ctrl Pts',(7.84903803364407,-0.359533549155462,
3.48651762675552));
#38549=CARTESIAN_POINT('Ctrl Pts',(7.83313275495647,-0.517367722861657,
3.64608029167009));
#38550=CARTESIAN_POINT('Ctrl Pts',(7.81722747626885,-0.571860514742998,
3.83538980050754));
#38551=CARTESIAN_POINT('Ctrl Pts',(7.80132219758124,-0.626353306624339,
4.02469930934499));
#38552=CARTESIAN_POINT('Ctrl Pts',(7.78541691889362,-0.577504716680827,
4.24375566210532));
#38553=CARTESIAN_POINT('Ctrl Pts',(7.769511640206,-0.447743950807975,4.3919774491103));
#38554=CARTESIAN_POINT('Ctrl Pts',(7.75595623055652,-0.337154229471824,
4.51830073342946));
#38555=CARTESIAN_POINT('Ctrl Pts',(7.74240082090705,-0.16779438404434,4.593173711641));
#38556=CARTESIAN_POINT('Ctrl Pts',(7.72884541125757,0.000455182276646732,
4.59460030787683));
#38557=CARTESIAN_POINT('Ctrl Pts',(7.62115458874249,-0.000367422317862596,
4.59479267874092));
#38558=CARTESIAN_POINT('Ctrl Pts',(7.62290423942022,-0.022065717876263,
4.59494994172972));
#38559=CARTESIAN_POINT('Ctrl Pts',(7.62465389009795,-0.043748134618359,
4.59386587358433));
#38560=CARTESIAN_POINT('Ctrl Pts',(7.62640354077568,-0.0652877816099521,
4.59148835294282));
#38561=CARTESIAN_POINT('Ctrl Pts',(7.64230881946329,-0.261094917625702,
4.56987539392751));
#38562=CARTESIAN_POINT('Ctrl Pts',(7.6582140981509,-0.445103845107109,4.44137409039354));
#38563=CARTESIAN_POINT('Ctrl Pts',(7.67411937683852,-0.532825449416136,
4.2649868044631));
#38564=CARTESIAN_POINT('Ctrl Pts',(7.69002465552613,-0.620547053725161,
4.08859951853267));
#38565=CARTESIAN_POINT('Ctrl Pts',(7.70592993421374,-0.611981334861803,
3.86432625020577));
#38566=CARTESIAN_POINT('Ctrl Pts',(7.72183521290136,-0.511061308497056,
3.69514379608856));
#38567=CARTESIAN_POINT('Ctrl Pts',(7.73774049158897,-0.410141282132307,
3.52596134197134));
#38568=CARTESIAN_POINT('Ctrl Pts',(7.75364577027658,-0.216866948266163,
3.4118697020638));
#38569=CARTESIAN_POINT('Ctrl Pts',(7.76955104896419,-0.0199817042712483,
3.40525493058698));
#38570=CARTESIAN_POINT('Ctrl Pts',(7.78545632765181,0.176903539723664,3.39864015911017));
#38571=CARTESIAN_POINT('Ctrl Pts',(7.80136160633942,0.377399693847348,3.49950225606407));
#38572=CARTESIAN_POINT('Ctrl Pts',(7.81726688502703,0.489447406431712,3.66152961365368));
#38573=CARTESIAN_POINT('Ctrl Pts',(7.83317216371464,0.601495119016078,3.82355697124329));
#38574=CARTESIAN_POINT('Ctrl Pts',(7.84907744240226,0.625094390061116,4.04674958946861));
#38575=CARTESIAN_POINT('Ctrl Pts',(7.86498272108987,0.549409432699027,4.22862686054007));
#38576=CARTESIAN_POINT('Ctrl Pts',(7.88088799977748,0.473724475336938,4.41050413161152));
#38577=CARTESIAN_POINT('Ctrl Pts',(7.89679327846509,0.298755289567731,4.55106605552911));
#38578=CARTESIAN_POINT('Ctrl Pts',(7.91269855715271,0.104840323164387,4.58577254351526));
#38579=CARTESIAN_POINT('Ctrl Pts',(7.9155172343493,0.0704753991278659,4.59192310448195));
#38580=CARTESIAN_POINT('Ctrl Pts',(7.91833591154589,0.0355154700816755,
4.59474920414003));
#38581=CARTESIAN_POINT('Ctrl Pts',(7.92115458874249,0.000504499356536197,
4.59443266285439));
#38582=CARTESIAN_POINT('Origin',(4.,0.,4.));
#38583=CARTESIAN_POINT('',(8.32884541125757,-0.000534402448739424,4.5938336238991));
#38584=CARTESIAN_POINT('',(8.2211545887425,0.000116005647334215,4.59313666129657));
#38585=CARTESIAN_POINT('',(4.,-7.27562663373442E-17,4.5941));
#38586=CARTESIAN_POINT('Ctrl Pts',(8.32884541125757,-0.000534402448739424,
4.5938336238991));
#38587=CARTESIAN_POINT('Ctrl Pts',(8.31735888647079,0.142509087977489,4.59259298046846));
#38588=CARTESIAN_POINT('Ctrl Pts',(8.30587236168401,0.286359812054371,4.54070236535691));
#38589=CARTESIAN_POINT('Ctrl Pts',(8.29438583689723,0.393155811111917,4.44670960845581));
#38590=CARTESIAN_POINT('Ctrl Pts',(8.27848055820962,0.541035187969857,4.31655875596735));
#38591=CARTESIAN_POINT('Ctrl Pts',(8.262575279522,0.617867056310918,4.10568264439756));
#38592=CARTESIAN_POINT('Ctrl Pts',(8.24667000083439,0.588373472681163,3.91090666274675));
#38593=CARTESIAN_POINT('Ctrl Pts',(8.23076472214677,0.558879889051408,3.71613068109593));
#38594=CARTESIAN_POINT('Ctrl Pts',(8.21485944345917,0.423060853450833,3.53745482936408));
#38595=CARTESIAN_POINT('Ctrl Pts',(8.19895416477155,0.243278720997716,3.45691949951456));
#38596=CARTESIAN_POINT('Ctrl Pts',(8.18304888608394,0.0634965885445972,
3.37638416966503));
#38597=CARTESIAN_POINT('Ctrl Pts',(8.16714360739632,-0.160248640761069,
3.39398936169784));
#38598=CARTESIAN_POINT('Ctrl Pts',(8.15123832870871,-0.325222623502191,
3.50165151624576));
#38599=CARTESIAN_POINT('Ctrl Pts',(8.1353330500211,-0.490196606243315,3.60931367079368));
#38600=CARTESIAN_POINT('Ctrl Pts',(8.11942777133349,-0.59639934241989,3.80703278785672));
#38601=CARTESIAN_POINT('Ctrl Pts',(8.10352249264588,-0.595067028646789,
4.00402461368555));
#38602=CARTESIAN_POINT('Ctrl Pts',(8.08761721395827,-0.593734714873688,
4.20101643951437));
#38603=CARTESIAN_POINT('Ctrl Pts',(8.07171193527065,-0.484867351150922,
4.39728097410898));
#38604=CARTESIAN_POINT('Ctrl Pts',(8.05580665658303,-0.3184522251018,4.50270184645125));
#38605=CARTESIAN_POINT('Ctrl Pts',(8.04681957480788,-0.224421408301879,
4.56226861162124));
#38606=CARTESIAN_POINT('Ctrl Pts',(8.03783249303272,-0.112017456676448,
4.59283194056482));
#38607=CARTESIAN_POINT('Ctrl Pts',(8.02884541125756,0.000208508845897126,
4.59318438507865));
#38608=CARTESIAN_POINT('Ctrl Pts',(7.92115458874249,0.000504499356536197,
4.59443266285439));
#38609=CARTESIAN_POINT('Ctrl Pts',(7.93424119023351,-0.162045019349314,
4.59296301969496));
#38610=CARTESIAN_POINT('Ctrl Pts',(7.94732779172453,-0.325694779556815,
4.52375140444135));
#38611=CARTESIAN_POINT('Ctrl Pts',(7.96041439321555,-0.436005268305889,
4.40499428651169));
#38612=CARTESIAN_POINT('Ctrl Pts',(7.97631967190316,-0.570075146335334,
4.26065848946726));
#38613=CARTESIAN_POINT('Ctrl Pts',(7.99222495059077,-0.625354155356748,
4.04313584332371));
#38614=CARTESIAN_POINT('Ctrl Pts',(8.00813022927838,-0.576460513088508,
3.85230354456612));
#38615=CARTESIAN_POINT('Ctrl Pts',(8.024035507966,-0.527566870820267,3.66147124580852));
#38616=CARTESIAN_POINT('Ctrl Pts',(8.03994078665361,-0.374500577262366,
3.49732929443689));
#38617=CARTESIAN_POINT('Ctrl Pts',(8.05584606534123,-0.187543198716277,
3.43524473024767));
#38618=CARTESIAN_POINT('Ctrl Pts',(8.07175134402884,-0.000585820170193818,
3.37316016605846));
#38619=CARTESIAN_POINT('Ctrl Pts',(8.08765662271645,0.220262643364076,3.41313298905166));
#38620=CARTESIAN_POINT('Ctrl Pts',(8.10356190140406,0.37359792075985,3.53680937001953));
#38621=CARTESIAN_POINT('Ctrl Pts',(8.11946718009167,0.526933198155627,3.66048575098741));
#38622=CARTESIAN_POINT('Ctrl Pts',(8.13537245877928,0.612755289412907,3.86786568992997));
#38623=CARTESIAN_POINT('Ctrl Pts',(8.1512777374669,0.591658321059451,4.06372909240644));
#38624=CARTESIAN_POINT('Ctrl Pts',(8.16718301615451,0.570561352705995,4.2595924948829));
#38625=CARTESIAN_POINT('Ctrl Pts',(8.18308829484212,0.44254532474181,4.44393936089328));
#38626=CARTESIAN_POINT('Ctrl Pts',(8.19899357352974,0.266389781296621,4.53212540863836));
#38627=CARTESIAN_POINT('Ctrl Pts',(8.20638057860065,0.184576572093718,4.57308230066594));
#38628=CARTESIAN_POINT('Ctrl Pts',(8.21376758367158,0.0923795717789203,
4.59329710918813));
#38629=CARTESIAN_POINT('Ctrl Pts',(8.2211545887425,0.000116005647334215,
4.59313666129657));
#38630=CARTESIAN_POINT('Origin',(4.,0.,4.));
#38631=CARTESIAN_POINT('',(8.62884541125757,3.48566139269993E-5,4.59507810043999));
#38632=CARTESIAN_POINT('',(8.5211545887425,-0.000547905086566465,4.594005652201));
#38633=CARTESIAN_POINT('',(4.,-7.27562663373442E-17,4.5941));
#38634=CARTESIAN_POINT('Ctrl Pts',(8.62884541125757,3.48566139269993E-5,
4.59507810043999));
#38635=CARTESIAN_POINT('Ctrl Pts',(8.62869583728408,0.00188744051982823,
4.59507966949126));
#38636=CARTESIAN_POINT('Ctrl Pts',(8.62854626331059,0.00374001065808006,
4.59507176912216));
#38637=CARTESIAN_POINT('Ctrl Pts',(8.6283966893371,0.00559249142073073,
4.59505435897699));
#38638=CARTESIAN_POINT('Ctrl Pts',(8.61249141064948,0.202580123064263,4.59320301275402));
#38639=CARTESIAN_POINT('Ctrl Pts',(8.59658613196187,0.398557131004382,4.48381890612783));
#38640=CARTESIAN_POINT('Ctrl Pts',(8.58068085327426,0.503539164298441,4.31712659320126));
#38641=CARTESIAN_POINT('Ctrl Pts',(8.56477557458664,0.608521197592498,4.15043428027469));
#38642=CARTESIAN_POINT('Ctrl Pts',(8.54887029589904,0.622508256240502,3.92643376104774));
#38643=CARTESIAN_POINT('Ctrl Pts',(8.53296501721142,0.539078074654942,3.74797659726896));
#38644=CARTESIAN_POINT('Ctrl Pts',(8.51705973852381,0.455647893069379,3.56951943349019));
#38645=CARTESIAN_POINT('Ctrl Pts',(8.50115445983619,0.274800471250253,3.43660562515959));
#38646=CARTESIAN_POINT('Ctrl Pts',(8.48524918114857,0.0795732942734406,
3.41026356994308));
#38647=CARTESIAN_POINT('Ctrl Pts',(8.46934390246096,-0.115653882703369,
3.38392151472657));
#38648=CARTESIAN_POINT('Ctrl Pts',(8.45343862377335,-0.32526081483786,3.46415121262414));
#38649=CARTESIAN_POINT('Ctrl Pts',(8.43753334508574,-0.453004866631874,
3.61411458059983));
#38650=CARTESIAN_POINT('Ctrl Pts',(8.42162806639813,-0.580748918425883,
3.76407794857552));
#38651=CARTESIAN_POINT('Ctrl Pts',(8.40572278771052,-0.626630089879422,
3.98377498662932));
#38652=CARTESIAN_POINT('Ctrl Pts',(8.3898175090229,-0.569581688133314,4.17233010950212));
#38653=CARTESIAN_POINT('Ctrl Pts',(8.37391223033529,-0.512533286387202,
4.36088523237493));
#38654=CARTESIAN_POINT('Ctrl Pts',(8.35800695164768,-0.352555311441432,
4.51829844006673));
#38655=CARTESIAN_POINT('Ctrl Pts',(8.34210167296007,-0.163102881281137,
4.57229224720906));
#38656=CARTESIAN_POINT('Ctrl Pts',(8.33768291905923,-0.110469810133188,
4.58729263485501));
#38657=CARTESIAN_POINT('Ctrl Pts',(8.3332641651584,-0.0555618361628184,
4.59431088730997));
#38658=CARTESIAN_POINT('Ctrl Pts',(8.32884541125757,-0.000534402448739424,
4.5938336238991));
#38659=CARTESIAN_POINT('Ctrl Pts',(8.2211545887425,0.000116005647334215,
4.59313666129657));
#38660=CARTESIAN_POINT('Ctrl Pts',(8.22967286235919,-0.106277085140544,
4.59295164192424));
#38661=CARTESIAN_POINT('Ctrl Pts',(8.23819113597589,-0.212758691085218,
4.56567285125378));
#38662=CARTESIAN_POINT('Ctrl Pts',(8.24670940959258,-0.303508593564514,
4.51186277431583));
#38663=CARTESIAN_POINT('Ctrl Pts',(8.26261468828019,-0.472956366054245,
4.41138886276846));
#38664=CARTESIAN_POINT('Ctrl Pts',(8.2785199669678,-0.587556852107514,4.21841581019395));
#38665=CARTESIAN_POINT('Ctrl Pts',(8.29442524565541,-0.594690356875377,
4.02154867831793));
#38666=CARTESIAN_POINT('Ctrl Pts',(8.31033052434302,-0.60182386164324,3.82468154644191));
#38667=CARTESIAN_POINT('Ctrl Pts',(8.32623580303064,-0.501490385125681,
3.62392033526436));
#38668=CARTESIAN_POINT('Ctrl Pts',(8.34214108171825,-0.339758814980244,
3.51144609945163));
#38669=CARTESIAN_POINT('Ctrl Pts',(8.35804636040587,-0.178027244834812,
3.3989718636389));
#38670=CARTESIAN_POINT('Ctrl Pts',(8.37395163909348,0.0451024189384938,
3.37478460319097));
#38671=CARTESIAN_POINT('Ctrl Pts',(8.38985691778109,0.227178474572579,3.44999008482693));
#38672=CARTESIAN_POINT('Ctrl Pts',(8.4057621964687,0.40925453020667,3.5251955664629));
#38673=CARTESIAN_POINT('Ctrl Pts',(8.42166747515631,0.550276977701535,3.69979379018275));
#38674=CARTESIAN_POINT('Ctrl Pts',(8.43757275384392,0.585494275335268,3.89361663829603));
#38675=CARTESIAN_POINT('Ctrl Pts',(8.45347803253154,0.620711572969,4.0874394864093));
#38676=CARTESIAN_POINT('Ctrl Pts',(8.46938331121915,0.550123720741606,4.30048695891599));
#38677=CARTESIAN_POINT('Ctrl Pts',(8.48528858990677,0.406141674070155,4.4349366697363));
#38678=CARTESIAN_POINT('Ctrl Pts',(8.49724392285201,0.297916389879728,4.53599689564107));
#38679=CARTESIAN_POINT('Ctrl Pts',(8.50919925579725,0.148224117540273,4.59265016978245));
#38680=CARTESIAN_POINT('Ctrl Pts',(8.5211545887425,-0.000547905086566465,
4.594005652201));
#38681=CARTESIAN_POINT('Origin',(4.,0.,4.));
#38682=CARTESIAN_POINT('',(8.92884541125757,0.000516595407308196,4.59372894893997));
#38683=CARTESIAN_POINT('',(8.82115458874249,0.000142235148737217,4.59503945166131));
#38684=CARTESIAN_POINT('',(4.,-7.27562663373442E-17,4.5941));
#38685=CARTESIAN_POINT('Ctrl Pts',(8.92884541125757,0.000516595407308196,
4.59372894893997));
#38686=CARTESIAN_POINT('Ctrl Pts',(8.92412750940976,0.0592956068199462,
4.59421507565108));
#38687=CARTESIAN_POINT('Ctrl Pts',(8.91940960756194,0.117944888069788,4.58619493689145));
#38688=CARTESIAN_POINT('Ctrl Pts',(8.91469170571413,0.17383025386194,4.56912565303288));
#38689=CARTESIAN_POINT('Ctrl Pts',(8.89878642702651,0.362234410233906,4.51158064138869));
#38690=CARTESIAN_POINT('Ctrl Pts',(8.8828811483389,0.519225559109383,4.35118846702123));
#38691=CARTESIAN_POINT('Ctrl Pts',(8.86697586965128,0.572720006672535,4.16159443076672));
#38692=CARTESIAN_POINT('Ctrl Pts',(8.85107059096367,0.626214454235688,3.97200039451221));
#38693=CARTESIAN_POINT('Ctrl Pts',(8.83516531227606,0.576212200486512,3.75320449637065));
#38694=CARTESIAN_POINT('Ctrl Pts',(8.81926003358845,0.445672164925724,3.60566855627755));
#38695=CARTESIAN_POINT('Ctrl Pts',(8.80335475490084,0.315132129364936,3.45813261618446));
#38696=CARTESIAN_POINT('Ctrl Pts',(8.78744947621322,0.104054311992536,3.38185663413984));
#38697=CARTESIAN_POINT('Ctrl Pts',(8.77154419752561,-0.0906432834200916,
3.41186331412789));
#38698=CARTESIAN_POINT('Ctrl Pts',(8.755638918838,-0.285340878832719,3.44186999411594));
#38699=CARTESIAN_POINT('Ctrl Pts',(8.73973364015038,-0.463658252285575,
3.57815933613666));
#38700=CARTESIAN_POINT('Ctrl Pts',(8.72382836146277,-0.543719609875046,
3.75815304026071));
#38701=CARTESIAN_POINT('Ctrl Pts',(8.70792308277515,-0.623780967464517,
3.93814674438476));
#38702=CARTESIAN_POINT('Ctrl Pts',(8.69201780408754,-0.605586309190603,
4.16184481061213));
#38703=CARTESIAN_POINT('Ctrl Pts',(8.67611252539993,-0.497489852380174,
4.32653455081593));
#38704=CARTESIAN_POINT('Ctrl Pts',(8.66035682068581,-0.390409939629295,
4.48967554111606));
#38705=CARTESIAN_POINT('Ctrl Pts',(8.64460111597169,-0.195111159088962,
4.59491282095998));
#38706=CARTESIAN_POINT('Ctrl Pts',(8.62884541125757,3.48566139269993E-5,
4.59507810043999));
#38707=CARTESIAN_POINT('Ctrl Pts',(8.5211545887425,-0.000547905086566465,
4.594005652201));
#38708=CARTESIAN_POINT('Ctrl Pts',(8.52510453448487,-0.0497009834700827,
4.59445349267793));
#38709=CARTESIAN_POINT('Ctrl Pts',(8.52905448022724,-0.0987536084630192,
4.58886509038946));
#38710=CARTESIAN_POINT('Ctrl Pts',(8.53300442596961,-0.146177075786514,
4.57684766499685));
#38711=CARTESIAN_POINT('Ctrl Pts',(8.54890970465722,-0.337137537856201,
4.52845700030318));
#38712=CARTESIAN_POINT('Ctrl Pts',(8.56481498334483,-0.501682220880061,
4.37582372178193));
#38713=CARTESIAN_POINT('Ctrl Pts',(8.58072026203244,-0.564259167724997,
4.18903057354857));
#38714=CARTESIAN_POINT('Ctrl Pts',(8.59662554072005,-0.626836114569933,
4.00223742531521));
#38715=CARTESIAN_POINT('Ctrl Pts',(8.61253081940767,-0.587445325235947,
3.78128440736974));
#38716=CARTESIAN_POINT('Ctrl Pts',(8.62843609809528,-0.464173383698336,
3.62762379780141));
#38717=CARTESIAN_POINT('Ctrl Pts',(8.6443413767829,-0.340901442160722,3.47396318823307));
#38718=CARTESIAN_POINT('Ctrl Pts',(8.66024665547051,-0.133748348419481,
3.38759498704188));
#38719=CARTESIAN_POINT('Ctrl Pts',(8.67615193415812,0.0621699608040676,
3.40817581827756));
#38720=CARTESIAN_POINT('Ctrl Pts',(8.69205721284573,0.25808827002761,3.42875664951325));
#38721=CARTESIAN_POINT('Ctrl Pts',(8.70796249153334,0.44277179473346,3.55628651317581));
#38722=CARTESIAN_POINT('Ctrl Pts',(8.72386777022095,0.531421673692279,3.73220909121499));
#38723=CARTESIAN_POINT('Ctrl Pts',(8.73977304890857,0.620071552651101,3.90813166925417));
#38724=CARTESIAN_POINT('Ctrl Pts',(8.75567832759618,0.612687785862888,4.13244696166997));
#38725=CARTESIAN_POINT('Ctrl Pts',(8.7715836062838,0.512660686655375,4.30215887618246));
#38726=CARTESIAN_POINT('Ctrl Pts',(8.78748888497141,0.412633587447865,4.47187079069495));
#38727=CARTESIAN_POINT('Ctrl Pts',(8.80339416365902,0.21996315582106,4.58697932730413));
#38728=CARTESIAN_POINT('Ctrl Pts',(8.81929944234663,0.0231155027642346,
4.59463151583965));
#38729=CARTESIAN_POINT('Ctrl Pts',(8.81991782447859,0.0154622529370322,
4.59492902566351));
#38730=CARTESIAN_POINT('Ctrl Pts',(8.82053620661054,0.00780268890311657,
4.59506410656044));
#38731=CARTESIAN_POINT('Ctrl Pts',(8.82115458874249,0.000142235148737217,
4.59503945166131));
#38732=CARTESIAN_POINT('Origin',(4.,0.,4.));
#38733=CARTESIAN_POINT('',(9.22884541125756,-0.000264402795292107,4.59322887297718));
#38734=CARTESIAN_POINT('',(9.12115458874249,0.000475196148639644,4.59357609051269));
#38735=CARTESIAN_POINT('',(4.,-7.27562663373442E-17,4.5941));
#38736=CARTESIAN_POINT('Ctrl Pts',(9.22884541125756,-0.000264402795292107,
4.59322887297718));
#38737=CARTESIAN_POINT('Ctrl Pts',(9.21955918153543,0.115675446261185,4.59276508993807));
#38738=CARTESIAN_POINT('Ctrl Pts',(9.21027295181329,0.231857423975292,4.55999255403315));
#38739=CARTESIAN_POINT('Ctrl Pts',(9.20098672209116,0.327844211240712,4.49662776730038));
#38740=CARTESIAN_POINT('Ctrl Pts',(9.18508144340355,0.492248565587605,4.38809775866155));
#38741=CARTESIAN_POINT('Ctrl Pts',(9.16917616471593,0.597407924103304,4.18982173958679));
#38742=CARTESIAN_POINT('Ctrl Pts',(9.15327088602831,0.595037558282966,3.99283966966863));
#38743=CARTESIAN_POINT('Ctrl Pts',(9.1373656073407,0.592667192462628,3.79585759975047));
#38744=CARTESIAN_POINT('Ctrl Pts',(9.12146032865309,0.482767102306254,3.60016947898891));
#38745=CARTESIAN_POINT('Ctrl Pts',(9.10555504996548,0.315798759724268,3.49562701355602));
#38746=CARTESIAN_POINT('Ctrl Pts',(9.08964977127787,0.148830417142278,3.39108454812312));
#38747=CARTESIAN_POINT('Ctrl Pts',(9.07374449259025,-0.0752061778653251,
3.37768773801888));
#38748=CARTESIAN_POINT('Ctrl Pts',(9.05783921390264,-0.253442899077741,
3.46158783167087));
#38749=CARTESIAN_POINT('Ctrl Pts',(9.04193393521502,-0.431679620290152,
3.54548792532286));
#38750=CARTESIAN_POINT('Ctrl Pts',(9.02602865652741,-0.56411646770738,3.72668492273107));
#38751=CARTESIAN_POINT('Ctrl Pts',(9.0101233778398,-0.589944043936388,3.92198082849844));
#38752=CARTESIAN_POINT('Ctrl Pts',(8.99421809915219,-0.615771620165397,
4.11727673426582));
#38753=CARTESIAN_POINT('Ctrl Pts',(8.97831282046457,-0.534989925206181,
4.32667154839236));
#38754=CARTESIAN_POINT('Ctrl Pts',(8.96240754177696,-0.384690495792338,
4.45402003099517));
#38755=CARTESIAN_POINT('Ctrl Pts',(8.95122016493716,-0.278973620993485,
4.54359378149875));
#38756=CARTESIAN_POINT('Ctrl Pts',(8.94003278809737,-0.138863784294423,
4.59257621560968));
#38757=CARTESIAN_POINT('Ctrl Pts',(8.92884541125757,0.000516595407308196,
4.59372894893997));
#38758=CARTESIAN_POINT('Ctrl Pts',(8.82115458874249,0.000142235148737217,
4.59503945166131));
#38759=CARTESIAN_POINT('Ctrl Pts',(8.83644148529816,-0.189230254871984,
4.59442996300828));
#38760=CARTESIAN_POINT('Ctrl Pts',(8.85172838185382,-0.379146468724227,
4.49620311855542));
#38761=CARTESIAN_POINT('Ctrl Pts',(8.86701527840948,-0.487657002993039,
4.34104488491935));
#38762=CARTESIAN_POINT('Ctrl Pts',(8.88292055709709,-0.600556981206626,
4.17961022500168));
#38763=CARTESIAN_POINT('Ctrl Pts',(8.89882583578469,-0.62533206314696,3.95654506470448));
#38764=CARTESIAN_POINT('Ctrl Pts',(8.91473111447231,-0.550606579334316,
3.77427148852754));
#38765=CARTESIAN_POINT('Ctrl Pts',(8.93063639315992,-0.47588109552167,3.5919979123506));
#38766=CARTESIAN_POINT('Ctrl Pts',(8.94654167184753,-0.301655045956043,
3.45051592029392));
#38767=CARTESIAN_POINT('Ctrl Pts',(8.96244695053515,-0.107925661701669,
3.41478805750048));
#38768=CARTESIAN_POINT('Ctrl Pts',(8.97835222922276,0.0858037225526985,
3.37906019470703));
#38769=CARTESIAN_POINT('Ctrl Pts',(8.99425750791037,0.299036441495806,3.4490864611768));
#38770=CARTESIAN_POINT('Ctrl Pts',(9.01016278659798,0.433865051721373,3.5927137579139));
#38771=CARTESIAN_POINT('Ctrl Pts',(9.0260680652856,0.568693661946943,3.736341054651));
#38772=CARTESIAN_POINT('Ctrl Pts',(9.04197334397321,0.625118163454969,3.95356938165542));
#38773=CARTESIAN_POINT('Ctrl Pts',(9.05787862266082,0.577230812276762,4.14465668133936));
#38774=CARTESIAN_POINT('Ctrl Pts',(9.07378390134844,0.529343461098555,4.3357439810233));
#38775=CARTESIAN_POINT('Ctrl Pts',(9.08968918003605,0.377144257234124,4.50069025338676));
#38776=CARTESIAN_POINT('Ctrl Pts',(9.10559445872366,0.190516636080703,4.56375914846174));
#38777=CARTESIAN_POINT('Ctrl Pts',(9.11078116872994,0.129657384941762,4.58432590969837));
#38778=CARTESIAN_POINT('Ctrl Pts',(9.11596787873622,0.0651369761893139,
4.59405891310139));
#38779=CARTESIAN_POINT('Ctrl Pts',(9.12115458874249,0.000475196148639644,
4.59357609051269));
#38780=CARTESIAN_POINT('Origin',(4.,0.,4.));
#38781=CARTESIAN_POINT('',(9.52884541125756,-0.000414715089906426,4.59470005288553));
#38782=CARTESIAN_POINT('',(9.4211545887425,-0.000345133784900094,4.59331940772745));
#38783=CARTESIAN_POINT('',(4.,-7.27562663373442E-17,4.5941));
#38784=CARTESIAN_POINT('Ctrl Pts',(9.52884541125756,-0.000414715089906426,
4.59470005288553));
#38785=CARTESIAN_POINT('Ctrl Pts',(9.5149908536611,0.17147269131647,4.59333531965569));
#38786=CARTESIAN_POINT('Ctrl Pts',(9.50113629606464,0.344448366351018,4.51470554290992));
#38787=CARTESIAN_POINT('Ctrl Pts',(9.48728173846818,0.455032043431697,4.38349290156166));
#38788=CARTESIAN_POINT('Ctrl Pts',(9.47137645978057,0.581984072756561,4.23285845412795));
#38789=CARTESIAN_POINT('Ctrl Pts',(9.45547118109296,0.626706888961734,4.01292269047354));
#38790=CARTESIAN_POINT('Ctrl Pts',(9.43956590240535,0.56866566691212,3.82467080855373));
#38791=CARTESIAN_POINT('Ctrl Pts',(9.42366062371773,0.510624444862503,3.63641892663391));
#38792=CARTESIAN_POINT('Ctrl Pts',(9.40775534503012,0.349819184558098,3.47985092644869));
#38793=CARTESIAN_POINT('Ctrl Pts',(9.39185006634251,0.160084858421151,3.42685620983728));
#38794=CARTESIAN_POINT('Ctrl Pts',(9.37594478765489,-0.0296494677157886,
3.37386149322587));
#38795=CARTESIAN_POINT('Ctrl Pts',(9.36003950896728,-0.248312859685263,
3.42444006018826));
#38796=CARTESIAN_POINT('Ctrl Pts',(9.34413423027966,-0.395504338780113,
3.55536837257802));
#38797=CARTESIAN_POINT('Ctrl Pts',(9.32822895159205,-0.542695817874971,
3.6862966849678));
#38798=CARTESIAN_POINT('Ctrl Pts',(9.31232367290444,-0.618415384095196,
3.89757474278496));
#38799=CARTESIAN_POINT('Ctrl Pts',(9.29641839421683,-0.587895816063128,
4.09219260031737));
#38800=CARTESIAN_POINT('Ctrl Pts',(9.28051311552922,-0.55737624803106,4.28681045784976));
#38801=CARTESIAN_POINT('Ctrl Pts',(9.26460783684159,-0.42061754574671,4.4647681150974));
#38802=CARTESIAN_POINT('Ctrl Pts',(9.24870255815398,-0.240413519515492,
4.54435494461976));
#38803=CARTESIAN_POINT('Ctrl Pts',(9.24208350918851,-0.165420852186184,
4.57747534017911));
#38804=CARTESIAN_POINT('Ctrl Pts',(9.23546446022304,-0.0829041350566004,
4.59355944875842));
#38805=CARTESIAN_POINT('Ctrl Pts',(9.22884541125756,-0.000264402795292107,
4.59322887297718));
#38806=CARTESIAN_POINT('Ctrl Pts',(9.12115458874249,0.000475196148639644,
4.59357609051269));
#38807=CARTESIAN_POINT('Ctrl Pts',(9.13187315742383,-0.133151270259641,
4.59257831599443));
#38808=CARTESIAN_POINT('Ctrl Pts',(9.14259172610516,-0.267381477949042,
4.54795275857003));
#38809=CARTESIAN_POINT('Ctrl Pts',(9.1533102947865,-0.371151898503526,4.46515291500219));
#38810=CARTESIAN_POINT('Ctrl Pts',(9.16921557347411,-0.525136773491911,
4.34228626868117));
#38811=CARTESIAN_POINT('Ctrl Pts',(9.18512085216173,-0.612050485026272,
4.13536145825263));
#38812=CARTESIAN_POINT('Ctrl Pts',(9.20102613084934,-0.591985933785934,
3.93938960239856));
#38813=CARTESIAN_POINT('Ctrl Pts',(9.21693140953695,-0.571921382545595,
3.74341774654449));
#38814=CARTESIAN_POINT('Ctrl Pts',(9.23283668822456,-0.444878568530549,
3.55839884526489));
#38815=CARTESIAN_POINT('Ctrl Pts',(9.24874196691217,-0.269190177198291,
3.46928575052316));
#38816=CARTESIAN_POINT('Ctrl Pts',(9.26464724559978,-0.0935017858660342,
3.38017265578144));
#38817=CARTESIAN_POINT('Ctrl Pts',(9.28055252428739,0.130832182783434,3.38696536757758));
#38818=CARTESIAN_POINT('Ctrl Pts',(9.29645780297501,0.300807061133818,3.48654496003073));
#38819=CARTESIAN_POINT('Ctrl Pts',(9.31236308166262,0.470781939484206,3.58612455248389));
#38820=CARTESIAN_POINT('Ctrl Pts',(9.32826836035024,0.586397727535503,3.77849102559406));
#38821=CARTESIAN_POINT('Ctrl Pts',(9.34417363903785,0.594568546715174,3.97531783326339));
#38822=CARTESIAN_POINT('Ctrl Pts',(9.36007891772546,0.602739365894845,4.17214464093271));
#38823=CARTESIAN_POINT('Ctrl Pts',(9.37598419641307,0.503465216202894,4.37343178316119));
#38824=CARTESIAN_POINT('Ctrl Pts',(9.39188947510069,0.342328587234952,4.48675671999422));
#38825=CARTESIAN_POINT('Ctrl Pts',(9.40164451298129,0.243500144778355,4.55626125828842));
#38826=CARTESIAN_POINT('Ctrl Pts',(9.41139955086189,0.121401365174849,4.59267772446372));
#38827=CARTESIAN_POINT('Ctrl Pts',(9.4211545887425,-0.000345133784900094,
4.59331940772745));
#38828=CARTESIAN_POINT('Origin',(4.,0.,4.));
#38829=CARTESIAN_POINT('',(9.82884541125756,0.000474857175501747,4.59454166667424));
#38830=CARTESIAN_POINT('',(9.7211545887425,-0.000338423355870402,4.59484023865297));
#38831=CARTESIAN_POINT('',(4.,-7.27562663373442E-17,4.5941));
#38832=CARTESIAN_POINT('Ctrl Pts',(9.82884541125756,0.000474857175501747,
4.59454166667424));
#38833=CARTESIAN_POINT('Ctrl Pts',(9.82632780447438,0.0317313679687054,
4.59481419231428));
#38834=CARTESIAN_POINT('Ctrl Pts',(9.82381019769121,0.0629485386443197,
4.59256288124703));
#38835=CARTESIAN_POINT('Ctrl Pts',(9.82129259090804,0.093741277189286,4.58765086492638));
#38836=CARTESIAN_POINT('Ctrl Pts',(9.80538731222043,0.288278045752977,4.55661862072519));
#38837=CARTESIAN_POINT('Ctrl Pts',(9.78948203353282,0.465874751366426,4.41939150759219));
#38838=CARTESIAN_POINT('Ctrl Pts',(9.77357675484521,0.54498650030893,4.23897841027765));
#38839=CARTESIAN_POINT('Ctrl Pts',(9.7576714761576,0.624098249251433,4.05856531296313));
#38840=CARTESIAN_POINT('Ctrl Pts',(9.74176619746998,0.604725041522997,3.83496623146707));
#38841=CARTESIAN_POINT('Ctrl Pts',(9.72586091878237,0.495762234499694,3.67084840431546));
#38842=CARTESIAN_POINT('Ctrl Pts',(9.70995564009475,0.386799427476386,3.50673057716384));
#38843=CARTESIAN_POINT('Ctrl Pts',(9.69405036140714,0.188247021158209,3.40209400435668));
#38844=CARTESIAN_POINT('Ctrl Pts',(9.67814508271953,-0.00872811953311764,
3.40498337331868));
#38845=CARTESIAN_POINT('Ctrl Pts',(9.66223980403192,-0.205703260224436,
3.40787274228067));
#38846=CARTESIAN_POINT('Ctrl Pts',(9.6463345253443,-0.4011011352889,3.51828805301183));
#38847=CARTESIAN_POINT('Ctrl Pts',(9.63042924665669,-0.505203307099277,
3.68553126611098));
#38848=CARTESIAN_POINT('Ctrl Pts',(9.61452396796908,-0.609305478909656,
3.85277447921013));
#38849=CARTESIAN_POINT('Ctrl Pts',(9.59861868928147,-0.622111947465945,
4.07684559467727));
#38850=CARTESIAN_POINT('Ctrl Pts',(9.58271341059386,-0.537742524204099,
4.25486063595701));
#38851=CARTESIAN_POINT('Ctrl Pts',(9.56680813190624,-0.453373100942255,
4.43287567723675));
#38852=CARTESIAN_POINT('Ctrl Pts',(9.55090285321863,-0.271827785862281,
4.5648346443291));
#38853=CARTESIAN_POINT('Ctrl Pts',(9.53499757453102,-0.0764645071000137,
4.59014756226876));
#38854=CARTESIAN_POINT('Ctrl Pts',(9.53294685343987,-0.0512756623106346,
4.5934112419387));
#38855=CARTESIAN_POINT('Ctrl Pts',(9.53089613234871,-0.025857110284879,
4.59490205769144));
#38856=CARTESIAN_POINT('Ctrl Pts',(9.52884541125756,-0.000414715089906426,
4.59470005288553));
#38857=CARTESIAN_POINT('Ctrl Pts',(9.4211545887425,-0.000345133784900094,
4.59331940772745));
#38858=CARTESIAN_POINT('Ctrl Pts',(9.42730482954951,-0.0771024252662454,
4.59372396859559));
#38859=CARTESIAN_POINT('Ctrl Pts',(9.43345507035652,-0.153719688677923,
4.57990840728947));
#38860=CARTESIAN_POINT('Ctrl Pts',(9.43960531116353,-0.224276981305518,
4.55119942103951));
#38861=CARTESIAN_POINT('Ctrl Pts',(9.45551058985114,-0.406746812634079,
4.47695445381419));
#38862=CARTESIAN_POINT('Ctrl Pts',(9.47141586853875,-0.548687367047265,
4.30310178792596));
#38863=CARTESIAN_POINT('Ctrl Pts',(9.48732114722636,-0.58492554696818,4.10946721245096));
#38864=CARTESIAN_POINT('Ctrl Pts',(9.50322642591398,-0.621163726889096,
3.91583263697596));
#38865=CARTESIAN_POINT('Ctrl Pts',(9.5191317046016,-0.55169953231774,3.70241615191419));
#38866=CARTESIAN_POINT('Ctrl Pts',(9.53503698328921,-0.408427982613559,
3.56720957829912));
#38867=CARTESIAN_POINT('Ctrl Pts',(9.55094226197682,-0.265156432909381,
3.43200300468405));
#38868=CARTESIAN_POINT('Ctrl Pts',(9.56684754066442,-0.0480775280723801,
3.37500634251568));
#38869=CARTESIAN_POINT('Ctrl Pts',(9.58275281935204,0.14313528264739,3.42239004773181));
#38870=CARTESIAN_POINT('Ctrl Pts',(9.59865809803965,0.334348093367161,3.46977375294793));
#38871=CARTESIAN_POINT('Ctrl Pts',(9.61456337672728,0.499694809969701,3.62153782554855));
#38872=CARTESIAN_POINT('Ctrl Pts',(9.63046865541489,0.563255215433827,3.80799862400389));
#38873=CARTESIAN_POINT('Ctrl Pts',(9.6463739341025,0.626815620897955,3.99445942245922));
#38874=CARTESIAN_POINT('Ctrl Pts',(9.6622792127901,0.588589715223662,4.21561694676927));
#38875=CARTESIAN_POINT('Ctrl Pts',(9.67818449147771,0.466129217091882,4.36992501817411));
#38876=CARTESIAN_POINT('Ctrl Pts',(9.69250785723264,0.355848439261942,4.50888586187125));
#38877=CARTESIAN_POINT('Ctrl Pts',(9.70683122298757,0.177255492135987,4.59363345408847));
#38878=CARTESIAN_POINT('Ctrl Pts',(9.7211545887425,-0.000338423355870402,
4.59484023865297));
#38879=CARTESIAN_POINT('Origin',(4.,0.,4.));
#38880=CARTESIAN_POINT('',(10.1288454112576,0.000175993811045716,4.59316417414361));
#38881=CARTESIAN_POINT('',(10.0211545887425,0.000517772199431355,4.59437035498519));
#38882=CARTESIAN_POINT('',(4.,-7.27562663373442E-17,4.5941));
#38883=CARTESIAN_POINT('Ctrl Pts',(10.1288454112576,0.000175993811045716,
4.59316417414361));
#38884=CARTESIAN_POINT('Ctrl Pts',(10.1217594766001,0.0886689559287146,
4.59339827721605));
#38885=CARTESIAN_POINT('Ctrl Pts',(10.1146735419426,0.177068724884878,4.57486525982572));
#38886=CARTESIAN_POINT('Ctrl Pts',(10.1075876072851,0.256276603526552,4.53706914692868));
#38887=CARTESIAN_POINT('Ctrl Pts',(10.0916823285975,0.434068729046268,4.45223097977176));
#38888=CARTESIAN_POINT('Ctrl Pts',(10.0757770499098,0.565548899719798,4.27033860735548));
#38889=CARTESIAN_POINT('Ctrl Pts',(10.0598717712222,0.590346983641159,4.0749093118617));
#38890=CARTESIAN_POINT('Ctrl Pts',(10.0439664925346,0.61514506756252,3.87948001636793));
#38891=CARTESIAN_POINT('Ctrl Pts',(10.028061213847,0.533261064731712,3.67051379779667));
#38892=CARTESIAN_POINT('Ctrl Pts',(10.0121559351594,0.382292645022166,3.5439591030842));
#38893=CARTESIAN_POINT('Ctrl Pts',(9.99625065647179,0.231324225312614,3.41740440837173));
#38894=CARTESIAN_POINT('Ctrl Pts',(9.98034537778417,0.011271388724311,3.37326123751805));
#38895=CARTESIAN_POINT('Ctrl Pts',(9.96444009909655,-0.17682691184915,3.43179826703564));
#38896=CARTESIAN_POINT('Ctrl Pts',(9.94853482040894,-0.364925212422603,
3.49033529655323));
#38897=CARTESIAN_POINT('Ctrl Pts',(9.93262954172133,-0.521068976981223,
3.65155252644206));
#38898=CARTESIAN_POINT('Ctrl Pts',(9.91672426303372,-0.573563594737602,
3.84142582527571));
#38899=CARTESIAN_POINT('Ctrl Pts',(9.90081898434611,-0.626058212493981,
4.03129912410937));
#38900=CARTESIAN_POINT('Ctrl Pts',(9.8849137056585,-0.574903683448118,4.24982849188785));
#38901=CARTESIAN_POINT('Ctrl Pts',(9.86900842697089,-0.443588003168223,
4.39667448814241));
#38902=CARTESIAN_POINT('Ctrl Pts',(9.85562075506645,-0.333057953489513,
4.52027659892262));
#38903=CARTESIAN_POINT('Ctrl Pts',(9.842233083162,-0.165735336637852,4.59309247934331));
#38904=CARTESIAN_POINT('Ctrl Pts',(9.82884541125756,0.000474857175501747,
4.59454166667424));
#38905=CARTESIAN_POINT('Ctrl Pts',(9.7211545887425,-0.000338423355870402,
4.59484023865297));
#38906=CARTESIAN_POINT('Ctrl Pts',(9.72273650167518,-0.0199523965301825,
4.59497351934566));
#38907=CARTESIAN_POINT('Ctrl Pts',(9.72431841460787,-0.0395541838993478,
4.59408780127083));
#38908=CARTESIAN_POINT('Ctrl Pts',(9.72590032754056,-0.0590504136254521,
4.592143576127));
#38909=CARTESIAN_POINT('Ctrl Pts',(9.74180560622817,-0.255074455621757,
4.57259544417541));
#38910=CARTESIAN_POINT('Ctrl Pts',(9.75771088491579,-0.4404274490251,4.4460405617726));
#38911=CARTESIAN_POINT('Ctrl Pts',(9.7736161636034,-0.530003140903138,4.2705875768224));
#38912=CARTESIAN_POINT('Ctrl Pts',(9.78952144229101,-0.619578832781174,
4.0951345918722));
#38913=CARTESIAN_POINT('Ctrl Pts',(9.80542672097862,-0.61337722313391,3.87078350437461));
#38914=CARTESIAN_POINT('Ctrl Pts',(9.82133199966623,-0.514245828742901,
3.70054684219675));
#38915=CARTESIAN_POINT('Ctrl Pts',(9.83723727835384,-0.41511443435189,3.53031018001889));
#38916=CARTESIAN_POINT('Ctrl Pts',(9.85314255704146,-0.223053255217129,
3.41418794316076));
#38917=CARTESIAN_POINT('Ctrl Pts',(9.86904783572907,-0.0262486593588972,
3.40549855006092));
#38918=CARTESIAN_POINT('Ctrl Pts',(9.88495311441669,0.170555936499329,3.39680915696108));
#38919=CARTESIAN_POINT('Ctrl Pts',(9.9008583931043,0.372103949081026,3.49555260761951));
#38920=CARTESIAN_POINT('Ctrl Pts',(9.91676367179191,0.485853057801912,3.65639008698476));
#38921=CARTESIAN_POINT('Ctrl Pts',(9.93266895047952,0.5996021665228,3.81722756635002));
#38922=CARTESIAN_POINT('Ctrl Pts',(9.94857422916713,0.625552371382872,4.04015907442209));
#38923=CARTESIAN_POINT('Ctrl Pts',(9.96447950785475,0.551788436173011,4.22282389414861));
#38924=CARTESIAN_POINT('Ctrl Pts',(9.98038478654236,0.478024500963153,4.40548871387512));
#38925=CARTESIAN_POINT('Ctrl Pts',(9.99629006522997,0.304546425683368,4.54788684525607));
#38926=CARTESIAN_POINT('Ctrl Pts',(10.0121953439176,0.111008003250015,4.58463509072946));
#38927=CARTESIAN_POINT('Ctrl Pts',(10.0151817588592,0.0746687445744621,
4.59153503329043));
#38928=CARTESIAN_POINT('Ctrl Pts',(10.0181681738009,0.0376222632219309,
4.59471031472953));
#38929=CARTESIAN_POINT('Ctrl Pts',(10.0211545887425,0.000517772199431355,
4.59437035498519));
#38930=CARTESIAN_POINT('Origin',(4.,0.,4.));
#38931=CARTESIAN_POINT('',(10.4288454112576,-0.000541293539476018,4.59389423388278));
#38932=CARTESIAN_POINT('',(10.3211545887425,8.19078234495683E-5,4.59312629593825));
#38933=CARTESIAN_POINT('',(4.,-7.27562663373442E-17,4.5941));
#38934=CARTESIAN_POINT('Ctrl Pts',(10.4288454112576,-0.000541293539476018,
4.59389423388278));
#38935=CARTESIAN_POINT('Ctrl Pts',(10.4171911487257,0.144553461780974,4.59260897165526));
#38936=CARTESIAN_POINT('Ctrl Pts',(10.4055368861939,0.290497422953868,4.53904330389552));
#38937=CARTESIAN_POINT('Ctrl Pts',(10.3938826236621,0.397841883685798,4.4425412994096));
#38938=CARTESIAN_POINT('Ctrl Pts',(10.3779773449745,0.544341377656434,4.31083916286766));
#38939=CARTESIAN_POINT('Ctrl Pts',(10.3620720662869,0.618946539098701,4.09916502578488));
#38940=CARTESIAN_POINT('Ctrl Pts',(10.3461667875993,0.587401834162399,3.90471069671543));
#38941=CARTESIAN_POINT('Ctrl Pts',(10.3302615089117,0.555857129226098,3.710256367646));
#38942=CARTESIAN_POINT('Ctrl Pts',(10.314356230224,0.418162557911234,3.5330218465899));
#38943=CARTESIAN_POINT('Ctrl Pts',(10.2984509515364,0.237541641988682,3.45438572744188));
#38944=CARTESIAN_POINT('Ctrl Pts',(10.2825456728488,0.0569207260661262,
3.37574960829385));
#38945=CARTESIAN_POINT('Ctrl Pts',(10.2666403941612,-0.16662653446412,3.3957118910539));
#38946=CARTESIAN_POINT('Ctrl Pts',(10.2507351154736,-0.330456695071223,
3.50510674001315));
#38947=CARTESIAN_POINT('Ctrl Pts',(10.234829836786,-0.494286855678321,3.61450158897239));
#38948=CARTESIAN_POINT('Ctrl Pts',(10.2189245580984,-0.59839991636228,3.81332900413083));
#38949=CARTESIAN_POINT('Ctrl Pts',(10.2030192794108,-0.594991564317383,
4.01029584814195));
#38950=CARTESIAN_POINT('Ctrl Pts',(10.1871140007231,-0.591583212272486,
4.20726269215308));
#38951=CARTESIAN_POINT('Ctrl Pts',(10.1712087220355,-0.480653447498727,
4.40236896501689));
#38952=CARTESIAN_POINT('Ctrl Pts',(10.1553034433479,-0.313136524928893,
4.50603012050002));
#38953=CARTESIAN_POINT('Ctrl Pts',(10.1464840993178,-0.220249792163878,
4.56350936438632));
#38954=CARTESIAN_POINT('Ctrl Pts',(10.1376647552877,-0.109964716607974,
4.59287280319057));
#38955=CARTESIAN_POINT('Ctrl Pts',(10.1288454112576,0.000175993811045716,
4.59316417414361));
#38956=CARTESIAN_POINT('Ctrl Pts',(10.0211545887425,0.000517772199431355,
4.59437035498519));
#38957=CARTESIAN_POINT('Ctrl Pts',(10.0340734524885,-0.159991692577292,
4.59289973094197));
#38958=CARTESIAN_POINT('Ctrl Pts',(10.0469923162344,-0.321586704601994,
4.52564765365589));
#38959=CARTESIAN_POINT('Ctrl Pts',(10.0599111799804,-0.431712787135162,
4.40956688772629));
#38960=CARTESIAN_POINT('Ctrl Pts',(10.075816458668,-0.567296385500051,4.2666520796839));
#38961=CARTESIAN_POINT('Ctrl Pts',(10.0917217373556,-0.624864812642908,
4.04972410403331));
#38962=CARTESIAN_POINT('Ctrl Pts',(10.1076270160433,-0.577985082339038,
3.85838710972745));
#38963=CARTESIAN_POINT('Ctrl Pts',(10.1235322947309,-0.531105352035168,
3.6670501154216));
#38964=CARTESIAN_POINT('Ctrl Pts',(10.1394375734185,-0.379777464284567,
3.50130410246047));
#38965=CARTESIAN_POINT('Ctrl Pts',(10.1553428521061,-0.193484782987353,
3.43725262786029));
#38966=CARTESIAN_POINT('Ctrl Pts',(10.1712481307937,-0.00719210169012799,
3.37320115326011));
#38967=CARTESIAN_POINT('Ctrl Pts',(10.1871534094813,0.214065373153706,3.41084421702088));
#38968=CARTESIAN_POINT('Ctrl Pts',(10.2030586881689,0.368695569727689,3.53289771681035));
#38969=CARTESIAN_POINT('Ctrl Pts',(10.2189639668565,0.523325766301663,3.65495121659981));
#38970=CARTESIAN_POINT('Ctrl Pts',(10.2348692455442,0.611328684605784,3.86141515241798));
#38971=CARTESIAN_POINT('Ctrl Pts',(10.2507745242318,0.592297107651237,4.05749001970593));
#38972=CARTESIAN_POINT('Ctrl Pts',(10.2666798029194,0.573265530696689,4.25356488699388));
#38973=CARTESIAN_POINT('Ctrl Pts',(10.282585081607,0.447199458483466,4.43925068575162));
#38974=CARTESIAN_POINT('Ctrl Pts',(10.2984903602946,0.271983097956201,4.5292883529079));
#38975=CARTESIAN_POINT('Ctrl Pts',(10.3060451031106,0.188758241169316,4.57205474716445));
#38976=CARTESIAN_POINT('Ctrl Pts',(10.3135998459265,0.0944446272328244,
4.59324204311815));
#38977=CARTESIAN_POINT('Ctrl Pts',(10.3211545887425,8.19078234495684E-5,
4.59312629593825));
#38978=CARTESIAN_POINT('Origin',(4.,0.,4.));
#38979=CARTESIAN_POINT('',(10.7288454112576,7.37317986114466E-5,4.59506942345298));
#38980=CARTESIAN_POINT('',(10.6211545887425,-0.000548317120500629,4.59406879148573));
#38981=CARTESIAN_POINT('',(4.,-7.27562663373442E-17,4.5941));
#38982=CARTESIAN_POINT('Ctrl Pts',(10.7288454112576,7.37317986114466E-5,
4.59506942345298));
#38983=CARTESIAN_POINT('Ctrl Pts',(10.728528099539,0.00400402563557926,
4.59507627971693));
#38984=CARTESIAN_POINT('Ctrl Pts',(10.7282107878205,0.00793419209028873,
4.59504072157671));
#38985=CARTESIAN_POINT('Ctrl Pts',(10.727893476102,0.0118635052742893,4.59496237136513));
#38986=CARTESIAN_POINT('Ctrl Pts',(10.7119881974144,0.208820685209451,4.59103505989901));
#38987=CARTESIAN_POINT('Ctrl Pts',(10.6960829187267,0.403634001393415,4.47959161118634));
#38988=CARTESIAN_POINT('Ctrl Pts',(10.6801776400391,0.506853420906232,4.31180214209248));
#38989=CARTESIAN_POINT('Ctrl Pts',(10.6642723613515,0.610072840419052,4.14401267299861));
#38990=CARTESIAN_POINT('Ctrl Pts',(10.6483670826639,0.621698363260717,3.91987718352354));
#38991=CARTESIAN_POINT('Ctrl Pts',(10.6324618039763,0.536392041177647,3.74230920804366));
#38992=CARTESIAN_POINT('Ctrl Pts',(10.6165565252887,0.451085719094577,3.56474123256377));
#38993=CARTESIAN_POINT('Ctrl Pts',(10.6006512466011,0.26884755208677,3.43374077107907));
#38994=CARTESIAN_POINT('Ctrl Pts',(10.5847459679135,0.0733535965831807,
3.40945769333085));
#38995=CARTESIAN_POINT('Ctrl Pts',(10.5688406892258,-0.122140358920403,
3.38517461558263));
#38996=CARTESIAN_POINT('Ctrl Pts',(10.5529354105382,-0.33089010291977,3.46760892157089));
#38997=CARTESIAN_POINT('Ctrl Pts',(10.5370301318506,-0.457046584443773,
3.61891026549369));
#38998=CARTESIAN_POINT('Ctrl Pts',(10.521124853163,-0.583203065967777,3.7702116094165));
#38999=CARTESIAN_POINT('Ctrl Pts',(10.5052195744754,-0.626766285016417,
3.99037999127385));
#39000=CARTESIAN_POINT('Ctrl Pts',(10.4893142957878,-0.567733854410369,
4.17832340467295));
#39001=CARTESIAN_POINT('Ctrl Pts',(10.4734090171002,-0.508701423804317,
4.36626681807206));
#39002=CARTESIAN_POINT('Ctrl Pts',(10.4575037384126,-0.347073343543565,
4.52198526301292));
#39003=CARTESIAN_POINT('Ctrl Pts',(10.4415984597249,-0.157062390163684,
4.57397941748279));
#39004=CARTESIAN_POINT('Ctrl Pts',(10.4373474435692,-0.106278015462724,
4.58787593542499));
#39005=CARTESIAN_POINT('Ctrl Pts',(10.4330964274134,-0.0534661480554494,
4.59436304694399));
#39006=CARTESIAN_POINT('Ctrl Pts',(10.4288454112576,-0.000541293539476018,
4.59389423388278));
#39007=CARTESIAN_POINT('Ctrl Pts',(10.3211545887425,8.19078234495684E-5,
4.59312629593825));
#39008=CARTESIAN_POINT('Ctrl Pts',(10.3295051246142,-0.104220686264852,
4.59299835631127));
#39009=CARTESIAN_POINT('Ctrl Pts',(10.3378556604858,-0.208583275928277,
4.56684300569277));
#39010=CARTESIAN_POINT('Ctrl Pts',(10.3462061963575,-0.298097175589899,
4.5150330474864));
#39011=CARTESIAN_POINT('Ctrl Pts',(10.3621114750451,-0.468594439767441,
4.41635053935381));
#39012=CARTESIAN_POINT('Ctrl Pts',(10.3780167537327,-0.585222319281217,
4.22459598753381));
#39013=CARTESIAN_POINT('Ctrl Pts',(10.3939220324203,-0.594430225977177,
4.02781496975607));
#39014=CARTESIAN_POINT('Ctrl Pts',(10.4098273111079,-0.603638132673137,
3.83103395197833));
#39015=CARTESIAN_POINT('Ctrl Pts',(10.4257325897955,-0.505426066551287,
3.62922646824286));
#39016=CARTESIAN_POINT('Ctrl Pts',(10.4416378684831,-0.344888853364916,
3.51505397731042));
#39017=CARTESIAN_POINT('Ctrl Pts',(10.4575431471707,-0.184351640178541,
3.40088148637798));
#39018=CARTESIAN_POINT('Ctrl Pts',(10.4734484258584,0.0385107200723601,
3.37434398824859));
#39019=CARTESIAN_POINT('Ctrl Pts',(10.489353704546,0.221369260089487,3.4476263793543));
#39020=CARTESIAN_POINT('Ctrl Pts',(10.5052589832336,0.40422780010661,3.52090877046001));
#39021=CARTESIAN_POINT('Ctrl Pts',(10.5211642619212,0.54708251988996,3.69401105080081));
#39022=CARTESIAN_POINT('Ctrl Pts',(10.5370695406088,0.584340575799814,3.88745197659776));
#39023=CARTESIAN_POINT('Ctrl Pts',(10.5529748192964,0.621598631709669,4.08089290239472));
#39024=CARTESIAN_POINT('Ctrl Pts',(10.568880097984,0.55326002374602,4.29467247364782));
#39025=CARTESIAN_POINT('Ctrl Pts',(10.5847853766716,0.4107029495177,4.43063215550545));
#39026=CARTESIAN_POINT('Ctrl Pts',(10.5969084473619,0.302045344566967,4.53426120008624));
#39027=CARTESIAN_POINT('Ctrl Pts',(10.6090315180522,0.150270129189204,4.59268036842864));
#39028=CARTESIAN_POINT('Ctrl Pts',(10.6211545887425,-0.000548317120500629,
4.59406879148573));
#39029=CARTESIAN_POINT('Origin',(4.,0.,4.));
#39030=CARTESIAN_POINT('',(11.0288454112576,0.000503618959454472,4.59367252935801));
#39031=CARTESIAN_POINT('',(10.9211545887425,0.000179316795020235,4.59501533910171));
#39032=CARTESIAN_POINT('',(4.,-7.27562663373442E-17,4.5941));
#39033=CARTESIAN_POINT('Ctrl Pts',(11.0288454112576,0.000503618959454472,
4.59367252935801));
#39034=CARTESIAN_POINT('Ctrl Pts',(11.0239597716647,0.0613870506829751,
4.59415995979602));
#39035=CARTESIAN_POINT('Ctrl Pts',(11.0190741320719,0.122135879976345,4.58554712933309));
#39036=CARTESIAN_POINT('Ctrl Pts',(11.014188492479,0.179818659528701,4.56726203449827));
#39037=CARTESIAN_POINT('Ctrl Pts',(10.9982832137914,0.36760588100072,4.50773461262244));
#39038=CARTESIAN_POINT('Ctrl Pts',(10.9823779351038,0.52289792528528,4.34569680405454));
#39039=CARTESIAN_POINT('Ctrl Pts',(10.9664726564162,0.574391255511512,4.15554951523459));
#39040=CARTESIAN_POINT('Ctrl Pts',(10.9505673777285,0.625884585737745,3.96540222641464));
#39041=CARTESIAN_POINT('Ctrl Pts',(10.9346620990409,0.573579201905647,3.74714545734266));
#39042=CARTESIAN_POINT('Ctrl Pts',(10.9187568203533,0.441491523412615,3.60099348269406));
#39043=CARTESIAN_POINT('Ctrl Pts',(10.9028515416657,0.309403844919578,3.45484150804546));
#39044=CARTESIAN_POINT('Ctrl Pts',(10.8869462629781,0.0975338717655902,
3.38079432782024));
#39045=CARTESIAN_POINT('Ctrl Pts',(10.8710409842905,-0.0968366678563846,
3.41285127449999));
#39046=CARTESIAN_POINT('Ctrl Pts',(10.8551357056029,-0.291207207478354,
3.44490822117975));
#39047=CARTESIAN_POINT('Ctrl Pts',(10.8392304269153,-0.468078313568319,
3.58306929476445));
#39048=CARTESIAN_POINT('Ctrl Pts',(10.8233251482276,-0.546238257009186,
3.76389677537701));
#39049=CARTESIAN_POINT('Ctrl Pts',(10.80741986954,-0.624398200450053,3.94472425598957));
#39050=CARTESIAN_POINT('Ctrl Pts',(10.7915145908524,-0.603846981241821,
4.16821814362997));
#39051=CARTESIAN_POINT('Ctrl Pts',(10.7756093121648,-0.494020849794526,
4.33175950034039));
#39052=CARTESIAN_POINT('Ctrl Pts',(10.7600213451957,-0.386385759396791,
4.49203819249975));
#39053=CARTESIAN_POINT('Ctrl Pts',(10.7444333782267,-0.193002309618558,
4.59473260886404));
#39054=CARTESIAN_POINT('Ctrl Pts',(10.7288454112576,7.37317986114466E-5,
4.59506942345298));
#39055=CARTESIAN_POINT('Ctrl Pts',(10.6211545887425,-0.000548317120500629,
4.59406879148573));
#39056=CARTESIAN_POINT('Ctrl Pts',(10.6249367967398,-0.0476013079303647,
4.5945019577127));
#39057=CARTESIAN_POINT('Ctrl Pts',(10.6287190047372,-0.0945611723716044,
4.58938408097059));
#39058=CARTESIAN_POINT('Ctrl Pts',(10.6325012127345,-0.140089514783682,
4.57835619988505));
#39059=CARTESIAN_POINT('Ctrl Pts',(10.6484064914221,-0.331549364363767,
4.53198076994489));
#39060=CARTESIAN_POINT('Ctrl Pts',(10.6643117701097,-0.497693523030948,
4.38109011760241));
#39061=CARTESIAN_POINT('Ctrl Pts',(10.6802170487973,-0.562235622104956,
4.19496684675621));
#39062=CARTESIAN_POINT('Ctrl Pts',(10.6961223274849,-0.626777721178965,
4.00884357591002));
#39063=CARTESIAN_POINT('Ctrl Pts',(10.7120276061725,-0.589717760659791,
3.78748768656011));
#39064=CARTESIAN_POINT('Ctrl Pts',(10.7279328848602,-0.468072106540212,
3.63253643830059));
#39065=CARTESIAN_POINT('Ctrl Pts',(10.7438381635478,-0.346426452420629,
3.47758519004106));
#39066=CARTESIAN_POINT('Ctrl Pts',(10.7597434422354,-0.140195104700642,
3.38903858287192));
#39067=CARTESIAN_POINT('Ctrl Pts',(10.775648720923,0.0559292266755373,3.40755347270721));
#39068=CARTESIAN_POINT('Ctrl Pts',(10.7915539996106,0.252053558051711,3.4260683625425));
#39069=CARTESIAN_POINT('Ctrl Pts',(10.8074592782982,0.438070873084069,3.55164474938222));
#39070=CARTESIAN_POINT('Ctrl Pts',(10.8233645569858,0.528569890453362,3.72662326908837));
#39071=CARTESIAN_POINT('Ctrl Pts',(10.8392698356734,0.619068907822657,3.90160178879453));
#39072=CARTESIAN_POINT('Ctrl Pts',(10.8551751143611,0.614049627528876,4.12598244136713));
#39073=CARTESIAN_POINT('Ctrl Pts',(10.8710803930487,0.515816690734684,4.29673912390739));
#39074=CARTESIAN_POINT('Ctrl Pts',(10.8869856717363,0.417583753940498,4.46749580644764));
#39075=CARTESIAN_POINT('Ctrl Pts',(10.9028909504239,0.226137160645921,4.58462851895556));
#39076=CARTESIAN_POINT('Ctrl Pts',(10.9187962291115,0.0293810870543861,
4.59435487532392));
#39077=CARTESIAN_POINT('Ctrl Pts',(10.9195823489885,0.0196563998352688,
4.59483560139116));
#39078=CARTESIAN_POINT('Ctrl Pts',(10.9203684688655,0.00991874240631306,
4.5950539509358));
#39079=CARTESIAN_POINT('Ctrl Pts',(10.9211545887425,0.000179316795020235,
4.59501533910171));
#39080=CARTESIAN_POINT('Origin',(4.,0.,4.));
#39081=CARTESIAN_POINT('',(11.3288454112576,-0.000294350894641693,4.59325842069974));
#39082=CARTESIAN_POINT('',(11.2211545887425,0.000456638431143918,4.59352536526061));
#39083=CARTESIAN_POINT('',(4.,-7.27562663373442E-17,4.5941));
#39084=CARTESIAN_POINT('Ctrl Pts',(11.3288454112576,-0.000294350894641693,
4.59325842069974));
#39085=CARTESIAN_POINT('Ctrl Pts',(11.3193914437904,0.117725031793324,4.59273125875086));
#39086=CARTESIAN_POINT('Ctrl Pts',(11.3099374763232,0.236024696118704,4.55868066117597));
#39087=CARTESIAN_POINT('Ctrl Pts',(11.300483508856,0.333060002447629,4.49314500997921));
#39088=CARTESIAN_POINT('Ctrl Pts',(11.2845782301684,0.496311419914153,4.38288835848583));
#39089=CARTESIAN_POINT('Ctrl Pts',(11.2686729514808,0.599375291650127,4.18351506848348));
#39090=CARTESIAN_POINT('Ctrl Pts',(11.2527676727932,0.594929048027223,3.98656891995295));
#39091=CARTESIAN_POINT('Ctrl Pts',(11.2368623941056,0.59048280440432,3.78962277142242));
#39092=CARTESIAN_POINT('Ctrl Pts',(11.220957115418,0.478526445422532,3.5951037643637));
#39093=CARTESIAN_POINT('Ctrl Pts',(11.2050518367303,0.310465594643358,3.49232679739763));
#39094=CARTESIAN_POINT('Ctrl Pts',(11.1891465580427,0.142404743864184,3.38954983043155));
#39095=CARTESIAN_POINT('Ctrl Pts',(11.1732412793551,-0.0817605987123653,
3.37851490355812));
#39096=CARTESIAN_POINT('Ctrl Pts',(11.1573360006675,-0.259103191428711,
3.46428878834836));
#39097=CARTESIAN_POINT('Ctrl Pts',(11.1414307219799,-0.436445784145052,
3.5500626731386));
#39098=CARTESIAN_POINT('Ctrl Pts',(11.1255254432923,-0.566965627001181,
3.73264536959251));
#39099=CARTESIAN_POINT('Ctrl Pts',(11.1096201646047,-0.590733529996744,
3.92820262793532));
#39100=CARTESIAN_POINT('Ctrl Pts',(11.0937148859171,-0.614501432992307,
4.12375988627813));
#39101=CARTESIAN_POINT('Ctrl Pts',(11.0778096072294,-0.531517396127296,
4.33229170650985));
#39102=CARTESIAN_POINT('Ctrl Pts',(11.0619043285418,-0.379884178365051,
4.45804909903384));
#39103=CARTESIAN_POINT('Ctrl Pts',(11.0508846894471,-0.274828280424841,
4.54517747360242));
#39104=CARTESIAN_POINT('Ctrl Pts',(11.0398650503523,-0.136819945681758,
4.59257312212411));
#39105=CARTESIAN_POINT('Ctrl Pts',(11.0288454112576,0.000503618959454472,
4.59367252935801));
#39106=CARTESIAN_POINT('Ctrl Pts',(10.9211545887425,0.000179316795020235,
4.59501533910171));
#39107=CARTESIAN_POINT('Ctrl Pts',(10.9362737475531,-0.187135527734918,
4.59427273168419));
#39108=CARTESIAN_POINT('Ctrl Pts',(10.9513929063637,-0.375104412928531,
4.49848156101044));
#39109=CARTESIAN_POINT('Ctrl Pts',(10.9665120651743,-0.484035620954107,
4.34616539940523));
#39110=CARTESIAN_POINT('Ctrl Pts',(10.982417343862,-0.598630701482551,4.1859295668894));
#39111=CARTESIAN_POINT('Ctrl Pts',(10.9983226225496,-0.625755308650954,
3.96313790162893));
#39112=CARTESIAN_POINT('Ctrl Pts',(11.0142279012372,-0.55295497039508,3.7800869107734));
#39113=CARTESIAN_POINT('Ctrl Pts',(11.0301331799248,-0.480154632139201,
3.59703591991786));
#39114=CARTESIAN_POINT('Ctrl Pts',(11.0460384586124,-0.307429348459053,
3.45372560346725));
#39115=CARTESIAN_POINT('Ctrl Pts',(11.0619437373,-0.114087262216405,3.41595799577618));
#39116=CARTESIAN_POINT('Ctrl Pts',(11.0778490159876,0.0792548240262376,
3.37819038808511));
#39117=CARTESIAN_POINT('Ctrl Pts',(11.0937542946752,0.293213712831377,3.4459654891536));
#39118=CARTESIAN_POINT('Ctrl Pts',(11.1096595733629,0.429548534313776,3.58816383989905));
#39119=CARTESIAN_POINT('Ctrl Pts',(11.1255648520505,0.565883355796175,3.7303621906445));
#39120=CARTESIAN_POINT('Ctrl Pts',(11.1414701307381,0.624594109955846,3.94698379106692));
#39121=CARTESIAN_POINT('Ctrl Pts',(11.1573754094257,0.578723302329844,4.13856516675647));
#39122=CARTESIAN_POINT('Ctrl Pts',(11.1732806881133,0.53285249470384,4.33014654244603));
#39123=CARTESIAN_POINT('Ctrl Pts',(11.1891859668009,0.382400125292158,4.49668769340272));
#39124=CARTESIAN_POINT('Ctrl Pts',(11.2050912454885,0.196447557013804,4.56171996888228));
#39125=CARTESIAN_POINT('Ctrl Pts',(11.2104456932399,0.133847376870746,4.58361282144047));
#39126=CARTESIAN_POINT('Ctrl Pts',(11.2158001409912,0.0672239414478651,
4.5940016224088));
#39127=CARTESIAN_POINT('Ctrl Pts',(11.2211545887425,0.000456638431143918,
4.59352536526061));
#39128=CARTESIAN_POINT('Origin',(4.,0.,4.));
#39129=CARTESIAN_POINT('',(11.6288454112576,-0.000389145320547679,4.59475273347735));
#39130=CARTESIAN_POINT('',(11.5211545887425,-0.0003715675665865,4.59335763259963));
#39131=CARTESIAN_POINT('',(4.,-7.27562663373442E-17,4.5941));
#39132=CARTESIAN_POINT('Ctrl Pts',(11.6288454112576,-0.000389145320547679,
4.59475273347735));
#39133=CARTESIAN_POINT('Ctrl Pts',(11.6148231159161,0.173538999407471,4.59343557735163));
#39134=CARTESIAN_POINT('Ctrl Pts',(11.6008008205746,0.348531733704351,4.51264940831536));
#39135=CARTESIAN_POINT('Ctrl Pts',(11.586778525233,0.459048433726307,4.37867598496766));
#39136=CARTESIAN_POINT('Ctrl Pts',(11.5708732465454,0.584405864209301,4.22671194604376));
#39137=CARTESIAN_POINT('Ctrl Pts',(11.5549679678578,0.626808276394098,4.00631705984067));
#39138=CARTESIAN_POINT('Ctrl Pts',(11.5390626891702,0.566786276503563,3.81868733396413));
#39139=CARTESIAN_POINT('Ctrl Pts',(11.5231574104826,0.506764276613028,3.6310576080876));
#39140=CARTESIAN_POINT('Ctrl Pts',(11.507252131795,0.344317864647159,3.47619304253762));
#39141=CARTESIAN_POINT('Ctrl Pts',(11.4913468531074,0.154035560439752,3.4252008940353));
#39142=CARTESIAN_POINT('Ctrl Pts',(11.4754415744198,-0.0362467437676612,
3.37420874553297));
#39143=CARTESIAN_POINT('Ctrl Pts',(11.4595362957322,-0.254364940216614,
3.4270890140783));
#39144=CARTESIAN_POINT('Ctrl Pts',(11.4436310170445,-0.400168380917644,
3.55956131753494));
#39145=CARTESIAN_POINT('Ctrl Pts',(11.4277257383569,-0.545971821618673,
3.69203362099157));
#39146=CARTESIAN_POINT('Ctrl Pts',(11.4118204596693,-0.619460506571779,
3.90409795935952));
#39147=CARTESIAN_POINT('Ctrl Pts',(11.3959151809817,-0.586891540696359,
4.09838336016249));
#39148=CARTESIAN_POINT('Ctrl Pts',(11.3800099022941,-0.554322574820941,
4.29266876096545));
#39149=CARTESIAN_POINT('Ctrl Pts',(11.3641046236065,-0.415695958117004,
4.46917522420345));
#39150=CARTESIAN_POINT('Ctrl Pts',(11.3481993449189,-0.234663168166497,
4.54685844933023));
#39151=CARTESIAN_POINT('Ctrl Pts',(11.3417480336984,-0.161234786808821,
4.57836740127901));
#39152=CARTESIAN_POINT('Ctrl Pts',(11.335296722478,-0.080829826651965,4.59361815176584));
#39153=CARTESIAN_POINT('Ctrl Pts',(11.3288454112576,-0.000294350894641693,
4.59325842069974));
#39154=CARTESIAN_POINT('Ctrl Pts',(11.2211545887425,0.000456638431143918,
4.59352536526061));
#39155=CARTESIAN_POINT('Ctrl Pts',(11.2317054196788,-0.131106980996848,
4.59258691018808));
#39156=CARTESIAN_POINT('Ctrl Pts',(11.2422562506151,-0.263229208150973,
4.54946171071576));
#39157=CARTESIAN_POINT('Ctrl Pts',(11.2528070815514,-0.366229002642205,
4.4690386804108));
#39158=CARTESIAN_POINT('Ctrl Pts',(11.268712360239,-0.521500226874852,4.34780171645731));
#39159=CARTESIAN_POINT('Ctrl Pts',(11.2846176389266,-0.610589908195122,
4.1418043885479));
#39160=CARTESIAN_POINT('Ctrl Pts',(11.3005229176142,-0.592591834014348,
3.94563195463032));
#39161=CARTESIAN_POINT('Ctrl Pts',(11.3164281963018,-0.574593759833574,
3.74945952071274));
#39162=CARTESIAN_POINT('Ctrl Pts',(11.3323334749894,-0.449507930151742,
3.56311198078699));
#39163=CARTESIAN_POINT('Ctrl Pts',(11.3482387536771,-0.274768466013715,
3.47215224147272));
#39164=CARTESIAN_POINT('Ctrl Pts',(11.3641440323647,-0.100029001875688,
3.38119250215845));
#39165=CARTESIAN_POINT('Ctrl Pts',(11.3800493110523,0.12436409671854,3.38562056345565));
#39166=CARTESIAN_POINT('Ctrl Pts',(11.3959545897399,0.295379012183608,3.48340324695247));
#39167=CARTESIAN_POINT('Ctrl Pts',(11.4118598684275,0.466393927648671,3.5811859304493));
#39168=CARTESIAN_POINT('Ctrl Pts',(11.4277651471151,0.584030659984583,3.77232323614575));
#39169=CARTESIAN_POINT('Ctrl Pts',(11.4436704258027,0.594275398502411,3.96905299961855));
#39170=CARTESIAN_POINT('Ctrl Pts',(11.4595757044903,0.60452013702024,4.16578276309136));
#39171=CARTESIAN_POINT('Ctrl Pts',(11.475480983178,0.507372881719984,4.36810498434052));
#39172=CARTESIAN_POINT('Ctrl Pts',(11.4913862618656,0.34743954227408,4.48312185891572));
#39173=CARTESIAN_POINT('Ctrl Pts',(11.5013090374912,0.247662438486696,4.55487707062799));
#39174=CARTESIAN_POINT('Ctrl Pts',(11.5112318131169,0.123448374926332,4.59265218509947));
#39175=CARTESIAN_POINT('Ctrl Pts',(11.5211545887425,-0.0003715675665865,
4.59335763259963));
#39176=CARTESIAN_POINT('Origin',(4.,0.,4.));
#39177=CARTESIAN_POINT('',(11.9288454112576,0.000492284285450728,4.5944814532616));
#39178=CARTESIAN_POINT('',(11.8211545887425,-0.000307672146732893,4.59488449882539));
#39179=CARTESIAN_POINT('',(4.,-7.27562663373442E-17,4.5941));
#39180=CARTESIAN_POINT('Ctrl Pts',(11.9288454112576,0.000492284285450728,
4.5944814532616));
#39181=CARTESIAN_POINT('Ctrl Pts',(11.9261600667293,0.0338400408399785,
4.59477876231094));
#39182=CARTESIAN_POINT('Ctrl Pts',(11.9234747222011,0.0671420792079604,
4.59221542322669));
#39183=CARTESIAN_POINT('Ctrl Pts',(11.9207893776729,0.0999293694653808,
4.5866302815369));
#39184=CARTESIAN_POINT('Ctrl Pts',(11.9048840989853,0.294128282668868,4.55354952256816));
#39185=CARTESIAN_POINT('Ctrl Pts',(11.8889788202977,0.470268877700486,4.41445832512751));
#39186=CARTESIAN_POINT('Ctrl Pts',(11.8730735416101,0.547474845215755,4.2332214826164));
#39187=CARTESIAN_POINT('Ctrl Pts',(11.8571682629225,0.624680812731027,4.05198464010529));
#39188=CARTESIAN_POINT('Ctrl Pts',(11.8412629842349,0.602952152729945,3.82860215252373));
#39189=CARTESIAN_POINT('Ctrl Pts',(11.8253577055472,0.492265746621211,3.66564180763548));
#39190=CARTESIAN_POINT('Ctrl Pts',(11.8094524268596,0.38157934051248,3.50268146274723));
#39191=CARTESIAN_POINT('Ctrl Pts',(11.793547148172,0.181935188296101,3.40014326055229));
#39192=CARTESIAN_POINT('Ctrl Pts',(11.7776418694844,-0.0149985615777061,
3.40510840546499));
#39193=CARTESIAN_POINT('Ctrl Pts',(11.7617365907968,-0.211932311451519,
3.41007355037768));
#39194=CARTESIAN_POINT('Ctrl Pts',(11.7458313121092,-0.406155658982761,
3.52254204239802));
#39195=CARTESIAN_POINT('Ctrl Pts',(11.7299260334216,-0.508489459897291,
3.69087310813977));
#39196=CARTESIAN_POINT('Ctrl Pts',(11.714020754734,-0.610823260811815,3.8592041738815));
#39197=CARTESIAN_POINT('Ctrl Pts',(11.6981154760463,-0.621267515109637,
4.08339781334463));
#39198=CARTESIAN_POINT('Ctrl Pts',(11.6822101973587,-0.53502666307716,4.26051379213839));
#39199=CARTESIAN_POINT('Ctrl Pts',(11.6663049186711,-0.448785811044678,
4.43762977093217));
#39200=CARTESIAN_POINT('Ctrl Pts',(11.6503996399835,-0.265859852681883,
4.56766808905658));
#39201=CARTESIAN_POINT('Ctrl Pts',(11.6344943612959,-0.070240649109886,
4.59092065229643));
#39202=CARTESIAN_POINT('Ctrl Pts',(11.6326113779498,-0.0470818155087989,
4.59367346098309));
#39203=CARTESIAN_POINT('Ctrl Pts',(11.6307283946037,-0.0237450789937817,
4.59492960773286));
#39204=CARTESIAN_POINT('Ctrl Pts',(11.6288454112576,-0.000389145320547679,
4.59475273347735));
#39205=CARTESIAN_POINT('Ctrl Pts',(11.5211545887425,-0.0003715675665865,
4.59335763259963));
#39206=CARTESIAN_POINT('Ctrl Pts',(11.5271370918045,-0.0750233800274846,
4.5937829512795));
#39207=CARTESIAN_POINT('Ctrl Pts',(11.5331195948664,-0.149531931096223,
4.58073359799715));
#39208=CARTESIAN_POINT('Ctrl Pts',(11.5391020979284,-0.218455391669058,
4.55353248138526));
#39209=CARTESIAN_POINT('Ctrl Pts',(11.555007376616,-0.40169756257477,4.48121470137836));
#39210=CARTESIAN_POINT('Ctrl Pts',(11.5709126553036,-0.545462480794654,
4.3088676134633));
#39211=CARTESIAN_POINT('Ctrl Pts',(11.5868179339912,-0.583739378074245,
4.1156257090067));
#39212=CARTESIAN_POINT('Ctrl Pts',(11.6027232126789,-0.622016275353834,
3.92238380455011));
#39213=CARTESIAN_POINT('Ctrl Pts',(11.6186284913665,-0.554805151693135,
3.70824708355197));
#39214=CARTESIAN_POINT('Ctrl Pts',(11.6345337700541,-0.412966511608993,
3.57153806891708));
#39215=CARTESIAN_POINT('Ctrl Pts',(11.6504390487417,-0.271127871524847,
3.43482905428217));
#39216=CARTESIAN_POINT('Ctrl Pts',(11.6663443274293,-0.0546617150172531,
3.37554774601052));
#39217=CARTESIAN_POINT('Ctrl Pts',(11.6822496061169,0.137039856773353,3.42091361287512));
#39218=CARTESIAN_POINT('Ctrl Pts',(11.6981548848045,0.328741428563947,3.46627947973972));
#39219=CARTESIAN_POINT('Ctrl Pts',(11.7140601634921,0.495678415637556,3.61629252174057));
#39220=CARTESIAN_POINT('Ctrl Pts',(11.7299654421798,0.56120041605148,3.80207309651931));
#39221=CARTESIAN_POINT('Ctrl Pts',(11.7458707208674,0.626722416465409,3.98785367129807));
#39222=CARTESIAN_POINT('Ctrl Pts',(11.761775999555,0.590829430219633,4.20940177885472));
#39223=CARTESIAN_POINT('Ctrl Pts',(11.7776812782426,0.470001998091193,4.36499190112672));
#39224=CARTESIAN_POINT('Ctrl Pts',(11.7921723817426,0.359917612963646,4.5067481450567));
#39225=CARTESIAN_POINT('Ctrl Pts',(11.8066634852425,0.179330777996457,4.59375393408315));
#39226=CARTESIAN_POINT('Ctrl Pts',(11.8211545887425,-0.000307672146732893,
4.59488449882539));
#39227=CARTESIAN_POINT('Origin',(4.,0.,4.));
#39228=CARTESIAN_POINT('',(12.2288454112576,0.000142795628640946,4.59314744373127));
#39229=CARTESIAN_POINT('',(12.1211545887425,0.00052868291625318,4.59430727435519));
#39230=CARTESIAN_POINT('',(4.,-7.27562663373442E-17,4.5941));
#39231=CARTESIAN_POINT('Ctrl Pts',(12.2288454112576,0.000142795628640946,
4.59314744373127));
#39232=CARTESIAN_POINT('Ctrl Pts',(12.221591738855,0.0907369315914116,4.59334157666405));
#39233=CARTESIAN_POINT('Ctrl Pts',(12.2143380664525,0.181251971066953,4.57388161006077));
#39234=CARTESIAN_POINT('Ctrl Pts',(12.2070843940499,0.261922584292681,4.53433840020651));
#39235=CARTESIAN_POINT('Ctrl Pts',(12.1911791153623,0.438810719578057,4.44763117963851));
#39236=CARTESIAN_POINT('Ctrl Pts',(12.1752738366747,0.56836661021043,4.26436322928705));
#39237=CARTESIAN_POINT('Ctrl Pts',(12.1593685579871,0.591103672269137,4.06868343852597));
#39238=CARTESIAN_POINT('Ctrl Pts',(12.1434632792995,0.613840734327844,3.87300364776488));
#39239=CARTESIAN_POINT('Ctrl Pts',(12.1275580006119,0.529758967812885,3.66491201659415));
#39240=CARTESIAN_POINT('Ctrl Pts',(12.1116527219243,0.377465162701742,3.53995541841648));
#39241=CARTESIAN_POINT('Ctrl Pts',(12.0957474432367,0.225171357590603,3.41499882023882));
#39242=CARTESIAN_POINT('Ctrl Pts',(12.0798421645491,0.00466551388328543,
3.37317725505421));
#39243=CARTESIAN_POINT('Ctrl Pts',(12.0639368858614,-0.182805413822737,
3.43369341627091));
#39244=CARTESIAN_POINT('Ctrl Pts',(12.0480316071738,-0.37027634152876,3.49420957748762));
#39245=CARTESIAN_POINT('Ctrl Pts',(12.0321263284862,-0.524712353233489,
3.65706346510565));
#39246=CARTESIAN_POINT('Ctrl Pts',(12.0162210497986,-0.575202966010955,
3.84747946371059));
#39247=CARTESIAN_POINT('Ctrl Pts',(12.000315771111,-0.625693578788423,4.03789546231555));
#39248=CARTESIAN_POINT('Ctrl Pts',(11.9844104924234,-0.572238792638624,
4.25587357190742));
#39249=CARTESIAN_POINT('Ctrl Pts',(11.9685052137358,-0.439382783876041,
4.40132746645495));
#39250=CARTESIAN_POINT('Ctrl Pts',(11.9552852795764,-0.328957325572706,
4.52222386487166));
#39251=CARTESIAN_POINT('Ctrl Pts',(11.942065345417,-0.163678510702966,4.59301780268865));
#39252=CARTESIAN_POINT('Ctrl Pts',(11.9288454112576,0.000492284285450728,
4.5944814532616));
#39253=CARTESIAN_POINT('Ctrl Pts',(11.8211545887425,-0.000307672146732893,
4.59488449882539));
#39254=CARTESIAN_POINT('Ctrl Pts',(11.8225687639301,-0.0178384446610953,
4.59499482973335));
#39255=CARTESIAN_POINT('Ctrl Pts',(11.8239829391178,-0.035360185088601,
4.59428731490513));
#39256=CARTESIAN_POINT('Ctrl Pts',(11.8253971143054,-0.0528064866265509,
4.59273302680715));
#39257=CARTESIAN_POINT('Ctrl Pts',(11.8413023929931,-0.249025661204777,
4.57525189322826));
#39258=CARTESIAN_POINT('Ctrl Pts',(11.8572076716807,-0.435702132350142,
4.45065748908313));
#39259=CARTESIAN_POINT('Ctrl Pts',(11.8731129503683,-0.527121962142897,
4.27615829360067));
#39260=CARTESIAN_POINT('Ctrl Pts',(11.8890182290559,-0.618541791935657,
4.10165909811819));
#39261=CARTESIAN_POINT('Ctrl Pts',(11.9049235077435,-0.614704980375792,
3.87725511129838));
#39262=CARTESIAN_POINT('Ctrl Pts',(11.9208287864311,-0.517373229009482,
3.70598315013913));
#39263=CARTESIAN_POINT('Ctrl Pts',(11.9367340651187,-0.420041477643178,
3.53471118897989));
#39264=CARTESIAN_POINT('Ctrl Pts',(11.9526393438063,-0.229214786470442,
3.41657125348121));
#39265=CARTESIAN_POINT('Ctrl Pts',(11.9685446224939,-0.0325126988662629,
3.4058082039356));
#39266=CARTESIAN_POINT('Ctrl Pts',(11.9844499011816,0.164189388737916,3.39504515438998));
#39267=CARTESIAN_POINT('Ctrl Pts',(12.0003551798692,0.366766872773537,3.49165899079743));
#39268=CARTESIAN_POINT('Ctrl Pts',(12.0162604585568,0.482204742918021,3.65128872687397));
#39269=CARTESIAN_POINT('Ctrl Pts',(12.0321657372444,0.597642613062508,3.81091846295053));
#39270=CARTESIAN_POINT('Ctrl Pts',(12.048071015932,0.625940869315854,4.03356409869619));
#39271=CARTESIAN_POINT('Ctrl Pts',(12.0639762946196,0.554106149607013,4.21699617753661));
#39272=CARTESIAN_POINT('Ctrl Pts',(12.0798815733072,0.482271429898174,4.40042825637702));
#39273=CARTESIAN_POINT('Ctrl Pts',(12.0957868519948,0.310303734227154,4.5446467783122));
#39274=CARTESIAN_POINT('Ctrl Pts',(12.1116921306825,0.117163353092859,4.583432699452));
#39275=CARTESIAN_POINT('Ctrl Pts',(12.1148462833691,0.0788619649798074,
4.59112427906975));
#39276=CARTESIAN_POINT('Ctrl Pts',(12.1180004360558,0.0397279339241207,
4.59466958677844));
#39277=CARTESIAN_POINT('Ctrl Pts',(12.1211545887425,0.00052868291625318,
4.59430727435519));
#39278=CARTESIAN_POINT('Origin',(4.,0.,4.));
#39279=CARTESIAN_POINT('',(12.5288454112576,-0.000545899910317726,4.59395595168017));
#39280=CARTESIAN_POINT('',(12.4211545887425,4.74932194801069E-5,4.59311952367199));
#39281=CARTESIAN_POINT('',(4.,-7.27562663373442E-17,4.5941));
#39282=CARTESIAN_POINT('Ctrl Pts',(12.5288454112576,-0.000545899910317726,
4.59395595168017));
#39283=CARTESIAN_POINT('Ctrl Pts',(12.5170234109807,0.14659828900878,4.5926299020853));
#39284=CARTESIAN_POINT('Ctrl Pts',(12.5052014107038,0.29463204299547,4.53735693360054));
#39285=CARTESIAN_POINT('Ctrl Pts',(12.493379410427,0.402483765871145,4.43832383497591));
#39286=CARTESIAN_POINT('Ctrl Pts',(12.4774741317394,0.547587104485886,4.30508504322883));
#39287=CARTESIAN_POINT('Ctrl Pts',(12.4615688530518,0.619957272242066,4.09263639239171));
#39288=CARTESIAN_POINT('Ctrl Pts',(12.4456635743641,0.586364949835353,3.89852531496775));
#39289=CARTESIAN_POINT('Ctrl Pts',(12.4297582956765,0.55277262742864,3.7044142375438));
#39290=CARTESIAN_POINT('Ctrl Pts',(12.4138530169889,0.41321781485904,3.52864073353302));
#39291=CARTESIAN_POINT('Ctrl Pts',(12.3979477383013,0.231778177981285,3.45191255961345));
#39292=CARTESIAN_POINT('Ctrl Pts',(12.3820424596137,0.0503385411035255,
3.37518438569388));
#39293=CARTESIAN_POINT('Ctrl Pts',(12.3661371809261,-0.172985920082391,
3.39750154186552));
#39294=CARTESIAN_POINT('Ctrl Pts',(12.3502319022385,-0.335654061078685,
3.50861693417539));
#39295=CARTESIAN_POINT('Ctrl Pts',(12.3343266235509,-0.498322202074975,
3.61973232648525));
#39296=CARTESIAN_POINT('Ctrl Pts',(12.3184213448632,-0.600334022881645,
3.81964595493332));
#39297=CARTESIAN_POINT('Ctrl Pts',(12.3025160661756,-0.594850011148503,
4.0165659389844));
#39298=CARTESIAN_POINT('Ctrl Pts',(12.286610787488,-0.58936599941536,4.21348592303547));
#39299=CARTESIAN_POINT('Ctrl Pts',(12.2707055088004,-0.476386155142398,
4.40741226268955));
#39300=CARTESIAN_POINT('Ctrl Pts',(12.2548002301128,-0.307786043036728,
4.50930218712431));
#39301=CARTESIAN_POINT('Ctrl Pts',(12.2461486238277,-0.216076754679914,
4.564724762732));
#39302=CARTESIAN_POINT('Ctrl Pts',(12.2374970175426,-0.107910718865932,
4.59291589733543));
#39303=CARTESIAN_POINT('Ctrl Pts',(12.2288454112576,0.000142795628640946,
4.59314744373127));
#39304=CARTESIAN_POINT('Ctrl Pts',(12.1211545887425,0.00052868291625318,
4.59430727435519));
#39305=CARTESIAN_POINT('Ctrl Pts',(12.1339057147434,-0.157940052872902,
4.59284257311225));
#39306=CARTESIAN_POINT('Ctrl Pts',(12.1466568407444,-0.317474678016714,
4.52751565545538));
#39307=CARTESIAN_POINT('Ctrl Pts',(12.1594079667453,-0.427372353356377,
4.41409399619463));
#39308=CARTESIAN_POINT('Ctrl Pts',(12.1753132454329,-0.564454612073754,
4.27261605145303));
#39309=CARTESIAN_POINT('Ctrl Pts',(12.1912185241205,-0.62430606291093,4.0563068416254));
#39310=CARTESIAN_POINT('Ctrl Pts',(12.2071238028081,-0.579445451749542,
3.8644864045766));
#39311=CARTESIAN_POINT('Ctrl Pts',(12.2230290814957,-0.534584840588155,
3.6726659675278));
#39312=CARTESIAN_POINT('Ctrl Pts',(12.2389343601834,-0.38501216742821,3.50533430325784));
#39313=CARTESIAN_POINT('Ctrl Pts',(12.254839638871,-0.199404875886796,3.43932303278057));
#39314=CARTESIAN_POINT('Ctrl Pts',(12.2707449175586,-0.0137975843453769,
3.37331176230329));
#39315=CARTESIAN_POINT('Ctrl Pts',(12.2866501962462,0.207844325577514,3.40862088561871));
#39316=CARTESIAN_POINT('Ctrl Pts',(12.3025554749338,0.363752265741203,3.52903794710619));
#39317=CARTESIAN_POINT('Ctrl Pts',(12.3184607536214,0.519660205904889,3.64945500859368));
#39318=CARTESIAN_POINT('Ctrl Pts',(12.334366032309,0.609834176309377,3.85498000825323));
#39319=CARTESIAN_POINT('Ctrl Pts',(12.3502713109967,0.592870104691008,4.05124456128685));
#39320=CARTESIAN_POINT('Ctrl Pts',(12.3661765896843,0.575906033072638,4.24750911432049));
#39321=CARTESIAN_POINT('Ctrl Pts',(12.3820818683719,0.451803919431404,4.4345132207282));
#39322=CARTESIAN_POINT('Ctrl Pts',(12.3979871470595,0.277546204023914,4.52639250633888));
#39323=CARTESIAN_POINT('Ctrl Pts',(12.4057096276205,0.192938958450368,4.57100260157974));
#39324=CARTESIAN_POINT('Ctrl Pts',(12.4134321081815,0.0965080911524262,
4.59318808505049));
#39325=CARTESIAN_POINT('Ctrl Pts',(12.4211545887425,4.74932194801069E-5,
4.59311952367199));
#39326=CARTESIAN_POINT('Origin',(4.,0.,4.));
#39327=CARTESIAN_POINT('',(12.8288454112576,0.000112157221815526,4.59505491513413));
#39328=CARTESIAN_POINT('',(12.7211545887425,-0.000546355209092884,4.59413239245978));
#39329=CARTESIAN_POINT('',(4.,-7.27562663373442E-17,4.5941));
#39330=CARTESIAN_POINT('Ctrl Pts',(12.8288454112576,0.000112157221815526,
4.59505491513413));
#39331=CARTESIAN_POINT('Ctrl Pts',(12.828360361794,0.00612048155630211,
4.59507046002904));
#39332=CARTESIAN_POINT('Ctrl Pts',(12.8278753123304,0.0121283652366354,
4.59498736156652));
#39333=CARTESIAN_POINT('Ctrl Pts',(12.8273902628668,0.0181332013859869,
4.59480429815638));
#39334=CARTESIAN_POINT('Ctrl Pts',(12.8114849841792,0.215038052543873,4.58880145767424));
#39335=CARTESIAN_POINT('Ctrl Pts',(12.7955797054916,0.408666038032992,4.47531104548453));
#39336=CARTESIAN_POINT('Ctrl Pts',(12.779674426804,0.510111378641258,4.30644305748136));
#39337=CARTESIAN_POINT('Ctrl Pts',(12.7637691481164,0.611556719249521,4.1375750694782));
#39338=CARTESIAN_POINT('Ctrl Pts',(12.7478638694288,0.620819414976937,3.9133295056616));
#39339=CARTESIAN_POINT('Ctrl Pts',(12.7319585907412,0.533646427817818,3.7366704418887));
#39340=CARTESIAN_POINT('Ctrl Pts',(12.7160533120536,0.446473440658691,3.56001137811579));
#39341=CARTESIAN_POINT('Ctrl Pts',(12.700148033366,0.26286477061301,3.43093881438659));
#39342=CARTESIAN_POINT('Ctrl Pts',(12.6842427546783,0.0671257511235207,
3.4087174113557));
#39343=CARTESIAN_POINT('Ctrl Pts',(12.6683374759907,-0.128613268365957,
3.38649600832481));
#39344=CARTESIAN_POINT('Ctrl Pts',(12.6524321973031,-0.336482637299241,
3.47112576599221));
#39345=CARTESIAN_POINT('Ctrl Pts',(12.6365269186155,-0.461037535689932,
3.62374828002683));
#39346=CARTESIAN_POINT('Ctrl Pts',(12.6206216399279,-0.585592434080627,
3.77637079406146));
#39347=CARTESIAN_POINT('Ctrl Pts',(12.6047163612403,-0.626832861928724,
3.9969860644633));
#39348=CARTESIAN_POINT('Ctrl Pts',(12.5888110825527,-0.565822959504995,
4.18429689252621));
#39349=CARTESIAN_POINT('Ctrl Pts',(12.5729058038651,-0.504813057081268,
4.37160772058911));
#39350=CARTESIAN_POINT('Ctrl Pts',(12.5570005251774,-0.341552824385721,
4.52561410631309));
#39351=CARTESIAN_POINT('Ctrl Pts',(12.5410952464898,-0.151004453301302,
4.57560283284656));
#39352=CARTESIAN_POINT('Ctrl Pts',(12.5370119680791,-0.102085973774189,
4.58843617527608));
#39353=CARTESIAN_POINT('Ctrl Pts',(12.5329286896683,-0.0513689988622793,
4.59441396466913));
#39354=CARTESIAN_POINT('Ctrl Pts',(12.5288454112576,-0.000545899910317726,
4.59395595168017));
#39355=CARTESIAN_POINT('Ctrl Pts',(12.4211545887425,4.74932194801069E-5,
4.59311952367199));
#39356=CARTESIAN_POINT('Ctrl Pts',(12.4293373868691,-0.102162877376194,
4.59304687552285));
#39357=CARTESIAN_POINT('Ctrl Pts',(12.4375201849957,-0.204406628577491,
4.5679880979308));
#39358=CARTESIAN_POINT('Ctrl Pts',(12.4457029831223,-0.292652646395614,
4.51814611323009));
#39359=CARTESIAN_POINT('Ctrl Pts',(12.4616082618099,-0.46418046423393,4.42126596969699));
#39360=CARTESIAN_POINT('Ctrl Pts',(12.4775135404976,-0.582822782736806,
4.23075121781716));
#39361=CARTESIAN_POINT('Ctrl Pts',(12.4934188191852,-0.594104068590283,
4.03407817163935));
#39362=CARTESIAN_POINT('Ctrl Pts',(12.5093240978728,-0.605385354443759,
3.83740512546155));
#39363=CARTESIAN_POINT('Ctrl Pts',(12.5252293765604,-0.509305607647849,
3.63457378498577));
#39364=CARTESIAN_POINT('Ctrl Pts',(12.541134655248,-0.34998058313236,3.51871572067214));
#39365=CARTESIAN_POINT('Ctrl Pts',(12.5570399339356,-0.19065555861687,3.4028576563585));
#39366=CARTESIAN_POINT('Ctrl Pts',(12.5729452126232,0.031914743618199,3.37397286820701));
#39367=CARTESIAN_POINT('Ctrl Pts',(12.5888504913108,0.215535456959467,3.44532402892222));
#39368=CARTESIAN_POINT('Ctrl Pts',(12.6047557699985,0.399156170300736,3.51667518963742));
#39369=CARTESIAN_POINT('Ctrl Pts',(12.6206610486861,0.543827294748204,3.68826229921932));
#39370=CARTESIAN_POINT('Ctrl Pts',(12.6365663273737,0.583121970486127,3.88129981619987));
#39371=CARTESIAN_POINT('Ctrl Pts',(12.6524716060613,0.622416646224052,4.07433733318042));
#39372=CARTESIAN_POINT('Ctrl Pts',(12.6683768847489,0.556334873252426,4.28882525755962));
#39373=CARTESIAN_POINT('Ctrl Pts',(12.6842821634365,0.415218606030559,4.42627980869829));
#39374=CARTESIAN_POINT('Ctrl Pts',(12.6965729718718,0.306170972122536,4.53249785050629));
#39375=CARTESIAN_POINT('Ctrl Pts',(12.7088637803072,0.152317016475741,4.59271595401221));
#39376=CARTESIAN_POINT('Ctrl Pts',(12.7211545887425,-0.000546355209092884,
4.59413239245978));
#39377=CARTESIAN_POINT('Origin',(4.,0.,4.));
#39378=CARTESIAN_POINT('',(13.1288454112576,0.000488576923893258,4.59361798633976));
#39379=CARTESIAN_POINT('',(13.0211545887425,0.000215375668158819,4.59498635240753));
#39380=CARTESIAN_POINT('',(4.,-7.27562663373442E-17,4.5941));
#39381=CARTESIAN_POINT('Ctrl Pts',(13.1288454112576,0.000488576923893258,
4.59361798633976));
#39382=CARTESIAN_POINT('Ctrl Pts',(13.1237920339197,0.0634769139372694,
4.59410397103046));
#39383=CARTESIAN_POINT('Ctrl Pts',(13.1187386565818,0.126326538027094,4.58487602541266));
#39384=CARTESIAN_POINT('Ctrl Pts',(13.1136852792439,0.185787091792062,4.56533540718874));
#39385=CARTESIAN_POINT('Ctrl Pts',(13.0977800005563,0.372936519850693,4.50383218710482));
#39386=CARTESIAN_POINT('Ctrl Pts',(13.0818747218686,0.526512210440984,4.34016674272733));
#39387=CARTESIAN_POINT('Ctrl Pts',(13.065969443181,0.575998703695535,4.14948732200047));
#39388=CARTESIAN_POINT('Ctrl Pts',(13.0500641644934,0.625485196950086,3.9588079012736));
#39389=CARTESIAN_POINT('Ctrl Pts',(13.0341588858058,0.570882492868891,3.74111450419737));
#39390=CARTESIAN_POINT('Ctrl Pts',(13.0182536071182,0.437261843116128,3.59636272886105));
#39391=CARTESIAN_POINT('Ctrl Pts',(13.0023483284306,0.303641193363369,3.45161095352474));
#39392=CARTESIAN_POINT('Ctrl Pts',(12.986443049743,0.0910025979390456,3.37980079992835));
#39393=CARTESIAN_POINT('Ctrl Pts',(12.9705377710554,-0.10301929613509,3.41390445256627));
#39394=CARTESIAN_POINT('Ctrl Pts',(12.9546324923678,-0.297041190209231,
3.4480081052042));
#39395=CARTESIAN_POINT('Ctrl Pts',(12.9387272136801,-0.472446382933184,
3.58802556407645));
#39396=CARTESIAN_POINT('Ctrl Pts',(12.9228219349925,-0.54869623058984,3.76966673571907));
#39397=CARTESIAN_POINT('Ctrl Pts',(12.9069166563049,-0.624946078246494,
3.95130790736168));
#39398=CARTESIAN_POINT('Ctrl Pts',(12.8910113776173,-0.602040580835857,
4.17457279177466));
#39399=CARTESIAN_POINT('Ctrl Pts',(12.8751060989297,-0.490496973717212,
4.33694759959386));
#39400=CARTESIAN_POINT('Ctrl Pts',(12.8596858697056,-0.382355015061345,
4.49437060399126));
#39401=CARTESIAN_POINT('Ctrl Pts',(12.8442656404816,-0.190898750836606,
4.59456072668396));
#39402=CARTESIAN_POINT('Ctrl Pts',(12.8288454112576,0.000112157221815526,
4.59505491513413));
#39403=CARTESIAN_POINT('Ctrl Pts',(12.7211545887425,-0.000546355209092884,
4.59413239245978));
#39404=CARTESIAN_POINT('Ctrl Pts',(12.7247690589948,-0.0455002825709059,
4.59454893744622));
#39405=CARTESIAN_POINT('Ctrl Pts',(12.7283835292471,-0.0903685417208244,
4.58988016539195));
#39406=CARTESIAN_POINT('Ctrl Pts',(12.7319979994994,-0.13398639330236,4.5798004937111));
#39407=CARTESIAN_POINT('Ctrl Pts',(12.747903278187,-0.325924363941296,4.53544544968711));
#39408=CARTESIAN_POINT('Ctrl Pts',(12.7638085568746,-0.493649543747071,
4.38631418374101));
#39409=CARTESIAN_POINT('Ctrl Pts',(12.7797138355622,-0.560149626020051,
4.20088146397168));
#39410=CARTESIAN_POINT('Ctrl Pts',(12.7956191142498,-0.626649708293032,
4.01544874420235));
#39411=CARTESIAN_POINT('Ctrl Pts',(12.8115243929374,-0.591924693033219,
3.79371457060979));
#39412=CARTESIAN_POINT('Ctrl Pts',(12.827429671625,-0.471918838153678,3.63748989490844));
#39413=CARTESIAN_POINT('Ctrl Pts',(12.8433349503126,-0.351912983274129,
3.48126521920708));
#39414=CARTESIAN_POINT('Ctrl Pts',(12.8592402290002,-0.146626288774854,
3.39055004139693));
#39415=CARTESIAN_POINT('Ctrl Pts',(12.8751455076879,0.0496822801939141,
3.40699693328572));
#39416=CARTESIAN_POINT('Ctrl Pts',(12.8910507863755,0.245990849162665,3.42344382517451));
#39417=CARTESIAN_POINT('Ctrl Pts',(12.9069560650631,0.433321292600904,3.54705278676224));
#39418=CARTESIAN_POINT('Ctrl Pts',(12.9228613437507,0.525659396179275,3.72106781235173));
#39419=CARTESIAN_POINT('Ctrl Pts',(12.9387666224383,0.617997499757654,3.89508283794124));
#39420=CARTESIAN_POINT('Ctrl Pts',(12.9546719011259,0.615343263476151,4.11950392753251));
#39421=CARTESIAN_POINT('Ctrl Pts',(12.9705771798135,0.518915400343756,4.29128641125856));
#39422=CARTESIAN_POINT('Ctrl Pts',(12.9864824585012,0.422487537211366,4.46306889498459));
#39423=CARTESIAN_POINT('Ctrl Pts',(13.0023877371888,0.232286047228094,4.58221277284539));
#39424=CARTESIAN_POINT('Ctrl Pts',(13.0182930158764,0.0356434078328121,
4.59401221668908));
#39425=CARTESIAN_POINT('Ctrl Pts',(13.0192468734984,0.0238505254767134,
4.59471984273368));
#39426=CARTESIAN_POINT('Ctrl Pts',(13.0202007311205,0.0120344772878951,
4.59504140054066));
#39427=CARTESIAN_POINT('Ctrl Pts',(13.0211545887425,0.000215375668158819,
4.59498635240753));
#39428=CARTESIAN_POINT('Origin',(4.,0.,4.));
#39429=CARTESIAN_POINT('',(13.4288454112576,-0.000323145728561625,4.59329116515504));
#39430=CARTESIAN_POINT('',(13.3211545887425,0.000436239896754628,4.59347700091179));
#39431=CARTESIAN_POINT('',(4.,-7.27562663373442E-17,4.5941));
#39432=CARTESIAN_POINT('Ctrl Pts',(13.4288454112576,-0.000323145728561625,
4.59329116515504));
#39433=CARTESIAN_POINT('Ctrl Pts',(13.4192237060453,0.11977362227264,4.59270025156928));
#39434=CARTESIAN_POINT('Ctrl Pts',(13.4096020008331,0.240190260834984,4.55734300206483));
#39435=CARTESIAN_POINT('Ctrl Pts',(13.3999802956209,0.338238798929947,4.48960747645051));
#39436=CARTESIAN_POINT('Ctrl Pts',(13.3840750169333,0.500319146323361,4.37763642888821));
#39437=CARTESIAN_POINT('Ctrl Pts',(13.3681697382457,0.601276083433826,4.17718801339723));
#39438=CARTESIAN_POINT('Ctrl Pts',(13.3522644595581,0.594754455875995,3.9802996620979));
#39439=CARTESIAN_POINT('Ctrl Pts',(13.3363591808704,0.588232828318166,3.78341131079859));
#39440=CARTESIAN_POINT('Ctrl Pts',(13.3204539021828,0.474232636092054,3.59008302369095));
#39441=CARTESIAN_POINT('Ctrl Pts',(13.3045486234952,0.305097944517489,3.48908297116948));
#39442=CARTESIAN_POINT('Ctrl Pts',(13.2886433448076,0.135963252942929,3.388082918648));
#39443=CARTESIAN_POINT('Ctrl Pts',(13.27273806612,-0.0883059379800925,3.3794111007127));
#39444=CARTESIAN_POINT('Ctrl Pts',(13.2568327874324,-0.264734703826722,
3.46704924928509));
#39445=CARTESIAN_POINT('Ctrl Pts',(13.2409275087448,-0.441163469673367,
3.55468739785749));
#39446=CARTESIAN_POINT('Ctrl Pts',(13.2250222300572,-0.569751810443623,
3.7386355129376));
#39447=CARTESIAN_POINT('Ctrl Pts',(13.2091169513696,-0.591457400179852,
3.9344324022836));
#39448=CARTESIAN_POINT('Ctrl Pts',(13.1932116726819,-0.613162989916079,
4.1302292916296));
#39449=CARTESIAN_POINT('Ctrl Pts',(13.1773063939943,-0.527985828618295,
4.33787495524147));
#39450=CARTESIAN_POINT('Ctrl Pts',(13.1614011153067,-0.375035665205916,
4.46202728915223));
#39451=CARTESIAN_POINT('Ctrl Pts',(13.150549213957,-0.270680367988337,4.54673431669939));
#39452=CARTESIAN_POINT('Ctrl Pts',(13.1396973126073,-0.134776053786733,
4.59257435599745));
#39453=CARTESIAN_POINT('Ctrl Pts',(13.1288454112576,0.000488576923893258,
4.59361798633976));
#39454=CARTESIAN_POINT('Ctrl Pts',(13.0211545887425,0.000215375668158819,
4.59498635240753));
#39455=CARTESIAN_POINT('Ctrl Pts',(13.0361060098081,-0.185045360160338,
4.59412349007018));
#39456=CARTESIAN_POINT('Ctrl Pts',(13.0510574308736,-0.371056311319581,
4.5007301079696));
#39457=CARTESIAN_POINT('Ctrl Pts',(13.0660088519392,-0.480360474535337,
4.35124746348123));
#39458=CARTESIAN_POINT('Ctrl Pts',(13.0819141306268,-0.596637928700896,
4.19222825660313));
#39459=CARTESIAN_POINT('Ctrl Pts',(13.0978194093145,-0.626109048224722,
3.96973483302036));
#39460=CARTESIAN_POINT('Ctrl Pts',(13.1137246880021,-0.555241941841719,
3.78592675992164));
#39461=CARTESIAN_POINT('Ctrl Pts',(13.1296299666897,-0.484374835458714,
3.60211868682292));
#39462=CARTESIAN_POINT('Ctrl Pts',(13.1455352453773,-0.313169503168878,
3.45699596420825));
#39463=CARTESIAN_POINT('Ctrl Pts',(13.1614405240649,-0.120236190459409,
3.4171928066662));
#39464=CARTESIAN_POINT('Ctrl Pts',(13.1773458027525,0.0726971222500488,
3.37738964912416));
#39465=CARTESIAN_POINT('Ctrl Pts',(13.1932510814401,0.287358415379145,3.44290605665475));
#39466=CARTESIAN_POINT('Ctrl Pts',(13.2091563601277,0.425184304693362,3.58365966669054));
#39467=CARTESIAN_POINT('Ctrl Pts',(13.2250616388154,0.563010194007583,3.72441327672633));
#39468=CARTESIAN_POINT('Ctrl Pts',(13.240966917503,0.624000679506934,3.94040408926733));
#39469=CARTESIAN_POINT('Ctrl Pts',(13.2568721961906,0.580151510544767,4.13245826101242));
#39470=CARTESIAN_POINT('Ctrl Pts',(13.2727774748782,0.536302341582597,4.32451243275751));
#39471=CARTESIAN_POINT('Ctrl Pts',(13.2886827535658,0.387613518158899,4.49262996370669));
#39472=CARTESIAN_POINT('Ctrl Pts',(13.3045880322534,0.202356657484476,4.55961839611428));
#39473=CARTESIAN_POINT('Ctrl Pts',(13.3101102177498,0.13803695776657,4.58287624384712));
#39474=CARTESIAN_POINT('Ctrl Pts',(13.3156324032461,0.0693092633201986,
4.59394375907155));
#39475=CARTESIAN_POINT('Ctrl Pts',(13.3211545887425,0.000436239896754628,
4.59347700091179));
#39476=CARTESIAN_POINT('Origin',(4.,0.,4.));
#39477=CARTESIAN_POINT('',(13.7288454112576,-0.000361622974213827,4.59480268714608));
#39478=CARTESIAN_POINT('',(13.6211545887425,-0.000396530615921017,4.59339874939382));
#39479=CARTESIAN_POINT('',(4.,-7.27562663373442E-17,4.5941));
#39480=CARTESIAN_POINT('Ctrl Pts',(13.7288454112576,-0.000361622974213827,
4.59480268714608));
#39481=CARTESIAN_POINT('Ctrl Pts',(13.714655378171,0.175608319374377,4.59354294412002));
#39482=CARTESIAN_POINT('Ctrl Pts',(13.7004653450845,0.352610168065205,4.51056419690263));
#39483=CARTESIAN_POINT('Ctrl Pts',(13.6862753119979,0.463013835099274,4.37381700684221));
#39484=CARTESIAN_POINT('Ctrl Pts',(13.6703700333103,0.586762742631886,4.22054025587244));
#39485=CARTESIAN_POINT('Ctrl Pts',(13.6544647546227,0.626840040937572,3.99971072753873));
#39486=CARTESIAN_POINT('Ctrl Pts',(13.6385594759351,0.564843930165024,3.81272399872504));
#39487=CARTESIAN_POINT('Ctrl Pts',(13.6226541972475,0.502847819392478,3.62573726991136));
#39488=CARTESIAN_POINT('Ctrl Pts',(13.6067489185599,0.338778299541704,3.4725933406177));
#39489=CARTESIAN_POINT('Ctrl Pts',(13.5908436398723,0.147969152919217,3.42360942419035));
#39490=CARTESIAN_POINT('Ctrl Pts',(13.5749383611846,-0.0428399937032757,
3.37462550776301));
#39491=CARTESIAN_POINT('Ctrl Pts',(13.559033082497,-0.260388767097474,3.42980160420198));
#39492=CARTESIAN_POINT('Ctrl Pts',(13.5431278038094,-0.404787974250376,
3.56380318433064));
#39493=CARTESIAN_POINT('Ctrl Pts',(13.5272225251218,-0.549187181403275,
3.6978047644593));
#39494=CARTESIAN_POINT('Ctrl Pts',(13.5113172464342,-0.620436822314871,
3.91063182827765));
#39495=CARTESIAN_POINT('Ctrl Pts',(13.4954119677466,-0.585822076202281,
4.10456319205082));
#39496=CARTESIAN_POINT('Ctrl Pts',(13.479506689059,-0.551207330089691,4.298494555824));
#39497=CARTESIAN_POINT('Ctrl Pts',(13.4636014103714,-0.410728196952908,
4.47353021955202));
#39498=CARTESIAN_POINT('Ctrl Pts',(13.4476961316837,-0.228886751546343,
4.54930121159921));
#39499=CARTESIAN_POINT('Ctrl Pts',(13.4414125582084,-0.15704808052867,4.57923546205676));
#39500=CARTESIAN_POINT('Ctrl Pts',(13.435128984733,-0.0787538239969463,
4.5936770685736));
#39501=CARTESIAN_POINT('Ctrl Pts',(13.4288454112576,-0.000323145728561625,
4.59329116515504));
#39502=CARTESIAN_POINT('Ctrl Pts',(13.3211545887425,0.000436239896754628,
4.59347700091179));
#39503=CARTESIAN_POINT('Ctrl Pts',(13.3315376819337,-0.129062311182503,
4.59259937855127));
#39504=CARTESIAN_POINT('Ctrl Pts',(13.341920775125,-0.259074650003773,4.55094414667863));
#39505=CARTESIAN_POINT('Ctrl Pts',(13.3523038683163,-0.361265427801182,
4.47287234722855));
#39506=CARTESIAN_POINT('Ctrl Pts',(13.3682091470039,-0.517805754487323,
4.35327853206923));
#39507=CARTESIAN_POINT('Ctrl Pts',(13.3841144256915,-0.609061509934468,
4.14823156788458));
#39508=CARTESIAN_POINT('Ctrl Pts',(13.4000197043791,-0.593131911953917,
3.95188034580653));
#39509=CARTESIAN_POINT('Ctrl Pts',(13.4159249830667,-0.577202313973367,
3.75552912372848));
#39510=CARTESIAN_POINT('Ctrl Pts',(13.4318302617543,-0.454087362565127,
3.56787364375704));
#39511=CARTESIAN_POINT('Ctrl Pts',(13.4477355404419,-0.280316234851803,
3.47507736324643));
#39512=CARTESIAN_POINT('Ctrl Pts',(13.4636408191295,-0.106545107138479,
3.38228108273583));
#39513=CARTESIAN_POINT('Ctrl Pts',(13.4795460978172,0.117882196879929,3.38434400168606));
#39514=CARTESIAN_POINT('Ctrl Pts',(13.4954513765048,0.2899181539344,3.48031891499009));
#39515=CARTESIAN_POINT('Ctrl Pts',(13.5113566551924,0.461954110988876,3.57629382829412));
#39516=CARTESIAN_POINT('Ctrl Pts',(13.52726193388,0.581598721079409,3.76618073595195));
#39517=CARTESIAN_POINT('Ctrl Pts',(13.5431672125676,0.593916240998451,3.96279160341967));
#39518=CARTESIAN_POINT('Ctrl Pts',(13.5590724912552,0.606233760917493,4.15940247088739));
#39519=CARTESIAN_POINT('Ctrl Pts',(13.5749777699428,0.511224190665043,4.362737298165));
#39520=CARTESIAN_POINT('Ctrl Pts',(13.5908830486304,0.352511905377589,4.47943333495374));
#39521=CARTESIAN_POINT('Ctrl Pts',(13.6009735620011,0.251822790258117,4.55346680161908));
#39522=CARTESIAN_POINT('Ctrl Pts',(13.6110640753718,0.125494626822297,4.59262991567553));
#39523=CARTESIAN_POINT('Ctrl Pts',(13.6211545887425,-0.000396530615921017,
4.59339874939382));
#39524=CARTESIAN_POINT('Origin',(4.,0.,4.));
#39525=CARTESIAN_POINT('',(14.0288454112576,0.000507412974116619,4.59441995931617));
#39526=CARTESIAN_POINT('',(13.9211545887425,-0.000275297881949146,4.59492513410986));
#39527=CARTESIAN_POINT('',(4.,-7.27562663373442E-17,4.5941));
#39528=CARTESIAN_POINT('Ctrl Pts',(14.0288454112576,0.000507412974116619,
4.59441995931617));
#39529=CARTESIAN_POINT('Ctrl Pts',(14.0259923289843,0.0359476882196221,
4.59474138052009));
#39530=CARTESIAN_POINT('Ctrl Pts',(14.0231392467111,0.0713355155074759,
4.59184535342408));
#39531=CARTESIAN_POINT('Ctrl Pts',(14.0202861644378,0.106106362061302,4.58554453803953));
#39532=CARTESIAN_POINT('Ctrl Pts',(14.0043808857502,0.299945849210873,4.55041893875697));
#39533=CARTESIAN_POINT('Ctrl Pts',(13.9884756070626,0.474610768799237,4.40947910659883));
#39534=CARTESIAN_POINT('Ctrl Pts',(13.972570328375,0.549902379214768,4.22743864981956));
#39535=CARTESIAN_POINT('Ctrl Pts',(13.9566650496873,0.625193989630293,4.04539819304031));
#39536=CARTESIAN_POINT('Ctrl Pts',(13.9407597709997,0.601112290873006,3.82225711163994));
#39537=CARTESIAN_POINT('Ctrl Pts',(13.9248544923121,0.488714580199595,3.66047234987686));
#39538=CARTESIAN_POINT('Ctrl Pts',(13.9089492136245,0.376316869526181,3.49868758811377));
#39539=CARTESIAN_POINT('Ctrl Pts',(13.8930439349369,0.175603146936639,3.39825914598798));
#39540=CARTESIAN_POINT('Ctrl Pts',(13.8771386562493,-0.0212673376532481,
3.40529951534663));
#39541=CARTESIAN_POINT('Ctrl Pts',(13.8612333775617,-0.218137822243141,
3.41233988470529));
#39542=CARTESIAN_POINT('Ctrl Pts',(13.8453280988741,-0.411165068833379,
3.52684906554841));
#39543=CARTESIAN_POINT('Ctrl Pts',(13.8294228201864,-0.511719132099071,
3.69624928651676));
#39544=CARTESIAN_POINT('Ctrl Pts',(13.8135175414988,-0.612273195364761,
3.8656495074851));
#39545=CARTESIAN_POINT('Ctrl Pts',(13.7976122628112,-0.62035407530591,4.08994076857866));
#39546=CARTESIAN_POINT('Ctrl Pts',(13.7817069841236,-0.532251373727382,
4.26613801168402));
#39547=CARTESIAN_POINT('Ctrl Pts',(13.765801705436,-0.44414867214885,4.44233525478938));
#39548=CARTESIAN_POINT('Ctrl Pts',(13.7498964267484,-0.259862389050636,
4.57043847990653));
#39549=CARTESIAN_POINT('Ctrl Pts',(13.7339911480608,-0.0640089891217576,
4.59162810566218));
#39550=CARTESIAN_POINT('Ctrl Pts',(13.7322759024597,-0.0428879079209441,
4.59391322201126));
#39551=CARTESIAN_POINT('Ctrl Pts',(13.7305606568586,-0.0216323041412813,
4.594954960835));
#39552=CARTESIAN_POINT('Ctrl Pts',(13.7288454112576,-0.000361622974213827,
4.59480268714608));
#39553=CARTESIAN_POINT('Ctrl Pts',(13.6211545887425,-0.000396530615921017,
4.59339874939382));
#39554=CARTESIAN_POINT('Ctrl Pts',(13.6269693540594,-0.0729426448807452,
4.59384179797573));
#39555=CARTESIAN_POINT('Ctrl Pts',(13.6327841193764,-0.145343639818557,
4.58153501668255));
#39556=CARTESIAN_POINT('Ctrl Pts',(13.6385988846933,-0.212609537044371,
4.5558040579697));
#39557=CARTESIAN_POINT('Ctrl Pts',(13.6545041633809,-0.396603693856438,
4.48542149789704));
#39558=CARTESIAN_POINT('Ctrl Pts',(13.6704094420685,-0.542177007158105,
4.31459913145184));
#39559=CARTESIAN_POINT('Ctrl Pts',(13.6863147207561,-0.582488370180261,
4.12177136240739));
#39560=CARTESIAN_POINT('Ctrl Pts',(13.7022199994437,-0.622799733202417,
3.92894359336294));
#39561=CARTESIAN_POINT('Ctrl Pts',(13.7181252781313,-0.557849145945042,
3.71411042171923));
#39562=CARTESIAN_POINT('Ctrl Pts',(13.734030556819,-0.417459170243993,3.57591415105311));
#39563=CARTESIAN_POINT('Ctrl Pts',(13.7499358355066,-0.277069194542941,
3.43771788038699));
#39564=CARTESIAN_POINT('Ctrl Pts',(13.7658411141942,-0.0612398303982075,
3.37615851069845));
#39565=CARTESIAN_POINT('Ctrl Pts',(13.7817463928818,0.130929209162332,3.41950150018632));
#39566=CARTESIAN_POINT('Ctrl Pts',(13.7976516715694,0.323098248722867,3.46284448967418));
#39567=CARTESIAN_POINT('Ctrl Pts',(13.813556950257,0.491606963699209,3.61108983833845));
#39568=CARTESIAN_POINT('Ctrl Pts',(13.8294622289446,0.559083281190044,3.79616955381596));
#39569=CARTESIAN_POINT('Ctrl Pts',(13.8453675076322,0.62655959868088,3.98124926929349));
#39570=CARTESIAN_POINT('Ctrl Pts',(13.8612727863198,0.593003518686204,4.20316335158427));
#39571=CARTESIAN_POINT('Ctrl Pts',(13.8771780650075,0.4738225734989,4.36001824251097));
#39572=CARTESIAN_POINT('Ctrl Pts',(13.8918369062525,0.363981395029584,4.50458099992985));
#39573=CARTESIAN_POINT('Ctrl Pts',(13.9064957474975,0.181409709145346,4.59388191268165));
#39574=CARTESIAN_POINT('Ctrl Pts',(13.9211545887425,-0.000275297881949146,
4.59492513410986));
#39575=CARTESIAN_POINT('Origin',(4.,0.,4.));
#39576=CARTESIAN_POINT('',(14.3288454112576,0.000109044058801022,4.5931342436645));
#39577=CARTESIAN_POINT('',(14.2211545887425,0.000537210645871958,4.59424369460725));
#39578=CARTESIAN_POINT('',(4.,-7.27562663373442E-17,4.5941));
#39579=CARTESIAN_POINT('Ctrl Pts',(14.3288454112576,0.000109044058801022,
4.5931342436645));
#39580=CARTESIAN_POINT('Ctrl Pts',(14.32142400111,0.0928032711674493,4.59328573107644));
#39581=CARTESIAN_POINT('Ctrl Pts',(14.3140025909624,0.185434358886594,4.57287353691408));
#39582=CARTESIAN_POINT('Ctrl Pts',(14.3065811808148,0.267539471941071,4.53154830171049));
#39583=CARTESIAN_POINT('Ctrl Pts',(14.2906759021272,0.443503969097433,4.44298165875801));
#39584=CARTESIAN_POINT('Ctrl Pts',(14.2747706234396,0.571121189235106,4.25835848700565));
#39585=CARTESIAN_POINT('Ctrl Pts',(14.258865344752,0.591794703906212,4.06244993615984));
#39586=CARTESIAN_POINT('Ctrl Pts',(14.2429600660644,0.612468218577319,3.86654138531401));
#39587=CARTESIAN_POINT('Ctrl Pts',(14.2270547873768,0.526198027781844,3.65934745537473));
#39588=CARTESIAN_POINT('Ctrl Pts',(14.2111495086891,0.372595753342289,3.53600283331781));
#39589=CARTESIAN_POINT('Ctrl Pts',(14.1952442300015,0.218993478902743,3.4126582112609));
#39590=CARTESIAN_POINT('Ctrl Pts',(14.1793389513139,-0.00194087918087354,
3.37316289708635));
#39591=CARTESIAN_POINT('Ctrl Pts',(14.1634336726263,-0.18876361063844,3.43565146815417));
#39592=CARTESIAN_POINT('Ctrl Pts',(14.1475283939387,-0.375586342096006,
3.49814003922198));
#39593=CARTESIAN_POINT('Ctrl Pts',(14.1316231152511,-0.528297446927522,
3.66261249553216));
#39594=CARTESIAN_POINT('Ctrl Pts',(14.1157178365635,-0.576778446468407,
3.85355004340287));
#39595=CARTESIAN_POINT('Ctrl Pts',(14.0998125578759,-0.625259446009293,
4.04448759127359));
#39596=CARTESIAN_POINT('Ctrl Pts',(14.0839072791882,-0.569510340259543,
4.26189023070484));
#39597=CARTESIAN_POINT('Ctrl Pts',(14.0680020005006,-0.435128760029281,
4.40593586721696));
#39598=CARTESIAN_POINT('Ctrl Pts',(14.0549498040863,-0.324852491748397,
4.52414265738481));
#39599=CARTESIAN_POINT('Ctrl Pts',(14.0418976076719,-0.161623710204441,
4.5929495310973));
#39600=CARTESIAN_POINT('Ctrl Pts',(14.0288454112576,0.000507412974116619,
4.59441995931617));
#39601=CARTESIAN_POINT('Ctrl Pts',(13.9211545887425,-0.000275297881949146,
4.59492513410986));
#39602=CARTESIAN_POINT('Ctrl Pts',(13.9224010261851,-0.015723926578741,
4.59501383895544));
#39603=CARTESIAN_POINT('Ctrl Pts',(13.9236474636277,-0.0311661445373128,
4.59446443570748));
#39604=CARTESIAN_POINT('Ctrl Pts',(13.9248939010703,-0.0465566941337027,
4.59325663951544));
#39605=CARTESIAN_POINT('Ctrl Pts',(13.9407991797579,-0.242949206199084,
4.5778444460306));
#39606=CARTESIAN_POINT('Ctrl Pts',(13.9567044584455,-0.430928419949921,
4.4552243594983));
#39607=CARTESIAN_POINT('Ctrl Pts',(13.9726097371331,-0.524182233176515,
4.28169833602613));
#39608=CARTESIAN_POINT('Ctrl Pts',(13.9885150158207,-0.617436046403107,
4.10817231255396));
#39609=CARTESIAN_POINT('Ctrl Pts',(14.0044202945084,-0.615964459105464,
3.88374035214192));
#39610=CARTESIAN_POINT('Ctrl Pts',(14.020325573196,-0.52044316191294,3.71145211607799));
#39611=CARTESIAN_POINT('Ctrl Pts',(14.0362308518836,-0.424921864720413,
3.53916388001405));
#39612=CARTESIAN_POINT('Ctrl Pts',(14.0521361305712,-0.235350857633014,
3.41901936829824));
#39613=CARTESIAN_POINT('Ctrl Pts',(14.0680414092588,-0.0387731270173405,
3.40618385781531));
#39614=CARTESIAN_POINT('Ctrl Pts',(14.0839466879464,0.157804603598333,3.39334834733239));
#39615=CARTESIAN_POINT('Ctrl Pts',(14.0998519666341,0.361389057742269,3.48782183808236));
#39616=CARTESIAN_POINT('Ctrl Pts',(14.1157572453217,0.478502867019537,3.64622609995664));
#39617=CARTESIAN_POINT('Ctrl Pts',(14.1316625240093,0.595616676296804,3.80463036183091));
#39618=CARTESIAN_POINT('Ctrl Pts',(14.1475678026969,0.626259840707404,4.02696539482948));
#39619=CARTESIAN_POINT('Ctrl Pts',(14.1634730813845,0.556362315559365,4.21114435801894));
#39620=CARTESIAN_POINT('Ctrl Pts',(14.1793783600721,0.486464790411328,4.3953233212084));
#39621=CARTESIAN_POINT('Ctrl Pts',(14.1952836387597,0.316026575704654,4.54134621458875));
#39622=CARTESIAN_POINT('Ctrl Pts',(14.2111889174473,0.123305688986428,4.58216550323889));
#39623=CARTESIAN_POINT('Ctrl Pts',(14.2145108078791,0.0830550475387342,
4.59069079896363));
#39624=CARTESIAN_POINT('Ctrl Pts',(14.2178326983108,0.0418324306113591,
4.59462708830176));
#39625=CARTESIAN_POINT('Ctrl Pts',(14.2211545887425,0.000537210645871958,
4.59424369460725));
#39626=CARTESIAN_POINT('Origin',(4.,0.,4.));
#39627=CARTESIAN_POINT('',(14.6288454112575,-0.000548182068839831,4.59401855345973));
#39628=CARTESIAN_POINT('',(14.5211545887425,1.28950532977596E-5,4.59311636453746));
#39629=CARTESIAN_POINT('',(4.,-7.27562663373442E-17,4.5941));
#39630=CARTESIAN_POINT('Ctrl Pts',(14.6288454112575,-0.000548182068839831,
4.59401855345973));
#39631=CARTESIAN_POINT('Ctrl Pts',(14.6168556732357,0.148643716013534,4.59265593252186));
#39632=CARTESIAN_POINT('Ctrl Pts',(14.6048659352138,0.29876355451001,4.53564313143304));
#39633=CARTESIAN_POINT('Ctrl Pts',(14.5928761971919,0.407080942069735,4.43405768361063));
#39634=CARTESIAN_POINT('Ctrl Pts',(14.5769709185042,0.55077200793829,4.29929703619113));
#39635=CARTESIAN_POINT('Ctrl Pts',(14.5610656398166,0.620899143473568,4.08609746938767));
#39636=CARTESIAN_POINT('Ctrl Pts',(14.545160361129,0.585262934872208,3.89235120454656));
#39637=CARTESIAN_POINT('Ctrl Pts',(14.5292550824414,0.549626726270847,3.69860493970543));
#39638=CARTESIAN_POINT('Ctrl Pts',(14.5133498037538,0.408227173532835,3.52431197682665));
#39639=CARTESIAN_POINT('Ctrl Pts',(14.4974445250662,0.225988969153725,3.44950027073699));
#39640=CARTESIAN_POINT('Ctrl Pts',(14.4815392463786,0.04375076477463,3.37468856464734));
#39641=CARTESIAN_POINT('Ctrl Pts',(14.465633967691,-0.179326091245555,3.39935811534679));
#39642=CARTESIAN_POINT('Ctrl Pts',(14.4497286890033,-0.340814144225853,
3.51218170883678));
#39643=CARTESIAN_POINT('Ctrl Pts',(14.4338234103157,-0.50230219720616,3.62500530232677));
#39644=CARTESIAN_POINT('Ctrl Pts',(14.4179181316281,-0.602201447146573,
3.82598293860731));
#39645=CARTESIAN_POINT('Ctrl Pts',(14.4020128529405,-0.594642384863179,
4.02283418976097));
#39646=CARTESIAN_POINT('Ctrl Pts',(14.3861075742529,-0.587083322579785,
4.21968544091462));
#39647=CARTESIAN_POINT('Ctrl Pts',(14.3702022955653,-0.47206594807259,4.4124103069414));
#39648=CARTESIAN_POINT('Ctrl Pts',(14.3542970168777,-0.302401373731467,
4.51251768287848));
#39649=CARTESIAN_POINT('Ctrl Pts',(14.3458131483376,-0.211902365642262,
4.565914912441));
#39650=CARTESIAN_POINT('Ctrl Pts',(14.3373292797976,-0.10585540495725,4.59296106912451));
#39651=CARTESIAN_POINT('Ctrl Pts',(14.3288454112576,0.000109044058801022,
4.5931342436645));
#39652=CARTESIAN_POINT('Ctrl Pts',(14.2211545887425,0.000537210645871958,
4.59424369460725));
#39653=CARTESIAN_POINT('Ctrl Pts',(14.2337379769984,-0.155889919212927,
4.59279139152499));
#39654=CARTESIAN_POINT('Ctrl Pts',(14.2463213652543,-0.313358837143528,
4.52935553548989));
#39655=CARTESIAN_POINT('Ctrl Pts',(14.2589047535102,-0.422984449084643,
4.4185751090669));
#39656=CARTESIAN_POINT('Ctrl Pts',(14.2748100321978,-0.561550141707708,
4.27854974232482));
#39657=CARTESIAN_POINT('Ctrl Pts',(14.2907153108854,-0.623677968224056,
4.06288332492072));
#39658=CARTESIAN_POINT('Ctrl Pts',(14.306620589573,-0.580841459108965,3.87060075163287));
#39659=CARTESIAN_POINT('Ctrl Pts',(14.3225258682606,-0.538004949993874,
3.67831817834502));
#39660=CARTESIAN_POINT('Ctrl Pts',(14.3384311469482,-0.390204105247342,
3.50941944917344));
#39661=CARTESIAN_POINT('Ctrl Pts',(14.3543364256359,-0.205302819838896,
3.44145571503774));
#39662=CARTESIAN_POINT('Ctrl Pts',(14.3702417043235,-0.0204015344304391,
3.37349198090203));
#39663=CARTESIAN_POINT('Ctrl Pts',(14.3861469830111,0.201600191639931,3.40646324180223));
#39664=CARTESIAN_POINT('Ctrl Pts',(14.4020522616987,0.358768557879186,3.52523048963197));
#39665=CARTESIAN_POINT('Ctrl Pts',(14.4179575403863,0.515936924118427,3.6439977374617));
#39666=CARTESIAN_POINT('Ctrl Pts',(14.4338628190739,0.608271930526566,3.84856097222098));
#39667=CARTESIAN_POINT('Ctrl Pts',(14.4497680977615,0.59337724853295,4.04499341086509));
#39668=CARTESIAN_POINT('Ctrl Pts',(14.4656733764491,0.578482566539332,4.2414258495092));
#39669=CARTESIAN_POINT('Ctrl Pts',(14.4815786551367,0.456358196143958,4.42972749203816));
#39670=CARTESIAN_POINT('Ctrl Pts',(14.4974839338244,0.283078481576349,4.52343819058819));
#39671=CARTESIAN_POINT('Ctrl Pts',(14.5053741521304,0.197118668938093,4.56992576768087));
#39672=CARTESIAN_POINT('Ctrl Pts',(14.5132643704364,0.0985699939877532,
4.59313537862966));
#39673=CARTESIAN_POINT('Ctrl Pts',(14.5211545887425,1.28950532977596E-5,
4.59311636453746));
#39674=CARTESIAN_POINT('Origin',(4.,0.,4.));
#39675=CARTESIAN_POINT('',(14.9288454112575,0.000149915246051877,4.59503491979621));
#39676=CARTESIAN_POINT('',(14.8211545887425,-0.000542004001680995,4.59419620878869));
#39677=CARTESIAN_POINT('',(4.,-7.27562663373442E-17,4.5941));
#39678=CARTESIAN_POINT('Ctrl Pts',(14.9288454112575,0.000149915246051877,
4.59503491979621));
#39679=CARTESIAN_POINT('Ctrl Pts',(14.9281926240489,0.00823674021970066,
4.59506221957623));
#39680=CARTESIAN_POINT('Ctrl Pts',(14.9275398368403,0.0163225255999611,
4.59491168338633));
#39681=CARTESIAN_POINT('Ctrl Pts',(14.9268870496317,0.0244008833477238,
4.59458015690877));
#39682=CARTESIAN_POINT('Ctrl Pts',(14.9109817709441,0.221231534471853,4.58650245417764));
#39683=CARTESIAN_POINT('Ctrl Pts',(14.8950764922565,0.413652681988333,4.47097768448731));
#39684=CARTESIAN_POINT('Ctrl Pts',(14.8791712135689,0.513312675625014,4.30104993462962));
#39685=CARTESIAN_POINT('Ctrl Pts',(14.8632659348813,0.612972669261697,4.13112218477192));
#39686=CARTESIAN_POINT('Ctrl Pts',(14.8473606561937,0.619871509018575,3.90679145474687));
#39687=CARTESIAN_POINT('Ctrl Pts',(14.831455377506,0.530841539545133,3.73106092513143));
#39688=CARTESIAN_POINT('Ctrl Pts',(14.8155500988184,0.441811570071688,3.55533039551599));
#39689=CARTESIAN_POINT('Ctrl Pts',(14.7996448201308,0.256852791367914,3.42820006631018));
#39690=CARTESIAN_POINT('Ctrl Pts',(14.7837395414432,0.0608904496539635,
3.40804280624462));
#39691=CARTESIAN_POINT('Ctrl Pts',(14.7678342627556,-0.135071892059981,
3.38788554617906));
#39692=CARTESIAN_POINT('Ctrl Pts',(14.751928984068,-0.342037796784102,3.47470135525375));
#39693=CARTESIAN_POINT('Ctrl Pts',(14.7360237053804,-0.464977277074429,
3.62862808681558));
#39694=CARTESIAN_POINT('Ctrl Pts',(14.7201184266927,-0.587916757364756,
3.78255481837741));
#39695=CARTESIAN_POINT('Ctrl Pts',(14.7042131480052,-0.62682981322129,4.00359247242638));
#39696=CARTESIAN_POINT('Ctrl Pts',(14.6883078693175,-0.56384921567034,4.19024990955517));
#39697=CARTESIAN_POINT('Ctrl Pts',(14.6724025906299,-0.500868618119389,
4.37690734668397));
#39698=CARTESIAN_POINT('Ctrl Pts',(14.6564973119423,-0.335994367160947,
4.52918456689258));
#39699=CARTESIAN_POINT('Ctrl Pts',(14.6405920332547,-0.144929743580805,
4.57716231297912));
#39700=CARTESIAN_POINT('Ctrl Pts',(14.636676492589,-0.097893704910838,4.5889734116427));
#39701=CARTESIAN_POINT('Ctrl Pts',(14.6327609519233,-0.0492704262804658,
4.59446355048005));
#39702=CARTESIAN_POINT('Ctrl Pts',(14.6288454112575,-0.000548182068839831,
4.59401855345973));
#39703=CARTESIAN_POINT('Ctrl Pts',(14.5211545887425,1.28950532977596E-5,
4.59311636453746));
#39704=CARTESIAN_POINT('Ctrl Pts',(14.5291696491241,-0.100103612291989,
4.59309704959697));
#39705=CARTESIAN_POINT('Ctrl Pts',(14.5371847095056,-0.200228812305367,
4.56910822985942));
#39706=CARTESIAN_POINT('Ctrl Pts',(14.5451997698872,-0.287175610734119,
4.52120162576233));
#39707=CARTESIAN_POINT('Ctrl Pts',(14.5611050485748,-0.459714929737158,
4.42613460781534));
#39708=CARTESIAN_POINT('Ctrl Pts',(14.5770103272624,-0.580358509003398,
4.23688081735026));
#39709=CARTESIAN_POINT('Ctrl Pts',(14.59291560595,-0.593711920942704,4.04033758828107));
#39710=CARTESIAN_POINT('Ctrl Pts',(14.6088208846377,-0.607065332882009,
3.84379435921188));
#39711=CARTESIAN_POINT('Ctrl Pts',(14.6247261633253,-0.513128577494387,
3.63996169153858));
#39712=CARTESIAN_POINT('Ctrl Pts',(14.6406314420129,-0.35503343871745,3.52243092280774));
#39713=CARTESIAN_POINT('Ctrl Pts',(14.6565367207005,-0.196938299940509,
3.40490015407689));
#39714=CARTESIAN_POINT('Ctrl Pts',(14.6724419993881,0.025315222225754,3.37367128428849));
#39715=CARTESIAN_POINT('Ctrl Pts',(14.6883472780757,0.209677713173688,3.44308328926485));
#39716=CARTESIAN_POINT('Ctrl Pts',(14.7042525567633,0.394040204121622,3.51249529424121));
#39717=CARTESIAN_POINT('Ctrl Pts',(14.720157835451,0.540511663851219,3.68254817398232));
#39718=CARTESIAN_POINT('Ctrl Pts',(14.7360631141386,0.581838594751101,3.87516084045512));
#39719=CARTESIAN_POINT('Ctrl Pts',(14.7519683928262,0.623165525650983,4.06777350692792));
#39720=CARTESIAN_POINT('Ctrl Pts',(14.7678736715138,0.559347927721136,4.2829459601324));
#39721=CARTESIAN_POINT('Ctrl Pts',(14.7837789502014,0.419688142031033,4.42188011275284));
#39722=CARTESIAN_POINT('Ctrl Pts',(14.7962374963817,0.310293146587505,4.53070672248707));
#39723=CARTESIAN_POINT('Ctrl Pts',(14.8086960425621,0.154364940471616,4.59275708529138));
#39724=CARTESIAN_POINT('Ctrl Pts',(14.8211545887425,-0.000542004001680995,
4.59419620878869));
#39725=CARTESIAN_POINT('Origin',(4.,0.,4.));
#39726=CARTESIAN_POINT('',(15.2288454112576,0.000471544078774977,4.59356550157774));
#39727=CARTESIAN_POINT('',(15.1211545887425,0.000250233060073018,4.59495282954609));
#39728=CARTESIAN_POINT('',(4.,-7.27562663373442E-17,4.5941));
#39729=CARTESIAN_POINT('Ctrl Pts',(15.2288454112576,0.000471544078774977,
4.59356550157774));
#39730=CARTESIAN_POINT('Ctrl Pts',(15.2236242961746,0.0655651715058866,
4.59404721416646));
#39731=CARTESIAN_POINT('Ctrl Pts',(15.2184031810917,0.130516835945995,4.58418155789741));
#39732=CARTESIAN_POINT('Ctrl Pts',(15.2131820660088,0.191734887706884,4.56334598510492));
#39733=CARTESIAN_POINT('Ctrl Pts',(15.1972767873211,0.378225734681762,4.49987379829874));
#39734=CARTESIAN_POINT('Ctrl Pts',(15.1813715086335,0.530068013118856,4.33459889729257));
#39735=CARTESIAN_POINT('Ctrl Pts',(15.1654662299459,0.577542172676889,4.143408524424));
#39736=CARTESIAN_POINT('Ctrl Pts',(15.1495609512583,0.625016332234921,3.95221815155542));
#39737=CARTESIAN_POINT('Ctrl Pts',(15.1336556725707,0.568122372913892,3.73511230682445));
#39738=CARTESIAN_POINT('Ctrl Pts',(15.1177503938831,0.432983593849097,3.59177680914072));
#39739=CARTESIAN_POINT('Ctrl Pts',(15.1018451151955,0.297844814784303,3.44844131145699));
#39740=CARTESIAN_POINT('Ctrl Pts',(15.0859398365078,0.0844612159757424,
3.37887616082051));
#39741=CARTESIAN_POINT('Ctrl Pts',(15.0700345578202,-0.109190481519281,
3.41502273134472));
#39742=CARTESIAN_POINT('Ctrl Pts',(15.0541292791326,-0.302842179014298,
3.45116930186893));
#39743=CARTESIAN_POINT('Ctrl Pts',(15.038224000445,-0.47676197519578,3.59302759355383));
#39744=CARTESIAN_POINT('Ctrl Pts',(15.0223187217574,-0.551093257596978,
3.77546228038711));
#39745=CARTESIAN_POINT('Ctrl Pts',(15.0064134430698,-0.625424539998176,
3.95789696722038));
#39746=CARTESIAN_POINT('Ctrl Pts',(14.9905081643822,-0.600167308619091,
4.18090804920204));
#39747=CARTESIAN_POINT('Ctrl Pts',(14.9746028856946,-0.486918615563658,
4.34209827230691));
#39748=CARTESIAN_POINT('Ctrl Pts',(14.9593503942156,-0.378317895025423,
4.49667289829699));
#39749=CARTESIAN_POINT('Ctrl Pts',(14.9440979027365,-0.188800216398263,
4.59439705548643));
#39750=CARTESIAN_POINT('Ctrl Pts',(14.9288454112575,0.000149915246051877,
4.59503491979621));
#39751=CARTESIAN_POINT('Ctrl Pts',(14.8211545887425,-0.000542004001680995,
4.59419620878869));
#39752=CARTESIAN_POINT('Ctrl Pts',(14.8246013212497,-0.0433979515083632,
4.5945943510493));
#39753=CARTESIAN_POINT('Ctrl Pts',(14.828048053757,-0.0861757330942537,
4.59035339483295));
#39754=CARTESIAN_POINT('Ctrl Pts',(14.8314947862642,-0.127868389248254,
4.58118038604969));
#39755=CARTESIAN_POINT('Ctrl Pts',(14.8474000649518,-0.320263161387096,
4.5388506546897));
#39756=CARTESIAN_POINT('Ctrl Pts',(14.8633053436395,-0.489550732214419,
4.39149533993331));
#39757=CARTESIAN_POINT('Ctrl Pts',(14.8792106223271,-0.558001411172811,
4.20677376822741));
#39758=CARTESIAN_POINT('Ctrl Pts',(14.8951159010147,-0.6264520901312,4.0220521965215));
#39759=CARTESIAN_POINT('Ctrl Pts',(14.9110211797023,-0.594065877220663,
3.79996436786608));
#39760=CARTESIAN_POINT('Ctrl Pts',(14.9269264583899,-0.475713151262041,
3.64248361741852));
#39761=CARTESIAN_POINT('Ctrl Pts',(14.9428317370775,-0.357360425303418,
3.48500286697096));
#39762=CARTESIAN_POINT('Ctrl Pts',(14.9587370157651,-0.153041186296697,
3.39212919473125));
#39763=CARTESIAN_POINT('Ctrl Pts',(14.9746422944528,0.0434298152403689,
3.40650626183085));
#39764=CARTESIAN_POINT('Ctrl Pts',(14.9905475731404,0.239900816777435,3.42088332893044));
#39765=CARTESIAN_POINT('Ctrl Pts',(15.006452851828,0.428523580844854,3.54251113536931));
#39766=CARTESIAN_POINT('Ctrl Pts',(15.0223581305156,0.522690514153935,3.71554333807889));
#39767=CARTESIAN_POINT('Ctrl Pts',(15.0382634092032,0.616857447463019,3.88857554078846));
#39768=CARTESIAN_POINT('Ctrl Pts',(15.0541686878908,0.616568550013756,4.11301213976874));
#39769=CARTESIAN_POINT('Ctrl Pts',(15.0700739665784,0.521956471292605,4.28580134389743));
#39770=CARTESIAN_POINT('Ctrl Pts',(15.085979245266,0.427344392571456,4.45859054802613));
#39771=CARTESIAN_POINT('Ctrl Pts',(15.1018845239536,0.238409132578427,4.57973235730324));
#39772=CARTESIAN_POINT('Ctrl Pts',(15.1177898026413,0.0419017695106382,
4.59360357799603));
#39773=CARTESIAN_POINT('Ctrl Pts',(15.1189113980083,0.0280446248267054,
4.59458173733358));
#39774=CARTESIAN_POINT('Ctrl Pts',(15.1200329933754,0.0141498265549413,
4.59502647517791));
#39775=CARTESIAN_POINT('Ctrl Pts',(15.1211545887425,0.000250233060073018,
4.59495282954609));
#39776=CARTESIAN_POINT('Origin',(4.,0.,4.));
#39777=CARTESIAN_POINT('',(15.5288454112575,-0.000350670266729247,4.59332700645389));
#39778=CARTESIAN_POINT('',(15.4211545887425,0.000414092275955974,4.59343115273787));
#39779=CARTESIAN_POINT('',(4.,-7.27562663373442E-17,4.5941));
#39780=CARTESIAN_POINT('Ctrl Pts',(15.5288454112575,-0.000350670266729247,
4.59332700645389));
#39781=CARTESIAN_POINT('Ctrl Pts',(15.5190559683003,0.121821298278883,4.59267222728074));
#39782=CARTESIAN_POINT('Ctrl Pts',(15.509266525343,0.244354036528086,4.55597946496206));
#39783=CARTESIAN_POINT('Ctrl Pts',(15.4994770823858,0.343380025451582,4.48601555964668));
#39784=CARTESIAN_POINT('Ctrl Pts',(15.4835718036982,0.504271299656008,4.37234255322809));
#39785=CARTESIAN_POINT('Ctrl Pts',(15.4676665250105,0.603110088323456,4.17084127710728));
#39786=CARTESIAN_POINT('Ctrl Pts',(15.4517612463229,0.594513801222153,3.97403259246294));
#39787=CARTESIAN_POINT('Ctrl Pts',(15.4358559676353,0.58591751412085,3.7772239078186));
#39788=CARTESIAN_POINT('Ctrl Pts',(15.4199506889477,0.469886151250777,3.58510781465072));
#39789=CARTESIAN_POINT('Ctrl Pts',(15.4040454102601,0.299696405559752,3.48589589518039));
#39790=CARTESIAN_POINT('Ctrl Pts',(15.3881401315725,0.129506659868722,3.38668397571006));
#39791=CARTESIAN_POINT('Ctrl Pts',(15.3722348528849,-0.0948414686432761,
3.38037622993726));
#39792=CARTESIAN_POINT('Ctrl Pts',(15.3563295741973,-0.270336810750117,
3.46986890786216));
#39793=CARTESIAN_POINT('Ctrl Pts',(15.3404242955096,-0.445832152856957,
3.55936158578705));
#39794=CARTESIAN_POINT('Ctrl Pts',(15.324519016822,-0.572474708558633,3.74465468740961));
#39795=CARTESIAN_POINT('Ctrl Pts',(15.3086137381344,-0.592115574081638,
3.94066945956945));
#39796=CARTESIAN_POINT('Ctrl Pts',(15.2927084594468,-0.611756439604643,
4.13668423172929));
#39797=CARTESIAN_POINT('Ctrl Pts',(15.2768031807592,-0.524395614948954,
4.3434206744264));
#39798=CARTESIAN_POINT('Ctrl Pts',(15.2608979020716,-0.370145494864779,
4.46595415947185));
#39799=CARTESIAN_POINT('Ctrl Pts',(15.2502137384669,-0.266529987624151,
4.54826443060822));
#39800=CARTESIAN_POINT('Ctrl Pts',(15.2395295748622,-0.13273198696893,4.59257975504152));
#39801=CARTESIAN_POINT('Ctrl Pts',(15.2288454112576,0.000471544078774977,
4.59356550157774));
#39802=CARTESIAN_POINT('Ctrl Pts',(15.1211545887425,0.000250233060073018,
4.59495282954609));
#39803=CARTESIAN_POINT('Ctrl Pts',(15.135938272063,-0.18295950063263,4.59398211075496));
#39804=CARTESIAN_POINT('Ctrl Pts',(15.1507219553836,-0.367002343096231,
4.50294888365168));
#39805=CARTESIAN_POINT('Ctrl Pts',(15.1655056387041,-0.476631971954554,
4.35629051265579));
#39806=CARTESIAN_POINT('Ctrl Pts',(15.1814109173917,-0.594578884209397,
4.19850559451431));
#39807=CARTESIAN_POINT('Ctrl Pts',(15.1973161960793,-0.626393242576541,
3.97633512612291));
#39808=CARTESIAN_POINT('Ctrl Pts',(15.2132214747669,-0.557467239648298,
3.79179038730953));
#39809=CARTESIAN_POINT('Ctrl Pts',(15.2291267534545,-0.488541236720055,
3.60724564849615));
#39810=CARTESIAN_POINT('Ctrl Pts',(15.2450320321422,-0.318874872496425,
3.46032663926078));
#39811=CARTESIAN_POINT('Ctrl Pts',(15.2609373108298,-0.126371763436977,
3.41849235301362));
#39812=CARTESIAN_POINT('Ctrl Pts',(15.2768425895174,0.0661313456224706,
3.37665806676646));
#39813=CARTESIAN_POINT('Ctrl Pts',(15.292747868205,0.281471199517752,3.4399085035075));
#39814=CARTESIAN_POINT('Ctrl Pts',(15.3086531468926,0.420772847618048,3.57920173859056));
#39815=CARTESIAN_POINT('Ctrl Pts',(15.3245584255802,0.560074495718348,3.71849497367363));
#39816=CARTESIAN_POINT('Ctrl Pts',(15.3404637042678,0.623337938023671,3.9338310070987));
#39817=CARTESIAN_POINT('Ctrl Pts',(15.3563689829554,0.581515278282945,4.12633664243329));
#39818=CARTESIAN_POINT('Ctrl Pts',(15.3722742616431,0.53969261854222,4.31884227776789));
#39819=CARTESIAN_POINT('Ctrl Pts',(15.3881795403307,0.392783856755445,4.48851751501199));
#39820=CARTESIAN_POINT('Ctrl Pts',(15.4040848190183,0.208243281137944,4.55745466359042));
#39821=CARTESIAN_POINT('Ctrl Pts',(15.4097747422597,0.142226097106806,4.58211610408423));
#39822=CARTESIAN_POINT('Ctrl Pts',(15.4154646655011,0.0713929250243718,
4.593885435962));
#39823=CARTESIAN_POINT('Ctrl Pts',(15.4211545887425,0.000414092275955974,
4.59343115273787));
#39824=CARTESIAN_POINT('Origin',(4.,0.,4.));
#39825=CARTESIAN_POINT('',(15.8288454112575,-0.000332254705457391,4.59484959654372));
#39826=CARTESIAN_POINT('',(15.7211545887425,-0.000419917270904514,4.59344262983929));
#39827=CARTESIAN_POINT('',(4.,-7.27562663373442E-17,4.5941));
#39828=CARTESIAN_POINT('Ctrl Pts',(15.8288454112575,-0.000332254705457391,
4.59484959654372));
#39829=CARTESIAN_POINT('Ctrl Pts',(15.814487640426,0.177680873019276,4.5936575613883));
#39830=CARTESIAN_POINT('Ctrl Pts',(15.8001298695944,0.356683508224643,4.50844978272675));
#39831=CARTESIAN_POINT('Ctrl Pts',(15.7857720987628,0.466927807092597,4.36891650689757));
#39832=CARTESIAN_POINT('Ctrl Pts',(15.7698668200752,0.589054446233417,4.21434406913608));
#39833=CARTESIAN_POINT('Ctrl Pts',(15.7539615413876,0.626802179063893,3.99310442736787));
#39834=CARTESIAN_POINT('Ctrl Pts',(15.7380562627,0.562838843643149,3.80678146521555));
#39835=CARTESIAN_POINT('Ctrl Pts',(15.7221509840123,0.498875508222402,3.62045850306322));
#39836=CARTESIAN_POINT('Ctrl Pts',(15.7062457053247,0.333201104550436,3.46905222052678));
#39837=CARTESIAN_POINT('Ctrl Pts',(15.6903404266371,0.141886309687413,3.42208197707538));
#39838=CARTESIAN_POINT('Ctrl Pts',(15.6744351479495,-0.0494284851756215,
3.37511173362399));
#39839=CARTESIAN_POINT('Ctrl Pts',(15.6585298692619,-0.266383671229707,
3.43257752925765));
#39840=CARTESIAN_POINT('Ctrl Pts',(15.6426245905743,-0.409362605655794,
3.5680935017987));
#39841=CARTESIAN_POINT('Ctrl Pts',(15.6267193118867,-0.552341540081869,
3.70360947433975));
#39842=CARTESIAN_POINT('Ctrl Pts',(15.6108140331991,-0.621344222879956,
3.9171756237882));
#39843=CARTESIAN_POINT('Ctrl Pts',(15.5949087545115,-0.584687541371933,
4.11073140955597));
#39844=CARTESIAN_POINT('Ctrl Pts',(15.5790034758238,-0.548030859863907,
4.30428719532377));
#39845=CARTESIAN_POINT('Ctrl Pts',(15.5630981971362,-0.405714814049763,
4.47783261741089));
#39846=CARTESIAN_POINT('Ctrl Pts',(15.5471929184486,-0.223084911271984,
4.55168296009627));
#39847=CARTESIAN_POINT('Ctrl Pts',(15.5410770827183,-0.152860773312716,
4.58007960584922));
#39848=CARTESIAN_POINT('Ctrl Pts',(15.5349612469879,-0.0766761255292402,
4.5937360717991));
#39849=CARTESIAN_POINT('Ctrl Pts',(15.5288454112575,-0.000350670266729247,
4.59332700645389));
#39850=CARTESIAN_POINT('Ctrl Pts',(15.4211545887425,0.000414092275955974,
4.59343115273787));
#39851=CARTESIAN_POINT('Ctrl Pts',(15.4313699441887,-0.12701715326484,4.59261555920332));
#39852=CARTESIAN_POINT('Ctrl Pts',(15.4415852996349,-0.254917899718674,
4.55240018390688));
#39853=CARTESIAN_POINT('Ctrl Pts',(15.4518006550811,-0.356261725310785,
4.47665348962993));
#39854=CARTESIAN_POINT('Ctrl Pts',(15.4677059337687,-0.514053766693778,
4.35871610717824));
#39855=CARTESIAN_POINT('Ctrl Pts',(15.4836112124564,-0.607465460011524,
4.15464228236211));
#39856=CARTESIAN_POINT('Ctrl Pts',(15.499516491144,-0.593606107615349,3.95813408188558));
#39857=CARTESIAN_POINT('Ctrl Pts',(15.5154217698316,-0.579746755219174,
3.76162588140906));
#39858=CARTESIAN_POINT('Ctrl Pts',(15.5313270485192,-0.458616357109098,
3.57268330527213));
#39859=CARTESIAN_POINT('Ctrl Pts',(15.5472323272068,-0.285832867492734,
3.47806079093568));
#39860=CARTESIAN_POINT('Ctrl Pts',(15.5631376058944,-0.113049377876356,
3.38343827659922));
#39861=CARTESIAN_POINT('Ctrl Pts',(15.579042884582,0.111387203246309,3.38313582406324));
#39862=CARTESIAN_POINT('Ctrl Pts',(15.5949481632696,0.284425092952457,3.47729230673655));
#39863=CARTESIAN_POINT('Ctrl Pts',(15.6108534419572,0.457462982658595,3.57144878940986));
#39864=CARTESIAN_POINT('Ctrl Pts',(15.6267587206449,0.579102180948212,3.76006420729246));
#39865=CARTESIAN_POINT('Ctrl Pts',(15.6426639993325,0.593491114096805,3.95653434015292));
#39866=CARTESIAN_POINT('Ctrl Pts',(15.6585692780201,0.607880047245398,4.15300447301339));
#39867=CARTESIAN_POINT('Ctrl Pts',(15.6744745567077,0.515018715252963,4.35732932085173));
#39868=CARTESIAN_POINT('Ctrl Pts',(15.6903798353953,0.357545113131455,4.47569155781202));
#39869=CARTESIAN_POINT('Ctrl Pts',(15.700638086511,0.255981111243369,4.55203033647815));
#39870=CARTESIAN_POINT('Ctrl Pts',(15.7108963376268,0.127540214881222,4.59261107697802));
#39871=CARTESIAN_POINT('Ctrl Pts',(15.7211545887425,-0.000419917270904514,
4.59344262983929));
#39872=CARTESIAN_POINT('Origin',(4.,0.,4.));
#39873=CARTESIAN_POINT('',(16.1288454112575,0.000520203518568921,4.59435747030618));
#39874=CARTESIAN_POINT('',(16.0211545887425,-0.00024144267326323,4.59496181546483));
#39875=CARTESIAN_POINT('',(4.,-7.27562663373442E-17,4.5941));
#39876=CARTESIAN_POINT('Ctrl Pts',(16.1288454112575,0.000520203518568921,
4.59435747030618));
#39877=CARTESIAN_POINT('Ctrl Pts',(16.1258245912393,0.0380542554257849,
4.59470210862833));
#39878=CARTESIAN_POINT('Ctrl Pts',(16.122803771221,0.0755288363057283,4.59145263304759));
#39879=CARTESIAN_POINT('Ctrl Pts',(16.1197829512027,0.112271568866026,4.58439375503351));
#39880=CARTESIAN_POINT('Ctrl Pts',(16.1038776725151,0.305730099191281,4.54722721702202));
#39881=CARTESIAN_POINT('Ctrl Pts',(16.0879723938275,0.478899942385972,4.40445440507416));
#39882=CARTESIAN_POINT('Ctrl Pts',(16.0720671151398,0.55226883266698,4.22163055421683));
#39883=CARTESIAN_POINT('Ctrl Pts',(16.0561618364522,0.625637722947984,4.03880670335952));
#39884=CARTESIAN_POINT('Ctrl Pts',(16.0402565577646,0.599205660315318,3.81593181359275));
#39885=CARTESIAN_POINT('Ctrl Pts',(16.024351279077,0.485109129681553,3.65534060523843));
#39886=CARTESIAN_POINT('Ctrl Pts',(16.0084460003894,0.371012599047788,3.4947493968841));
#39887=CARTESIAN_POINT('Ctrl Pts',(15.9925407217018,0.169251600412921,3.39644186994223));
#39888=CARTESIAN_POINT('Ctrl Pts',(15.9766354430142,-0.0275337514538456,
3.40555668173602));
#39889=CARTESIAN_POINT('Ctrl Pts',(15.9607301643265,-0.224319103320618,
3.41467149352982));
#39890=CARTESIAN_POINT('Ctrl Pts',(15.9448248856389,-0.416128808419276,
3.53120864405929));
#39891=CARTESIAN_POINT('Ctrl Pts',(15.9289196069513,-0.514891964967956,
3.70165920408156));
#39892=CARTESIAN_POINT('Ctrl Pts',(15.9130143282637,-0.613655121516638,
3.87210976410384));
#39893=CARTESIAN_POINT('Ctrl Pts',(15.8971090495761,-0.619371729515322,
4.09647373361892));
#39894=CARTESIAN_POINT('Ctrl Pts',(15.8812037708885,-0.52941696442075,4.27173266988224));
#39895=CARTESIAN_POINT('Ctrl Pts',(15.8652984922009,-0.439462199326184,
4.44699160614554));
#39896=CARTESIAN_POINT('Ctrl Pts',(15.8493932135132,-0.25383606113837,4.57314550915708));
#39897=CARTESIAN_POINT('Ctrl Pts',(15.8334879348256,-0.0577702193188812,
4.59226984378546));
#39898=CARTESIAN_POINT('Ctrl Pts',(15.8319404269696,-0.0386939468137543,
4.59413055045147));
#39899=CARTESIAN_POINT('Ctrl Pts',(15.8303929191136,-0.0195188482833839,
4.59497807636063));
#39900=CARTESIAN_POINT('Ctrl Pts',(15.8288454112575,-0.000332254705457391,
4.59484959654372));
#39901=CARTESIAN_POINT('Ctrl Pts',(15.7211545887425,-0.000419917270904514,
4.59344262983929));
#39902=CARTESIAN_POINT('Ctrl Pts',(15.7268016163144,-0.0708602278282204,
4.59390038836772));
#39903=CARTESIAN_POINT('Ctrl Pts',(15.7324486438863,-0.141154849878182,
4.58231274148771));
#39904=CARTESIAN_POINT('Ctrl Pts',(15.7380956714582,-0.206740066761224,
4.55801389847688));
#39905=CARTESIAN_POINT('Ctrl Pts',(15.7540009501458,-0.391465772281827,
4.48957437609924));
#39906=CARTESIAN_POINT('Ctrl Pts',(15.7699062288334,-0.538831311072463,
4.32029570526172));
#39907=CARTESIAN_POINT('Ctrl Pts',(15.785811507521,-0.58117266224226,4.12790349002296));
#39908=CARTESIAN_POINT('Ctrl Pts',(15.8017167862086,-0.62351401341206,3.93551127478418));
#39909=CARTESIAN_POINT('Ctrl Pts',(15.8176220648962,-0.560831176961022,
3.72000551514415));
#39910=CARTESIAN_POINT('Ctrl Pts',(15.8335273435838,-0.421905459495345,
3.58033733863277));
#39911=CARTESIAN_POINT('Ctrl Pts',(15.8494326222715,-0.282979742029676,
3.44066916212139));
#39912=CARTESIAN_POINT('Ctrl Pts',(15.8653379009591,-0.0678111435493865,
3.37683856873865));
#39913=CARTESIAN_POINT('Ctrl Pts',(15.8812431796467,0.124804018556085,3.41815386651619));
#39914=CARTESIAN_POINT('Ctrl Pts',(15.8971484583343,0.317419180661557,3.45946916429373));
#39915=CARTESIAN_POINT('Ctrl Pts',(15.9130537370219,0.487480906392202,3.60593035323155));
#39916=CARTESIAN_POINT('Ctrl Pts',(15.9289590157095,0.556904046010802,3.79028865163133));
#39917=CARTESIAN_POINT('Ctrl Pts',(15.9448642943971,0.6263271856294,3.9746469500311));
#39918=CARTESIAN_POINT('Ctrl Pts',(15.9607695730847,0.595111739135951,4.19690235789283));
#39919=CARTESIAN_POINT('Ctrl Pts',(15.9766748517723,0.477590518943614,4.35500459477727));
#39920=CARTESIAN_POINT('Ctrl Pts',(15.9915014307624,0.368039615220995,4.50238430120742));
#39921=CARTESIAN_POINT('Ctrl Pts',(16.0063280097524,0.18349252241573,4.59401752470064));
#39922=CARTESIAN_POINT('Ctrl Pts',(16.0211545887425,-0.00024144267326323,
4.59496181546483));
#39923=CARTESIAN_POINT('Origin',(4.,0.,4.));
#39924=CARTESIAN_POINT('',(16.4288454112575,7.48704377684928E-5,4.59312461313858));
#39925=CARTESIAN_POINT('',(16.3211545887425,0.000543344619121817,4.59417988242975));
#39926=CARTESIAN_POINT('',(4.,-7.27562663373442E-17,4.5941));
#39927=CARTESIAN_POINT('Ctrl Pts',(16.4288454112575,7.48704377684928E-5,
4.59312461313858));
#39928=CARTESIAN_POINT('Ctrl Pts',(16.4212562633649,0.0948679978941589,
4.5932308806522));
#39929=CARTESIAN_POINT('Ctrl Pts',(16.4136671154723,0.189615837117123,4.57184094704105));
#39930=CARTESIAN_POINT('Ctrl Pts',(16.4060779675797,0.273126642574496,4.52869916135151));
#39931=CARTESIAN_POINT('Ctrl Pts',(16.3901726888921,0.448147956300534,4.43828293357696));
#39932=CARTESIAN_POINT('Ctrl Pts',(16.3742674102045,0.573812330828296,4.25232504748949));
#39933=CARTESIAN_POINT('Ctrl Pts',(16.3583621315169,0.592420001795879,4.05620949715111));
#39934=CARTESIAN_POINT('Ctrl Pts',(16.3424568528292,0.611027672763462,3.86009394681272));
#39935=CARTESIAN_POINT('Ctrl Pts',(16.3265515741416,0.522578640170867,3.6538207322234));
#39936=CARTESIAN_POINT('Ctrl Pts',(16.310646295454,0.367684957814641,3.53210178682255));
#39937=CARTESIAN_POINT('Ctrl Pts',(16.2947410167664,0.212791275458425,3.4103828414217));
#39938=CARTESIAN_POINT('Ctrl Pts',(16.2788357380788,-0.00854705666138705,
3.3732181652093));
#39939=CARTESIAN_POINT('Ctrl Pts',(16.2629304593912,-0.19470084048803,3.43767220519428));
#39940=CARTESIAN_POINT('Ctrl Pts',(16.2470251807036,-0.380854624314662,
3.50212624517926));
#39941=CARTESIAN_POINT('Ctrl Pts',(16.231119902016,-0.531823859848111,3.66819900136163));
#39942=CARTESIAN_POINT('Ctrl Pts',(16.2152146233283,-0.578289861113055,
3.85963689006134));
#39943=CARTESIAN_POINT('Ctrl Pts',(16.1993093446407,-0.624755862378002,
4.05107477876107));
#39944=CARTESIAN_POINT('Ctrl Pts',(16.1834040659531,-0.566718629374431,
4.26787779997815));
#39945=CARTESIAN_POINT('Ctrl Pts',(16.1674987872655,-0.430826404144746,
4.41049917854914));
#39946=CARTESIAN_POINT('Ctrl Pts',(16.1546143285962,-0.320743594918802,
4.52603310245269));
#39947=CARTESIAN_POINT('Ctrl Pts',(16.1417298699269,-0.159570744489656,
4.592887512417));
#39948=CARTESIAN_POINT('Ctrl Pts',(16.1288454112575,0.000520203518568921,
4.59435747030618));
#39949=CARTESIAN_POINT('Ctrl Pts',(16.0211545887425,-0.00024144267326323,
4.59496181546483));
#39950=CARTESIAN_POINT('Ctrl Pts',(16.0222332884401,-0.0136089074611732,
4.59503051682625));
#39951=CARTESIAN_POINT('Ctrl Pts',(16.0233119881376,-0.0269720681925484,
4.59461918253551));
#39952=CARTESIAN_POINT('Ctrl Pts',(16.0243906878352,-0.0403017303441999,
4.59371435609144));
#39953=CARTESIAN_POINT('Ctrl Pts',(16.0402959665228,-0.236845765548457,
4.58037281461397));
#39954=CARTESIAN_POINT('Ctrl Pts',(16.0562012452104,-0.426106842065734,
4.45974066575184));
#39955=CARTESIAN_POINT('Ctrl Pts',(16.072106523898,-0.521184280535122,4.2872070887372));
#39956=CARTESIAN_POINT('Ctrl Pts',(16.0880118025856,-0.616261719004504,
4.11467351172257));
#39957=CARTESIAN_POINT('Ctrl Pts',(16.1039170812732,-0.61715551942601,3.89023850655542));
#39958=CARTESIAN_POINT('Ctrl Pts',(16.1198223599609,-0.523455286459661,
3.71695313254649));
#39959=CARTESIAN_POINT('Ctrl Pts',(16.1357276386485,-0.429755053493313,
3.54366775853756));
#39960=CARTESIAN_POINT('Ctrl Pts',(16.1516329173361,-0.241460787139106,
3.42153201568684));
#39961=CARTESIAN_POINT('Ctrl Pts',(16.1675381960237,-0.045029248433429,
3.40662546997421));
#39962=CARTESIAN_POINT('Ctrl Pts',(16.1834434747113,0.151402290272254,3.39171892426158));
#39963=CARTESIAN_POINT('Ctrl Pts',(16.1993487533989,0.355971101329402,3.48404157568705));
#39964=CARTESIAN_POINT('Ctrl Pts',(16.2152540320865,0.474747841293266,3.64120276856532));
#39965=CARTESIAN_POINT('Ctrl Pts',(16.2311593107741,0.593524581257127,3.79836396144359));
#39966=CARTESIAN_POINT('Ctrl Pts',(16.2470645894618,0.626509250127697,4.02036369577466));
#39967=CARTESIAN_POINT('Ctrl Pts',(16.2629698681494,0.558556683425868,4.20526908558792));
#39968=CARTESIAN_POINT('Ctrl Pts',(16.278875146837,0.490604116724039,4.39017447540119));
#39969=CARTESIAN_POINT('Ctrl Pts',(16.2947804255246,0.32171431444981,4.53798552069667));
#39970=CARTESIAN_POINT('Ctrl Pts',(16.3106857042122,0.129434328669215,4.58083364284428));
#39971=CARTESIAN_POINT('Ctrl Pts',(16.314175332389,0.0872479785030607,4.5902345478711));
#39972=CARTESIAN_POINT('Ctrl Pts',(16.3176649605657,0.0439357035691123,
4.5945828907904));
#39973=CARTESIAN_POINT('Ctrl Pts',(16.3211545887425,0.000543344619121817,
4.59417988242975));
#39974=CARTESIAN_POINT('Origin',(4.,0.,4.));
#39975=CARTESIAN_POINT('',(16.7288454112575,-0.000548108868865471,4.59408180714414));
#39976=CARTESIAN_POINT('',(16.6211545887425,-2.1752937549985E-5,4.5931168278739));
#39977=CARTESIAN_POINT('',(4.,-7.27562663373442E-17,4.5941));
#39978=CARTESIAN_POINT('Ctrl Pts',(16.7288454112575,-0.000548108868865471,
4.59408180714414));
#39979=CARTESIAN_POINT('Ctrl Pts',(16.7166879354906,0.15068989439403,4.59268722311157));
#39980=CARTESIAN_POINT('Ctrl Pts',(16.7045304597237,0.302891836883802,4.53390177381835));
#39981=CARTESIAN_POINT('Ctrl Pts',(16.6923729839567,0.411632901649024,4.42974331917764));
#39982=CARTESIAN_POINT('Ctrl Pts',(16.6764677052691,0.553895734249677,4.29347578465895));
#39983=CARTESIAN_POINT('Ctrl Pts',(16.6605624265815,0.621772048174623,4.07954898308531));
#39984=CARTESIAN_POINT('Ctrl Pts',(16.6446571478939,0.58409591167956,3.88618905124272));
#39985=CARTESIAN_POINT('Ctrl Pts',(16.6287518692063,0.546419775184499,3.69282911940014));
#39986=CARTESIAN_POINT('Ctrl Pts',(16.6128465905187,0.403191188269443,3.52003605728863));
#39987=CARTESIAN_POINT('Ctrl Pts',(16.596941311831,0.220174658543969,3.44714912875817));
#39988=CARTESIAN_POINT('Ctrl Pts',(16.5810360331434,0.0371581288184754,
3.37426220022769));
#39989=CARTESIAN_POINT('Ctrl Pts',(16.5651307544558,-0.185646343717467,
3.40128140527831));
#39990=CARTESIAN_POINT('Ctrl Pts',(16.5492254757682,-0.34593637135519,3.51580066803907));
#39991=CARTESIAN_POINT('Ctrl Pts',(16.5333201970806,-0.506226398992903,
3.63031993079982));
#39992=CARTESIAN_POINT('Ctrl Pts',(16.517414918393,-0.604001981732426,3.83233925127069));
#39993=CARTESIAN_POINT('Ctrl Pts',(16.5015096397054,-0.594368708523554,
4.02909990422408));
#39994=CARTESIAN_POINT('Ctrl Pts',(16.4856043610178,-0.584735435314682,
4.22586055717748));
#39995=CARTESIAN_POINT('Ctrl Pts',(16.4696990823301,-0.467693306157413,
4.4173625426134));
#39996=CARTESIAN_POINT('Ctrl Pts',(16.4537938036425,-0.296983115116624,
4.51567625060054));
#39997=CARTESIAN_POINT('Ctrl Pts',(16.4454776728475,-0.20772669247752,4.56707991793767));
#39998=CARTESIAN_POINT('Ctrl Pts',(16.4371615420525,-0.103798720846626,
4.59300816600183));
#39999=CARTESIAN_POINT('Ctrl Pts',(16.4288454112575,7.48704377684928E-5,
4.59312461313858));
#40000=CARTESIAN_POINT('Ctrl Pts',(16.3211545887425,0.000543344619121817,
4.59417988242975));
#40001=CARTESIAN_POINT('Ctrl Pts',(16.3335702392533,-0.153841115924154,
4.59274603025257));
#40002=CARTESIAN_POINT('Ctrl Pts',(16.3459858897642,-0.309239316255332,
4.53116741914846));
#40003=CARTESIAN_POINT('Ctrl Pts',(16.3584015402751,-0.418549561707542,
4.42300972860235));
#40004=CARTESIAN_POINT('Ctrl Pts',(16.3743068189627,-0.558583297016706,
4.28445249321304));
#40005=CARTESIAN_POINT('Ctrl Pts',(16.3902120976503,-0.622980598348072,
4.06945282343469));
#40006=CARTESIAN_POINT('Ctrl Pts',(16.4061173763379,-0.582172949355422,
3.87672947174358));
#40007=CARTESIAN_POINT('Ctrl Pts',(16.4220226550255,-0.541365300362771,
3.68400612005246));
#40008=CARTESIAN_POINT('Ctrl Pts',(16.4379279337131,-0.395352701046104,
3.5135590864486));
#40009=CARTESIAN_POINT('Ctrl Pts',(16.4538332124007,-0.211177959727979,
3.44365043774355));
#40010=CARTESIAN_POINT('Ctrl Pts',(16.4697384910883,-0.0270032184098532,
3.37374178903851));
#40011=CARTESIAN_POINT('Ctrl Pts',(16.485643769776,0.195333664909731,3.40437152523229));
#40012=CARTESIAN_POINT('Ctrl Pts',(16.5015490484636,0.353744999708243,3.52147576730199));
#40013=CARTESIAN_POINT('Ctrl Pts',(16.5174543271512,0.512156334506764,3.63858000937169));
#40014=CARTESIAN_POINT('Ctrl Pts',(16.5333596058388,0.606642120784206,3.84215875731731));
#40015=CARTESIAN_POINT('Ctrl Pts',(16.5492648845264,0.59381848284593,4.03873726278877));
#40016=CARTESIAN_POINT('Ctrl Pts',(16.565170163214,0.580994844907655,4.23531576826023));
#40017=CARTESIAN_POINT('Ctrl Pts',(16.5810754419016,0.460861782753675,4.42489403125753));
#40018=CARTESIAN_POINT('Ctrl Pts',(16.5969807205892,0.288579316114369,4.52042573380721));
#40019=CARTESIAN_POINT('Ctrl Pts',(16.6050386766403,0.201297315476928,4.56882414767653));
#40020=CARTESIAN_POINT('Ctrl Pts',(16.6130966326914,0.100630370301649,4.59308406930439));
#40021=CARTESIAN_POINT('Ctrl Pts',(16.6211545887425,-2.1752937549985E-5,
4.5931168278739));
#40022=CARTESIAN_POINT('Origin',(4.,0.,4.));
#40023=CARTESIAN_POINT('',(17.0288454112575,0.000186802344652959,4.59500977980842));
#40024=CARTESIAN_POINT('',(16.9211545887425,-0.000535257393875686,4.59425998651214));
#40025=CARTESIAN_POINT('',(4.,-7.27562663373442E-17,4.5941));
#40026=CARTESIAN_POINT('Ctrl Pts',(17.0288454112575,0.000186802344652959,
4.59500977980842));
#40027=CARTESIAN_POINT('Ctrl Pts',(17.0280248863039,0.0103527338555297,
4.59505157132578));
#40028=CARTESIAN_POINT('Ctrl Pts',(17.0272043613502,0.0205166685362397,
4.5948136789481));
#40029=CARTESIAN_POINT('Ctrl Pts',(17.0263838363966,0.0306658549750798,
4.59428997251885));
#40030=CARTESIAN_POINT('Ctrl Pts',(17.010478557709,0.227400443050786,4.58413830477164));
#40031=CARTESIAN_POINT('Ctrl Pts',(16.9945732790214,0.418593379366704,4.46659200952389));
#40032=CARTESIAN_POINT('Ctrl Pts',(16.9786680003338,0.516456956272638,4.29562337257973));
#40033=CARTESIAN_POINT('Ctrl Pts',(16.9627627216462,0.614320533178566,4.12465473563558));
#40034=CARTESIAN_POINT('Ctrl Pts',(16.9468574429585,0.618854750674521,3.90026375699502));
#40035=CARTESIAN_POINT('Ctrl Pts',(16.9309521642709,0.527977687913284,3.72548128085037));
#40036=CARTESIAN_POINT('Ctrl Pts',(16.9150468855833,0.437100625152047,3.55069880470573));
#40037=CARTESIAN_POINT('Ctrl Pts',(16.8991416068957,0.25081228213362,3.42552483105699));
#40038=CARTESIAN_POINT('Ctrl Pts',(16.8832363282081,0.054648384762208,3.40743395292956));
#40039=CARTESIAN_POINT('Ctrl Pts',(16.8673310495205,-0.141515512609204,
3.38934307480212));
#40040=CARTESIAN_POINT('Ctrl Pts',(16.8514257708328,-0.347554964333599,
3.47833529219599));
#40041=CARTESIAN_POINT('Ctrl Pts',(16.8355204921452,-0.468865370989487,
3.63354914383413));
#40042=CARTESIAN_POINT('Ctrl Pts',(16.8196152134576,-0.590175777645383,
3.78876299547228));
#40043=CARTESIAN_POINT('Ctrl Pts',(16.80370993477,-0.62675713923276,4.01019848135471));
#40044=CARTESIAN_POINT('Ctrl Pts',(16.7878046560824,-0.561812842140477,
4.19618179452704));
#40045=CARTESIAN_POINT('Ctrl Pts',(16.7718993773948,-0.496868545048197,
4.38216510769936));
#40046=CARTESIAN_POINT('Ctrl Pts',(16.7559940987072,-0.330398589276266,
4.53269624816158));
#40047=CARTESIAN_POINT('Ctrl Pts',(16.7400888200196,-0.138838935752124,
4.57865768466082));
#40048=CARTESIAN_POINT('Ctrl Pts',(16.7363410170989,-0.0937012275068688,
4.58948769960953));
#40049=CARTESIAN_POINT('Ctrl Pts',(16.7325932141782,-0.0471704703862807,
4.59451171761327));
#40050=CARTESIAN_POINT('Ctrl Pts',(16.7288454112575,-0.000548108868865471,
4.59408180714414));
#40051=CARTESIAN_POINT('Ctrl Pts',(16.6211545887425,-2.1752937549985E-5,
4.5931168278739));
#40052=CARTESIAN_POINT('Ctrl Pts',(16.629001911379,-0.0980428491191961,
4.59314873014073));
#40053=CARTESIAN_POINT('Ctrl Pts',(16.6368492340155,-0.196049888122182,
4.57020350190738));
#40054=CARTESIAN_POINT('Ctrl Pts',(16.6446965566521,-0.281666676968544,
4.52419924569128));
#40055=CARTESIAN_POINT('Ctrl Pts',(16.6606018353397,-0.455198332287519,
4.43095591292362));
#40056=CARTESIAN_POINT('Ctrl Pts',(16.6765071140273,-0.577829771800838,
4.24298410528626));
#40057=CARTESIAN_POINT('Ctrl Pts',(16.6924123927149,-0.593253826592341,
4.0465925244149));
#40058=CARTESIAN_POINT('Ctrl Pts',(16.7083176714025,-0.608677881383846,
3.85020094354353));
#40059=CARTESIAN_POINT('Ctrl Pts',(16.7242229500901,-0.516894551453523,
3.64538958943816));
#40060=CARTESIAN_POINT('Ctrl Pts',(16.7401282287778,-0.360046858872914,
3.52619917105016));
#40061=CARTESIAN_POINT('Ctrl Pts',(16.7560335074654,-0.203199166292313,
3.40700875266216));
#40062=CARTESIAN_POINT('Ctrl Pts',(16.771938786153,0.0187128889385656,3.37343926999153));
#40063=CARTESIAN_POINT('Ctrl Pts',(16.7878440648406,0.203796679382533,3.44090440927292));
#40064=CARTESIAN_POINT('Ctrl Pts',(16.8037493435282,0.388880469826499,3.50836954855431));
#40065=CARTESIAN_POINT('Ctrl Pts',(16.8196546222158,0.537135995483554,3.67686930978772));
#40066=CARTESIAN_POINT('Ctrl Pts',(16.8355599009034,0.58049059114602,3.86903573125179));
#40067=CARTESIAN_POINT('Ctrl Pts',(16.851465179591,0.623845186808487,4.06120215271587));
#40068=CARTESIAN_POINT('Ctrl Pts',(16.8673704582787,0.562298852476364,4.2770352344106));
#40069=CARTESIAN_POINT('Ctrl Pts',(16.8832757369663,0.424111061064287,4.41743355636644));
#40070=CARTESIAN_POINT('Ctrl Pts',(16.8959020208917,0.314411738992559,4.5288876912157));
#40071=CARTESIAN_POINT('Ctrl Pts',(16.9085283048171,0.156414067554279,4.59280392009262));
#40072=CARTESIAN_POINT('Ctrl Pts',(16.9211545887425,-0.000535257393875686,
4.59425998651214));
#40073=CARTESIAN_POINT('Origin',(4.,0.,4.));
#40074=CARTESIAN_POINT('',(17.3288454112575,0.000452601584348983,4.59351524744837));
#40075=CARTESIAN_POINT('',(17.2211545887425,0.000283723793354941,4.5949151055343));
#40076=CARTESIAN_POINT('',(4.,-7.27562663373442E-17,4.5941));
#40077=CARTESIAN_POINT('Ctrl Pts',(17.3288454112575,0.000452601584348983,
4.59351524744837));
#40078=CARTESIAN_POINT('Ctrl Pts',(17.3234565584296,0.0676518012035294,
4.59398979695312));
#40079=CARTESIAN_POINT('Ctrl Pts',(17.3180677056016,0.134706745978521,4.58346365752876));
#40080=CARTESIAN_POINT('Ctrl Pts',(17.3126788527736,0.197661386620268,4.56129398922237));
#40081=CARTESIAN_POINT('Ctrl Pts',(17.296773574086,0.383472937993069,4.49585988588324));
#40082=CARTESIAN_POINT('Ctrl Pts',(17.2808682953984,0.533564938357213,4.32899388620009));
#40083=CARTESIAN_POINT('Ctrl Pts',(17.2649630167108,0.579021491014364,4.13731379770915));
#40084=CARTESIAN_POINT('Ctrl Pts',(17.2490577380232,0.624478043671518,3.94563370921821));
#40085=CARTESIAN_POINT('Ctrl Pts',(17.2331524593355,0.565299148621668,3.72913953191949));
#40086=CARTESIAN_POINT('Ctrl Pts',(17.2172471806479,0.428657250819126,3.58723623291525));
#40087=CARTESIAN_POINT('Ctrl Pts',(17.2013419019603,0.292015353016592,3.44533293391101));
#40088=CARTESIAN_POINT('Ctrl Pts',(17.1854366232727,0.0779104524613767,
3.37802051320125));
#40089=CARTESIAN_POINT('Ctrl Pts',(17.1695313445851,-0.115349538542919,
3.41620598662221));
#40090=CARTESIAN_POINT('Ctrl Pts',(17.1536260658975,-0.308609529547215,
3.45439146004317));
#40091=CARTESIAN_POINT('Ctrl Pts',(17.1377207872099,-0.48102461100059,3.59807482759486));
#40092=CARTESIAN_POINT('Ctrl Pts',(17.1218155085223,-0.553429071780215,
3.78128276563952));
#40093=CARTESIAN_POINT('Ctrl Pts',(17.1059102298347,-0.625833532559839,
3.96449070368418));
#40094=CARTESIAN_POINT('Ctrl Pts',(17.090004951147,-0.598227372665711,4.18722321222181));
#40095=CARTESIAN_POINT('Ctrl Pts',(17.0740996724594,-0.483286172800906,
4.34721094636728));
#40096=CARTESIAN_POINT('Ctrl Pts',(17.0590149187255,-0.374274584390508,
4.4989451987145));
#40097=CARTESIAN_POINT('Ctrl Pts',(17.0439301649915,-0.186706445247169,
4.59424147319602));
#40098=CARTESIAN_POINT('Ctrl Pts',(17.0288454112575,0.000186802344652959,
4.59500977980842));
#40099=CARTESIAN_POINT('Ctrl Pts',(16.9211545887425,-0.000535257393875686,
4.59425998651214));
#40100=CARTESIAN_POINT('Ctrl Pts',(16.9244335835047,-0.0412943609811605,
4.59463812105998));
#40101=CARTESIAN_POINT('Ctrl Pts',(16.9277125782669,-0.0819827620002526,
4.59080381827239));
#40102=CARTESIAN_POINT('Ctrl Pts',(16.9309915730291,-0.121736182180322,
4.58249572362891));
#40103=CARTESIAN_POINT('Ctrl Pts',(16.9468968517167,-0.31456638552074,4.54219600671859));
#40104=CARTESIAN_POINT('Ctrl Pts',(16.9628021304043,-0.485397543709551,
4.39663301068103));
#40105=CARTESIAN_POINT('Ctrl Pts',(16.978707409092,-0.555791216176751,4.21264310503418));
#40106=CARTESIAN_POINT('Ctrl Pts',(16.9946126877796,-0.626184888643955,
4.02865319938731));
#40107=CARTESIAN_POINT('Ctrl Pts',(17.0105179664672,-0.596141075389537,
3.80623638413113));
#40108=CARTESIAN_POINT('Ctrl Pts',(17.0264232451548,-0.479454624411006,
3.64751705115182));
#40109=CARTESIAN_POINT('Ctrl Pts',(17.0423285238424,-0.362768173432475,
3.48879771817251));
#40110=CARTESIAN_POINT('Ctrl Pts',(17.05823380253,-0.159439084729831,3.39377586747005));
#40111=CARTESIAN_POINT('Ctrl Pts',(17.0741390812176,0.0371725263090214,
3.40608151284405));
#40112=CARTESIAN_POINT('Ctrl Pts',(17.0900443599052,0.233784137347885,3.41838715821804));
#40113=CARTESIAN_POINT('Ctrl Pts',(17.1059496385929,0.423678270722955,3.5380202996685));
#40114=CARTESIAN_POINT('Ctrl Pts',(17.1218549172805,0.519663574146654,3.71005045990219));
#40115=CARTESIAN_POINT('Ctrl Pts',(17.1377601959681,0.615648877570348,3.88208062013586));
#40116=CARTESIAN_POINT('Ctrl Pts',(17.1536654746557,0.617725351042682,4.10650779915277));
#40117=CARTESIAN_POINT('Ctrl Pts',(17.1695707533433,0.524939565793509,4.28028453107927));
#40118=CARTESIAN_POINT('Ctrl Pts',(17.1854760320309,0.432153780544336,4.45406126300578));
#40119=CARTESIAN_POINT('Ctrl Pts',(17.2013813107185,0.244505736573655,4.5771875478419));
#40120=CARTESIAN_POINT('Ctrl Pts',(17.2172865894061,0.0481554769387473,
4.59312900463441));
#40121=CARTESIAN_POINT('Ctrl Pts',(17.2185759225182,0.0322386925622284,
4.59442127046022));
#40122=CARTESIAN_POINT('Ctrl Pts',(17.2198652556304,0.0162647237884017,
4.5950091984451));
#40123=CARTESIAN_POINT('Ctrl Pts',(17.2211545887425,0.000283723793354941,
4.5949151055343));
#40124=CARTESIAN_POINT('Origin',(4.,0.,4.));
#40125=CARTESIAN_POINT('',(17.6288454112575,-0.000376811216598938,4.5933658344624));
#40126=CARTESIAN_POINT('',(17.5211545887425,0.000390292690419375,4.59338796628294));
#40127=CARTESIAN_POINT('',(4.,-7.27562663373442E-17,4.5941));
#40128=CARTESIAN_POINT('Ctrl Pts',(17.6288454112575,-0.000376811216598938,
4.5933658344624));
#40129=CARTESIAN_POINT('Ctrl Pts',(17.6188882305552,0.123868145157646,4.5926473455414));
#40130=CARTESIAN_POINT('Ctrl Pts',(17.608931049853,0.248515939035854,4.55458993700248));
#40131=CARTESIAN_POINT('Ctrl Pts',(17.5989738691507,0.348483110949462,4.48236965854082));
#40132=CARTESIAN_POINT('Ctrl Pts',(17.5830685904631,0.508167440925656,4.36700731952407));
#40133=CARTESIAN_POINT('Ctrl Pts',(17.5671633117754,0.604877102606476,4.16447556457896));
#40134=CARTESIAN_POINT('Ctrl Pts',(17.5512580330878,0.594207110796467,3.96776840716434));
#40135=CARTESIAN_POINT('Ctrl Pts',(17.5353527544002,0.583537118986457,3.77106124974973));
#40136=CARTESIAN_POINT('Ctrl Pts',(17.5194474757126,0.465487473685617,3.58017868986561));
#40137=CARTESIAN_POINT('Ctrl Pts',(17.503542197025,0.294261577747463,3.48276592343564));
#40138=CARTESIAN_POINT('Ctrl Pts',(17.4876369183374,0.123035681809298,3.38535315700567));
#40139=CARTESIAN_POINT('Ctrl Pts',(17.4717316396498,-0.101366464766187,
3.38141018402985));
#40140=CARTESIAN_POINT('Ctrl Pts',(17.4558263609621,-0.275908889943427,
3.47274745088526));
#40141=CARTESIAN_POINT('Ctrl Pts',(17.4399210822745,-0.450451315120656,
3.56408471774066));
#40142=CARTESIAN_POINT('Ctrl Pts',(17.4240158035869,-0.575134018899647,
3.75070222442727));
#40143=CARTESIAN_POINT('Ctrl Pts',(17.4081105248993,-0.592707978595278,
3.94691310701022));
#40144=CARTESIAN_POINT('Ctrl Pts',(17.3922052462117,-0.610281938290908,
4.14312398959316));
#40145=CARTESIAN_POINT('Ctrl Pts',(17.3762999675241,-0.520747153903178,
4.34892824807245));
#40146=CARTESIAN_POINT('Ctrl Pts',(17.3603946888365,-0.365214210518585,
4.46982927381454));
#40147=CARTESIAN_POINT('Ctrl Pts',(17.3498782629768,-0.262377240481122,
4.54976793433994));
#40148=CARTESIAN_POINT('Ctrl Pts',(17.3393618371172,-0.130687628661636,
4.59258915708319));
#40149=CARTESIAN_POINT('Ctrl Pts',(17.3288454112575,0.000452601584348983,
4.59351524744837));
#40150=CARTESIAN_POINT('Ctrl Pts',(17.2211545887425,0.000283723793354941,
4.5949151055343));
#40151=CARTESIAN_POINT('Ctrl Pts',(17.235770534318,-0.18087770297476,4.59384846352355));
#40152=CARTESIAN_POINT('Ctrl Pts',(17.2503864798935,-0.362942684182573,
4.50513801271133));
#40153=CARTESIAN_POINT('Ctrl Pts',(17.265002425469,-0.47285052735612,4.36129398677095));
#40154=CARTESIAN_POINT('Ctrl Pts',(17.2809077041566,-0.592453796716944,
4.20476088336606));
#40155=CARTESIAN_POINT('Ctrl Pts',(17.2968129828442,-0.626607860139456,
3.98293804780737));
#40156=CARTESIAN_POINT('Ctrl Pts',(17.3127182615318,-0.559630616639302,
3.79767714163318));
#40157=CARTESIAN_POINT('Ctrl Pts',(17.3286235402194,-0.492653373139145,
3.61241623545897));
#40158=CARTESIAN_POINT('Ctrl Pts',(17.3445288189071,-0.324544822716309,
3.46371725866926));
#40159=CARTESIAN_POINT('Ctrl Pts',(17.3604340975947,-0.132493299638714,
3.41985649047097));
#40160=CARTESIAN_POINT('Ctrl Pts',(17.3763393762823,0.0595582234388708,
3.37599572227269));
#40161=CARTESIAN_POINT('Ctrl Pts',(17.3922446549699,0.275552719171213,3.43697316266583));
#40162=CARTESIAN_POINT('Ctrl Pts',(17.4081499336575,0.416314653091553,3.5747905507646));
#40163=CARTESIAN_POINT('Ctrl Pts',(17.4240552123451,0.557076587011893,3.71260793886338));
#40164=CARTESIAN_POINT('Ctrl Pts',(17.4399604910327,0.622605959120231,3.92726527466781));
#40165=CARTESIAN_POINT('Ctrl Pts',(17.4558657697203,0.582814454063527,4.12020099097945));
#40166=CARTESIAN_POINT('Ctrl Pts',(17.4717710484079,0.543022949006823,4.31313670729109));
#40167=CARTESIAN_POINT('Ctrl Pts',(17.4876763270955,0.397910566785078,4.48435080410994));
#40168=CARTESIAN_POINT('Ctrl Pts',(17.5035816057832,0.214106774115907,4.55522901164789));
#40169=CARTESIAN_POINT('Ctrl Pts',(17.5094392667696,0.146414762764002,4.58133232736073));
#40170=CARTESIAN_POINT('Ctrl Pts',(17.515296927756,0.073474912906076,4.59382676872096));
#40171=CARTESIAN_POINT('Ctrl Pts',(17.5211545887425,0.000390292690419375,
4.59338796628294));
#40172=CARTESIAN_POINT('Origin',(4.,0.,4.));
#40173=CARTESIAN_POINT('',(17.9288454112575,-0.000301159635511528,4.59489313984584));
#40174=CARTESIAN_POINT('',(17.8211545887425,-0.000441626631060947,4.59348913571676));
#40175=CARTESIAN_POINT('',(4.,-7.27562663373442E-17,4.5941));
#40176=CARTESIAN_POINT('Ctrl Pts',(17.9288454112575,-0.000301159635511528,
4.59489313984584));
#40177=CARTESIAN_POINT('Ctrl Pts',(17.9143199026809,0.179756887528332,4.59377956832623));
#40178=CARTESIAN_POINT('Ctrl Pts',(17.8997943941043,0.360751589755073,4.50630604003092));
#40179=CARTESIAN_POINT('Ctrl Pts',(17.8852688855277,0.470789914960854,4.36397502945801));
#40180=CARTESIAN_POINT('Ctrl Pts',(17.8693636068401,0.591280720462369,4.20812407407766));
#40181=CARTESIAN_POINT('Ctrl Pts',(17.8534583281524,0.626694694978596,3.98649889312445));
#40182=CARTESIAN_POINT('Ctrl Pts',(17.8375530494648,0.560771239653389,3.80086039350393));
#40183=CARTESIAN_POINT('Ctrl Pts',(17.8216477707772,0.494847784328189,3.61522189388343));
#40184=CARTESIAN_POINT('Ctrl Pts',(17.8057424920896,0.327586899161578,3.46557007559562));
#40185=CARTESIAN_POINT('Ctrl Pts',(17.789837213402,0.135787706397568,3.42061872235194));
#40186=CARTESIAN_POINT('Ctrl Pts',(17.7739319347144,-0.0560114863664412,
3.37566736910827));
#40187=CARTESIAN_POINT('Ctrl Pts',(17.7580266560268,-0.272348986727849,
3.43541648090873));
#40188=CARTESIAN_POINT('Ctrl Pts',(17.7421213773392,-0.41389176700556,3.57243179339102));
#40189=CARTESIAN_POINT('Ctrl Pts',(17.7262160986515,-0.555434547283271,
3.7094471058733));
#40190=CARTESIAN_POINT('Ctrl Pts',(17.710310819964,-0.622182607477285,3.92372861903742));
#40191=CARTESIAN_POINT('Ctrl Pts',(17.6944055412763,-0.583488062224059,
4.11688732754162));
#40192=CARTESIAN_POINT('Ctrl Pts',(17.6785002625887,-0.544793516970831,
4.31004603604583));
#40193=CARTESIAN_POINT('Ctrl Pts',(17.6625949839011,-0.400656366270352,
4.48208193989012));
#40194=CARTESIAN_POINT('Ctrl Pts',(17.6466897052135,-0.217258291784321,
4.55400343026805));
#40195=CARTESIAN_POINT('Ctrl Pts',(17.6407416072282,-0.148672903323923,
4.58089991415997));
#40196=CARTESIAN_POINT('Ctrl Pts',(17.6347935092429,-0.0745967331795002,
4.59379503652584));
#40197=CARTESIAN_POINT('Ctrl Pts',(17.6288454112575,-0.000376811216598938,
4.5933658344624));
#40198=CARTESIAN_POINT('Ctrl Pts',(17.5211545887425,0.000390292690419375,
4.59338796628294));
#40199=CARTESIAN_POINT('Ctrl Pts',(17.5312022064437,-0.12497140465997,4.59263529057266));
#40200=CARTESIAN_POINT('Ctrl Pts',(17.5412498241448,-0.250759050797478,
4.55382993891589));
#40201=CARTESIAN_POINT('Ctrl Pts',(17.551297441846,-0.351218450958555,4.48038168762358));
#40202=CARTESIAN_POINT('Ctrl Pts',(17.5672027205336,-0.510244680247213,
4.36411383780432));
#40203=CARTESIAN_POINT('Ctrl Pts',(17.5831079992212,-0.605801935707933,
4.16103581990878));
#40204=CARTESIAN_POINT('Ctrl Pts',(17.5990132779088,-0.594014368327242,
3.96439246823218));
#40205=CARTESIAN_POINT('Ctrl Pts',(17.6149185565964,-0.58222680094655,3.76774911655557));
#40206=CARTESIAN_POINT('Ctrl Pts',(17.6308238352841,-0.463094410724447,
3.5775404310979));
#40207=CARTESIAN_POINT('Ctrl Pts',(17.6467291139717,-0.291317751175132,
3.48110219315546));
#40208=CARTESIAN_POINT('Ctrl Pts',(17.6626343926593,-0.119541091625818,
3.38466395521302));
#40209=CARTESIAN_POINT('Ctrl Pts',(17.6785396713469,0.104879837250709,3.38199616478582));
#40210=CARTESIAN_POINT('Ctrl Pts',(17.6944449500345,0.278900439380867,3.47432375837312));
#40211=CARTESIAN_POINT('Ctrl Pts',(17.7103502287221,0.452921041511034,3.56665135196042));
#40212=CARTESIAN_POINT('Ctrl Pts',(17.7262555074097,0.576541316894826,3.75397432956222));
#40213=CARTESIAN_POINT('Ctrl Pts',(17.7421607860974,0.593000065018554,3.95028190484542));
#40214=CARTESIAN_POINT('Ctrl Pts',(17.758066064785,0.60945881314228,4.1465894801286));
#40215=CARTESIAN_POINT('Ctrl Pts',(17.7739713434726,0.518756034005955,4.35188165309317));
#40216=CARTESIAN_POINT('Ctrl Pts',(17.7898766221602,0.362538606470845,4.47189694310939));
#40217=CARTESIAN_POINT('Ctrl Pts',(17.8003026110209,0.260137309937395,4.55056755941266));
#40218=CARTESIAN_POINT('Ctrl Pts',(17.8107285998817,0.129585238016204,4.59259583028147));
#40219=CARTESIAN_POINT('Ctrl Pts',(17.8211545887425,-0.000441626631060947,
4.59348913571676));
#40220=CARTESIAN_POINT('Origin',(4.,0.,4.));
#40221=CARTESIAN_POINT('',(18.2288454112575,0.000530626821107938,4.59429426521737));
#40222=CARTESIAN_POINT('',(18.1211545887425,-0.000206261771334874,4.59499421029555));
#40223=CARTESIAN_POINT('',(4.,-7.27562663373442E-17,4.5941));
#40224=CARTESIAN_POINT('Ctrl Pts',(18.2288454112575,0.000530626821107938,
4.59429426521737));
#40225=CARTESIAN_POINT('Ctrl Pts',(18.2256568534942,0.0401596894680921,
4.59466101186164));
#40226=CARTESIAN_POINT('Ctrl Pts',(18.2224682957309,0.0797220295111884,
4.5910372210354));
#40227=CARTESIAN_POINT('Ctrl Pts',(18.2192797379675,0.118424305077702,4.58317806034235));
#40228=CARTESIAN_POINT('Ctrl Pts',(18.2033744592799,0.311480390123117,4.54397471188459));
#40229=CARTESIAN_POINT('Ctrl Pts',(18.1874691805923,0.483135922039688,4.39938477867344));
#40230=CARTESIAN_POINT('Ctrl Pts',(18.1715639019047,0.554573942717995,4.21579784094385));
#40231=CARTESIAN_POINT('Ctrl Pts',(18.1556586232171,0.626011963396302,4.03221090321426));
#40232=CARTESIAN_POINT('Ctrl Pts',(18.1397533445295,0.597232472836345,3.80962696096622));
#40233=CARTESIAN_POINT('Ctrl Pts',(18.1238480658419,0.481449795543417,3.65024714373002));
#40234=CARTESIAN_POINT('Ctrl Pts',(18.1079427871543,0.365667118250483,3.49086732649381));
#40235=CARTESIAN_POINT('Ctrl Pts',(18.0920375084667,0.16288125422457,3.39469163426944));
#40236=CARTESIAN_POINT('Ctrl Pts',(18.076132229779,-0.0337971069360236,
3.40587987606835));
#40237=CARTESIAN_POINT('Ctrl Pts',(18.0602269510914,-0.230475468096606,
3.41706811786726));
#40238=CARTESIAN_POINT('Ctrl Pts',(18.0443216724038,-0.421046326391869,
3.53562029368944));
#40239=CARTESIAN_POINT('Ctrl Pts',(18.0284163937162,-0.518007606080761,
3.70710225992629));
#40240=CARTESIAN_POINT('Ctrl Pts',(18.0125111150286,-0.614968885769652,
3.87858422616314));
#40241=CARTESIAN_POINT('Ctrl Pts',(17.996605836341,-0.618320586852172,4.10299598281466));
#40242=CARTESIAN_POINT('Ctrl Pts',(17.9807005576534,-0.526523749990007,
4.27729714530494));
#40243=CARTESIAN_POINT('Ctrl Pts',(17.9647952789658,-0.434726913127837,
4.45159830779523));
#40244=CARTESIAN_POINT('Ctrl Pts',(17.9488900002781,-0.247781538320971,
4.57578887612429));
#40245=CARTESIAN_POINT('Ctrl Pts',(17.9329847215905,-0.0515250326741526,
4.59284579538505));
#40246=CARTESIAN_POINT('Ctrl Pts',(17.9316049514795,-0.0344999389365885,
4.59432546938787));
#40247=CARTESIAN_POINT('Ctrl Pts',(17.9302251813685,-0.0174047750035579,
4.59499891739512));
#40248=CARTESIAN_POINT('Ctrl Pts',(17.9288454112575,-0.000301159635511528,
4.59489313984584));
#40249=CARTESIAN_POINT('Ctrl Pts',(17.8211545887425,-0.000441626631060947,
4.59348913571676));
#40250=CARTESIAN_POINT('Ctrl Pts',(17.8266338785693,-0.0687761401428734,
4.59395860479535));
#40251=CARTESIAN_POINT('Ctrl Pts',(17.8321131683962,-0.136965594625977,
4.58306684864343));
#40252=CARTESIAN_POINT('Ctrl Pts',(17.837592458223,-0.200847632772524,4.56016175744822));
#40253=CARTESIAN_POINT('Ctrl Pts',(17.8534977369106,-0.386284368546891,
4.49367287470298));
#40254=CARTESIAN_POINT('Ctrl Pts',(17.8694030155983,-0.535425764161732,
4.32595670214462));
#40255=CARTESIAN_POINT('Ctrl Pts',(17.8853082942859,-0.579792400402821,
4.13402141072584));
#40256=CARTESIAN_POINT('Ctrl Pts',(17.9012135729735,-0.624159036643913,
3.94208611930704));
#40257=CARTESIAN_POINT('Ctrl Pts',(17.9171188516611,-0.563750913511241,
3.72593170902781));
#40258=CARTESIAN_POINT('Ctrl Pts',(17.9330241303487,-0.426304885490399,
3.58480714034942));
#40259=CARTESIAN_POINT('Ctrl Pts',(17.9489294090363,-0.288858857469565,
3.44368257167104));
#40260=CARTESIAN_POINT('Ctrl Pts',(17.9648346877239,-0.0743749245605683,
3.37758784459349));
#40261=CARTESIAN_POINT('Ctrl Pts',(17.9807399664116,0.118664965311668,3.41687086155347));
#40262=CARTESIAN_POINT('Ctrl Pts',(17.9966452450992,0.311704855183904,3.45615387851346));
#40263=CARTESIAN_POINT('Ctrl Pts',(18.0125505237868,0.483300702019379,3.60081463951098));
#40264=CARTESIAN_POINT('Ctrl Pts',(18.0284558024744,0.554662952572844,3.78443104318807));
#40265=CARTESIAN_POINT('Ctrl Pts',(18.044361081162,0.62602520312631,3.96804744686516));
#40266=CARTESIAN_POINT('Ctrl Pts',(18.0602663598496,0.597153857397765,4.19061949322182));
#40267=CARTESIAN_POINT('Ctrl Pts',(18.0761716385372,0.481305415899848,4.34995151481781));
#40268=CARTESIAN_POINT('Ctrl Pts',(18.0911659552723,0.372092100044007,4.50015792394613));
#40269=CARTESIAN_POINT('Ctrl Pts',(18.1061602720074,0.185579460002099,4.59416090236354));
#40270=CARTESIAN_POINT('Ctrl Pts',(18.1211545887425,-0.000206261771334874,
4.59499421029555));
#40271=CARTESIAN_POINT('Origin',(4.,0.,4.));
#40272=CARTESIAN_POINT('',(18.5288454112575,4.04073003155148E-5,4.59311858068669));
#40273=CARTESIAN_POINT('',(18.4211545887425,0.000547083855738422,4.59411609730493));
#40274=CARTESIAN_POINT('',(4.,-7.27562663373442E-17,4.5941));
#40275=CARTESIAN_POINT('Ctrl Pts',(18.5288454112575,4.04073003155148E-5,
4.59311858068669));
#40276=CARTESIAN_POINT('Ctrl Pts',(18.5210885256199,0.0969311390001333,
4.59317716754242));
#40277=CARTESIAN_POINT('Ctrl Pts',(18.5133316399822,0.193796352446061,4.57078374547556));
#40278=CARTESIAN_POINT('Ctrl Pts',(18.5055747543446,0.27868347559656,4.52579129559858));
#40279=CARTESIAN_POINT('Ctrl Pts',(18.489669475657,0.452742165355285,4.43353552600749));
#40280=CARTESIAN_POINT('Ctrl Pts',(18.4737641969693,0.576439736070726,4.24626358090446));
#40281=CARTESIAN_POINT('Ctrl Pts',(18.4578589182817,0.592979496483005,4.04996281465819));
#40282=CARTESIAN_POINT('Ctrl Pts',(18.4419536395941,0.609519256895283,3.85366204841193));
#40283=CARTESIAN_POINT('Ctrl Pts',(18.4260483609065,0.518901207004412,3.64833246102244));
#40284=CARTESIAN_POINT('Ctrl Pts',(18.4101430822189,0.362733321586741,3.52825271224048));
#40285=CARTESIAN_POINT('Ctrl Pts',(18.3942378035313,0.206565436169079,3.40817296345854));
#40286=CARTESIAN_POINT('Ctrl Pts',(18.3783325248437,-0.015152284775374,
3.37334305328413));
#40287=CARTESIAN_POINT('Ctrl Pts',(18.3624272461561,-0.200616443892158,
3.43975540293737));
#40288=CARTESIAN_POINT('Ctrl Pts',(18.3465219674685,-0.386080603008964,
3.50616775259061));
#40289=CARTESIAN_POINT('Ctrl Pts',(18.3306166887808,-0.535291200298091,
3.67382236207151));
#40290=CARTESIAN_POINT('Ctrl Pts',(18.3147114100932,-0.579737042064157,
3.86573932758804));
#40291=CARTESIAN_POINT('Ctrl Pts',(18.2988061314056,-0.624182883830224,
4.05765629310458));
#40292=CARTESIAN_POINT('Ctrl Pts',(18.282900852718,-0.563863970073232,4.27383561465674));
#40293=CARTESIAN_POINT('Ctrl Pts',(18.2669955740304,-0.426476194107598,
4.41501689358062));
#40294=CARTESIAN_POINT('Ctrl Pts',(18.2542788531061,-0.316630774880643,
4.52789532589669));
#40295=CARTESIAN_POINT('Ctrl Pts',(18.2415621321818,-0.157519428275204,
4.5928315930404));
#40296=CARTESIAN_POINT('Ctrl Pts',(18.2288454112575,0.000530626821107938,
4.59429426521737));
#40297=CARTESIAN_POINT('Ctrl Pts',(18.1211545887425,-0.000206261771334874,
4.59499421029555));
#40298=CARTESIAN_POINT('Ctrl Pts',(18.122065550695,-0.0114934532352288,
4.59504483693191));
#40299=CARTESIAN_POINT('Ctrl Pts',(18.1229765126475,-0.0227779616248223,
4.59475157188293));
#40300=CARTESIAN_POINT('Ctrl Pts',(18.1238874746001,-0.0340422900297544,
4.59410612569417));
#40301=CARTESIAN_POINT('Ctrl Pts',(18.1397927532877,-0.230716017194119,
4.58283671813918));
#40302=CARTESIAN_POINT('Ctrl Pts',(18.1556980319753,-0.421237934255556,
4.46420590619388));
#40303=CARTESIAN_POINT('Ctrl Pts',(18.1716033106629,-0.518128437217054,
4.29268393984778));
#40304=CARTESIAN_POINT('Ctrl Pts',(18.1875085893505,-0.615018940178556,
4.12116197350168));
#40305=CARTESIAN_POINT('Ctrl Pts',(18.2034138680381,-0.618278029040109,
3.89674885275477));
#40306=CARTESIAN_POINT('Ctrl Pts',(18.2193191467258,-0.526409268077163,
3.72248558851787));
#40307=CARTESIAN_POINT('Ctrl Pts',(18.2352244254134,-0.434540507114227,
3.54822232428098));
#40308=CARTESIAN_POINT('Ctrl Pts',(18.251129704101,-0.24754389632682,3.42410891655409));
#40309=CARTESIAN_POINT('Ctrl Pts',(18.2670349827886,-0.0512803682143169,
3.40713299136011));
#40310=CARTESIAN_POINT('Ctrl Pts',(18.2829402614762,0.144983159898198,3.39015706616613));
#40311=CARTESIAN_POINT('Ctrl Pts',(18.2988455401638,0.35051360533581,3.48031862350507));
#40312=CARTESIAN_POINT('Ctrl Pts',(18.3147508188514,0.470940082829639,3.63621929066782));
#40313=CARTESIAN_POINT('Ctrl Pts',(18.330656097539,0.591366560323475,3.79211995783059));
#40314=CARTESIAN_POINT('Ctrl Pts',(18.3465613762266,0.62668906987352,4.01375973481717));
#40315=CARTESIAN_POINT('Ctrl Pts',(18.3624666549143,0.560689009466533,4.199371012841));
#40316=CARTESIAN_POINT('Ctrl Pts',(18.3783719336019,0.49468894905955,4.38498229086483));
#40317=CARTESIAN_POINT('Ctrl Pts',(18.3942772122895,0.327366318695548,4.53456506992591));
#40318=CARTESIAN_POINT('Ctrl Pts',(18.4101824909771,0.135548591400956,4.57943726620491));
#40319=CARTESIAN_POINT('Ctrl Pts',(18.4138398568989,0.0914407431336166,
4.58975547846199));
#40320=CARTESIAN_POINT('Ctrl Pts',(18.4174972228207,0.0460377050408626,
4.59453706917327));
#40321=CARTESIAN_POINT('Ctrl Pts',(18.4211545887425,0.000547083855738422,
4.59411609730493));
#40322=CARTESIAN_POINT('Origin',(4.,0.,4.));
#40323=CARTESIAN_POINT('',(18.8288454112575,-0.000545657836941327,4.59414547262434));
#40324=CARTESIAN_POINT('',(18.7211545887425,-5.63168744233308E-5,4.59312091231189));
#40325=CARTESIAN_POINT('',(4.,-7.27562663373442E-17,4.5941));
#40326=CARTESIAN_POINT('Ctrl Pts',(18.8288454112575,-0.000545657836941327,
4.59414547262434));
#40327=CARTESIAN_POINT('Ctrl Pts',(18.8165201977456,0.15273698101805,4.59272393327212));
#40328=CARTESIAN_POINT('Ctrl Pts',(18.8041949842336,0.307016766534516,4.53213273669464));
#40329=CARTESIAN_POINT('Ctrl Pts',(18.7918697707216,0.416139138999065,4.42538122089617));
#40330=CARTESIAN_POINT('Ctrl Pts',(18.775964492034,0.556957936451544,4.28762193522949));
#40331=CARTESIAN_POINT('Ctrl Pts',(18.7600592133464,0.622575889387102,4.0729916608594));
#40332=CARTESIAN_POINT('Ctrl Pts',(18.7441539346588,0.582864009884755,3.88003953951897));
#40333=CARTESIAN_POINT('Ctrl Pts',(18.7282486559712,0.543152130382401,3.6870874181785));
#40334=CARTESIAN_POINT('Ctrl Pts',(18.7123433772835,0.3981104184421,3.51581344986768));
#40335=CARTESIAN_POINT('Ctrl Pts',(18.6964380985959,0.214335891977863,3.44485939483061));
#40336=CARTESIAN_POINT('Ctrl Pts',(18.6805328199083,0.0305613655136472,
3.37390533979354));
#40337=CARTESIAN_POINT('Ctrl Pts',(18.6646275412207,-0.191945975474496,
3.40327119803019));
#40338=CARTESIAN_POINT('Ctrl Pts',(18.6487222625331,-0.351020173514001,
3.51947340980541));
#40339=CARTESIAN_POINT('Ctrl Pts',(18.6328169838455,-0.510094371553506,
3.63567562158063));
#40340=CARTESIAN_POINT('Ctrl Pts',(18.6169117051579,-0.605735426644373,
3.83871418689441));
#40341=CARTESIAN_POINT('Ctrl Pts',(18.6010064264702,-0.594029012528289,
4.03536238640794));
#40342=CARTESIAN_POINT('Ctrl Pts',(18.5851011477826,-0.582322598412206,
4.23201058592146));
#40343=CARTESIAN_POINT('Ctrl Pts',(18.569195869095,-0.463268715089173,4.42226841963472));
#40344=CARTESIAN_POINT('Ctrl Pts',(18.5532905904074,-0.29153186902666,4.51877753945177));
#40345=CARTESIAN_POINT('Ctrl Pts',(18.5451421973574,-0.203549800283198,
4.56821988225003));
#40346=CARTESIAN_POINT('Ctrl Pts',(18.5369938043075,-0.101740616897797,
4.59305703682098));
#40347=CARTESIAN_POINT('Ctrl Pts',(18.5288454112575,4.04073003155148E-5,
4.59311858068669));
#40348=CARTESIAN_POINT('Ctrl Pts',(18.4211545887425,0.000547083855738422,
4.59411609730493));
#40349=CARTESIAN_POINT('Ctrl Pts',(18.4334025015083,-0.151793472668411,
4.59270633223614));
#40350=CARTESIAN_POINT('Ctrl Pts',(18.4456504142741,-0.305116246576315,
4.53295143150856));
#40351=CARTESIAN_POINT('Ctrl Pts',(18.4578983270399,-0.414068183831284,
4.42739736222451));
#40352=CARTESIAN_POINT('Ctrl Pts',(18.4738036057275,-0.555554407543751,
4.29032364846819));
#40353=CARTESIAN_POINT('Ctrl Pts',(18.4897088844152,-0.622214030743504,
4.07601460745865));
#40354=CARTESIAN_POINT('Ctrl Pts',(18.5056141631028,-0.583439774593308,
3.88287188415962));
#40355=CARTESIAN_POINT('Ctrl Pts',(18.5215194417904,-0.54466551844311,3.68972916086059));
#40356=CARTESIAN_POINT('Ctrl Pts',(18.537424720478,-0.400457382942952,3.51775275527208));
#40357=CARTESIAN_POINT('Ctrl Pts',(18.5533299991656,-0.217029642971419,
3.44590695711865));
#40358=CARTESIAN_POINT('Ctrl Pts',(18.5692352778532,-0.0336019029998957,
3.37406115896522));
#40359=CARTESIAN_POINT('Ctrl Pts',(18.5851405565408,0.189045441442997,3.40234596824686));
#40360=CARTESIAN_POINT('Ctrl Pts',(18.6010458352284,0.348682149221421,3.51777419717301));
#40361=CARTESIAN_POINT('Ctrl Pts',(18.6169511139161,0.508318856999844,3.63320242609916));
#40362=CARTESIAN_POINT('Ctrl Pts',(18.6328563926037,0.604944928113798,3.83577407466982));
#40363=CARTESIAN_POINT('Ctrl Pts',(18.6487616712913,0.594193758619731,4.03247681196108));
#40364=CARTESIAN_POINT('Ctrl Pts',(18.6646669499789,0.583442589125664,4.22917954925235));
#40365=CARTESIAN_POINT('Ctrl Pts',(18.6805722286665,0.465314179023576,4.42001337526422));
#40366=CARTESIAN_POINT('Ctrl Pts',(18.6964775073541,0.294048096631404,4.51735547060535));
#40367=CARTESIAN_POINT('Ctrl Pts',(18.7047032011502,0.205474838715737,4.56769764225005));
#40368=CARTESIAN_POINT('Ctrl Pts',(18.7129288949463,0.102689258835563,4.59303430424318));
#40369=CARTESIAN_POINT('Ctrl Pts',(18.7211545887425,-5.63168744233308E-5,
4.59312091231189));
#40370=CARTESIAN_POINT('Origin',(4.,0.,4.));
#40371=CARTESIAN_POINT('',(19.1288454112575,0.000222628893785728,4.59497983522242));
#40372=CARTESIAN_POINT('',(19.0211545887425,-0.000526118841417405,4.59432346427954));
#40373=CARTESIAN_POINT('',(4.,-7.27562663373442E-17,4.5941));
#40374=CARTESIAN_POINT('Ctrl Pts',(19.1288454112575,0.000222628893785728,
4.59497983522242));
#40375=CARTESIAN_POINT('Ctrl Pts',(19.1278571485589,0.012468395078646,4.59503853204781));
#40376=CARTESIAN_POINT('Ctrl Pts',(19.1268688858602,0.0247107891953784,
4.59469333777414));
#40377=CARTESIAN_POINT('Ctrl Pts',(19.1258806231615,0.0369274203756033,
4.59393377720877));
#40378=CARTESIAN_POINT('Ctrl Pts',(19.1099753444739,0.233544093050454,4.58170927203582));
#40379=CARTESIAN_POINT('Ctrl Pts',(19.0940700657862,0.423487581379576,4.46215450773496));
#40380=CARTESIAN_POINT('Ctrl Pts',(19.0781647870986,0.519543871337238,4.29016397409385));
#40381=CARTESIAN_POINT('Ctrl Pts',(19.062259508411,0.615600161294901,4.11817344045274));
#40382=CARTESIAN_POINT('Ctrl Pts',(19.0463542297234,0.617769252881104,3.89374713747137));
#40383=CARTESIAN_POINT('Ctrl Pts',(19.0304489510358,0.525055191022736,3.71993212880311));
#40384=CARTESIAN_POINT('Ctrl Pts',(19.0145436723482,0.432341129164367,3.54611712013485));
#40385=CARTESIAN_POINT('Ctrl Pts',(18.9986383936606,0.244743913861428,3.42291340577968));
#40386=CARTESIAN_POINT('Ctrl Pts',(18.982733114973,0.0484002497885746,3.40689091904056));
#40387=CARTESIAN_POINT('Ctrl Pts',(18.9668278362853,-0.147943414284278,
3.39086843230144));
#40388=CARTESIAN_POINT('Ctrl Pts',(18.9509225575977,-0.353033527127044,
3.48202717317836));
#40389=CARTESIAN_POINT('Ctrl Pts',(18.9350172789101,-0.472701385564812,
3.63851090447403));
#40390=CARTESIAN_POINT('Ctrl Pts',(18.9191120002225,-0.592369244002587,
3.79499463576972));
#40391=CARTESIAN_POINT('Ctrl Pts',(18.9032067215349,-0.626614848035354,
4.01680335748416));
#40392=CARTESIAN_POINT('Ctrl Pts',(18.8873014428473,-0.559714065105754,
4.20209188855652));
#40393=CARTESIAN_POINT('Ctrl Pts',(18.8713961641597,-0.492813282176159,
4.38738041962887));
#40394=CARTESIAN_POINT('Ctrl Pts',(18.8554908854721,-0.324766112284209,
4.53614876005914));
#40395=CARTESIAN_POINT('Ctrl Pts',(18.8395856067844,-0.132732706353525,
4.58008878179264));
#40396=CARTESIAN_POINT('Ctrl Pts',(18.8360055416088,-0.0895085590353085,
4.5899790920924));
#40397=CARTESIAN_POINT('Ctrl Pts',(18.8324254764332,-0.0450691735440342,
4.59455838259347));
#40398=CARTESIAN_POINT('Ctrl Pts',(18.8288454112575,-0.000545657836941327,
4.59414547262434));
#40399=CARTESIAN_POINT('Ctrl Pts',(18.7211545887425,-5.63168744233308E-5,
4.59312091231189));
#40400=CARTESIAN_POINT('Ctrl Pts',(18.728834173634,-0.0959805501911411,
4.59320177041728));
#40401=CARTESIAN_POINT('Ctrl Pts',(18.7365137585255,-0.191869914813978,
4.57127401300463));
#40402=CARTESIAN_POINT('Ctrl Pts',(18.744193343417,-0.276126457005151,4.5271386400555));
#40403=CARTESIAN_POINT('Ctrl Pts',(18.7600986221046,-0.450631173567243,
4.43572934949413));
#40404=CARTESIAN_POINT('Ctrl Pts',(18.7760039007922,-0.575236852009173,
4.249060403701));
#40405=CARTESIAN_POINT('Ctrl Pts',(18.7919091794798,-0.592729836422094,
4.05284228527226));
#40406=CARTESIAN_POINT('Ctrl Pts',(18.8078144581674,-0.610222820835014,
3.85662416684351));
#40407=CARTESIAN_POINT('Ctrl Pts',(18.823719736855,-0.520603111218926,3.65085687577915));
#40408=CARTESIAN_POINT('Ctrl Pts',(18.8396250155426,-0.365020286731977,
3.53002004684018));
#40409=CARTESIAN_POINT('Ctrl Pts',(18.8555302942302,-0.209437462245028,
3.40918321790122));
#40410=CARTESIAN_POINT('Ctrl Pts',(18.8714355729179,0.0121084771127808,
3.37327685108765));
#40411=CARTESIAN_POINT('Ctrl Pts',(18.8873408516055,0.197893008823487,3.43878763096633));
#40412=CARTESIAN_POINT('Ctrl Pts',(18.9032461302931,0.383677540534204,3.50429841084501));
#40413=CARTESIAN_POINT('Ctrl Pts',(18.9191514089807,0.533700664597814,3.67122633741595));
#40414=CARTESIAN_POINT('Ctrl Pts',(18.9350566876683,0.579078109400399,3.86292516893752));
#40415=CARTESIAN_POINT('Ctrl Pts',(18.9509619663559,0.624455554202981,4.05462400045908));
#40416=CARTESIAN_POINT('Ctrl Pts',(18.9668672450435,0.56518731974455,4.27109373693126));
#40417=CARTESIAN_POINT('Ctrl Pts',(18.9827725237311,0.428486871854059,4.41294063344238));
#40418=CARTESIAN_POINT('Ctrl Pts',(18.9955665454016,0.318526617336051,4.52704063153052));
#40419=CARTESIAN_POINT('Ctrl Pts',(19.008360567072,0.158464569423419,4.5928566151945));
#40420=CARTESIAN_POINT('Ctrl Pts',(19.0211545887425,-0.000526118841417405,
4.59432346427954));
#40421=CARTESIAN_POINT('Origin',(4.,0.,4.));
#40422=CARTESIAN_POINT('',(19.4288454112575,0.000431836873498515,4.59346738712276));
#40423=CARTESIAN_POINT('',(19.3211545887425,0.000315695961457875,4.59487351203822));
#40424=CARTESIAN_POINT('',(4.,-7.27562663373442E-17,4.5941));
#40425=CARTESIAN_POINT('Ctrl Pts',(19.4288454112575,0.000431836873498515,
4.59346738712276));
#40426=CARTESIAN_POINT('Ctrl Pts',(19.4232888206845,0.0697367837969298,
4.59393182999066));
#40427=CARTESIAN_POINT('Ctrl Pts',(19.4177322301115,0.13889623855249,4.58272225272434));
#40428=CARTESIAN_POINT('Ctrl Pts',(19.4121756395385,0.203565929825556,4.55917964700716));
#40429=CARTESIAN_POINT('Ctrl Pts',(19.3962703608509,0.38867754617092,4.49179089484985));
#40430=CARTESIAN_POINT('Ctrl Pts',(19.3803650821633,0.537002597765565,4.32335233206236));
#40431=CARTESIAN_POINT('Ctrl Pts',(19.3644598034757,0.580436494614329,4.13120381907284));
#40432=CARTESIAN_POINT('Ctrl Pts',(19.3485545247881,0.623870391463095,3.93905530608331));
#40433=CARTESIAN_POINT('Ctrl Pts',(19.3326492461004,0.562413133565966,3.72319684289176));
#40434=CARTESIAN_POINT('Ctrl Pts',(19.3167439674128,0.424283294458304,3.58274150440131));
#40435=CARTESIAN_POINT('Ctrl Pts',(19.3008386887252,0.286153455350651,3.44228616591086));
#40436=CARTESIAN_POINT('Ctrl Pts',(19.2849334100376,0.071351035032473,3.37723395212151));
#40437=CARTESIAN_POINT('Ctrl Pts',(19.26902813135,-0.12149578302492,3.4174540870367));
#40438=CARTESIAN_POINT('Ctrl Pts',(19.2531228526624,-0.314342601082313,
3.45767422195189));
#40439=CARTESIAN_POINT('Ctrl Pts',(19.2372175739748,-0.485233816878921,
3.60316670557164));
#40440=CARTESIAN_POINT('Ctrl Pts',(19.2213122952871,-0.555703413721375,
3.78712754492824));
#40441=CARTESIAN_POINT('Ctrl Pts',(19.2054070165995,-0.626173010563829,
3.97108838428485));
#40442=CARTESIAN_POINT('Ctrl Pts',(19.1895017379119,-0.59622098845213,4.19351757937831));
#40443=CARTESIAN_POINT('Ctrl Pts',(19.1735964592243,-0.479600048885993,
4.35228505390253));
#40444=CARTESIAN_POINT('Ctrl Pts',(19.1586794432354,-0.370225264934164,
4.50118762911129));
#40445=CARTESIAN_POINT('Ctrl Pts',(19.1437624272465,-0.184617181632464,
4.59409385471947));
#40446=CARTESIAN_POINT('Ctrl Pts',(19.1288454112575,0.000222628893785728,
4.59497983522242));
#40447=CARTESIAN_POINT('Ctrl Pts',(19.0211545887425,-0.000526118841417405,
4.59432346427954));
#40448=CARTESIAN_POINT('Ctrl Pts',(19.0242658457596,-0.0391895592568775,
4.59468017342281));
#40449=CARTESIAN_POINT('Ctrl Pts',(19.0273771027768,-0.0777896429211806,
4.59123148246997));
#40450=CARTESIAN_POINT('Ctrl Pts',(19.030488359794,-0.115590453236054,4.58374636034569));
#40451=CARTESIAN_POINT('Ctrl Pts',(19.0463936384816,-0.308834669113126,
4.5454811341878));
#40452=CARTESIAN_POINT('Ctrl Pts',(19.0622989171692,-0.481190439544719,
4.40172662532195));
#40453=CARTESIAN_POINT('Ctrl Pts',(19.0782041958568,-0.553519286527586,
4.21848882245705));
#40454=CARTESIAN_POINT('Ctrl Pts',(19.0941094745444,-0.625848133510457,
4.03525101959215));
#40455=CARTESIAN_POINT('Ctrl Pts',(19.1100147532321,-0.598150057044591,
3.81252992272818));
#40456=CARTESIAN_POINT('Ctrl Pts',(19.1259200319197,-0.483142842019737,
3.65258963701249));
#40457=CARTESIAN_POINT('Ctrl Pts',(19.1418253106073,-0.36813562699489,3.49264935129682));
#40458=CARTESIAN_POINT('Ctrl Pts',(19.1577305892949,-0.165819273411065,
3.39548987672941));
#40459=CARTESIAN_POINT('Ctrl Pts',(19.1736358679825,0.0309111084379188,
3.40572273351557));
#40460=CARTESIAN_POINT('Ctrl Pts',(19.1895411466701,0.227641490286902,3.41595559030173));
#40461=CARTESIAN_POINT('Ctrl Pts',(19.2054464253577,0.418785900401045,3.53358077844144));
#40462=CARTESIAN_POINT('Ctrl Pts',(19.2213517040453,0.516578912360374,3.70458978792342));
#40463=CARTESIAN_POINT('Ctrl Pts',(19.237256982733,0.614371924319703,3.87559879740541));
#40464=CARTESIAN_POINT('Ctrl Pts',(19.2531622614206,0.618813538124218,4.09999162822965));
#40465=CARTESIAN_POINT('Ctrl Pts',(19.2690675401082,0.527864352527146,4.27473658562515));
#40466=CARTESIAN_POINT('Ctrl Pts',(19.2849728187958,0.436915166930073,4.44948154302064));
#40467=CARTESIAN_POINT('Ctrl Pts',(19.3008780974834,0.250575181931413,4.5745786269874));
#40468=CARTESIAN_POINT('Ctrl Pts',(19.316783376171,0.0544038354309166,4.59258854924263));
#40469=CARTESIAN_POINT('Ctrl Pts',(19.3182404470282,0.0364327229714708,
4.59423842494573));
#40470=CARTESIAN_POINT('Ctrl Pts',(19.3196975178853,0.0183791031991185,
4.59498959766064));
#40471=CARTESIAN_POINT('Ctrl Pts',(19.3211545887425,0.000315695961457875,
4.59487351203822));
#40472=CARTESIAN_POINT('Origin',(4.,0.,4.));
#40473=CARTESIAN_POINT('',(19.7288454112575,-0.000401422265437046,4.59340756962635));
#40474=CARTESIAN_POINT('',(19.6211545887425,0.000364945106097663,4.59334757974602));
#40475=CARTESIAN_POINT('',(4.,-7.27562663373442E-17,4.5941));
#40476=CARTESIAN_POINT('Ctrl Pts',(19.7288454112575,-0.000401422265437046,
4.59340756962635));
#40477=CARTESIAN_POINT('Ctrl Pts',(19.7187204928102,0.125914276337785,4.59262579220321));
#40478=CARTESIAN_POINT('Ctrl Pts',(19.7085955743629,0.252675872983383,4.55317429478549));
#40479=CARTESIAN_POINT('Ctrl Pts',(19.6984706559155,0.353547469597214,4.47867015725961));
#40480=CARTESIAN_POINT('Ctrl Pts',(19.6825653772279,0.512007102052776,4.36163128164859));
#40481=CARTESIAN_POINT('Ctrl Pts',(19.6666600985403,0.606576931433326,4.15809158444534));
#40482=CARTESIAN_POINT('Ctrl Pts',(19.6507548198527,0.593834428727047,3.9615078130365));
#40483=CARTESIAN_POINT('Ctrl Pts',(19.6348495411651,0.581091926020768,3.76492404162769));
#40484=CARTESIAN_POINT('Ctrl Pts',(19.6189442624775,0.46103709122769,3.57529619601327));
#40485=CARTESIAN_POINT('Ctrl Pts',(19.6030389837899,0.288794059426421,3.47969339775167));
#40486=CARTESIAN_POINT('Ctrl Pts',(19.5871337051022,0.116551027625133,3.38409059949006));
#40487=CARTESIAN_POINT('Ctrl Pts',(19.5712284264146,-0.107880201184358,
3.38251284858128));
#40488=CARTESIAN_POINT('Ctrl Pts',(19.555323147727,-0.281450319664219,3.47568456171554));
#40489=CARTESIAN_POINT('Ctrl Pts',(19.5394178690394,-0.45502043814407,3.5688562748498));
#40490=CARTESIAN_POINT('Ctrl Pts',(19.5235125903518,-0.577729446294298,
3.75677745202708));
#40491=CARTESIAN_POINT('Ctrl Pts',(19.5076073116642,-0.593234549413986,
3.95316264945144));
#40492=CARTESIAN_POINT('Ctrl Pts',(19.4917020329766,-0.608739652533674,
4.1495478468758));
#40493=CARTESIAN_POINT('Ctrl Pts',(19.475796754289,-0.517040850622822,4.35439706454724));
#40494=CARTESIAN_POINT('Ctrl Pts',(19.4598914756013,-0.360242359119356,
4.47365220261941));
#40495=CARTESIAN_POINT('Ctrl Pts',(19.4495427874867,-0.258222223711561,
4.55124494740629));
#40496=CARTESIAN_POINT('Ctrl Pts',(19.4391940993721,-0.128642866595325,
4.59260240088276));
#40497=CARTESIAN_POINT('Ctrl Pts',(19.4288454112575,0.000431836873498515,
4.59346738712276));
#40498=CARTESIAN_POINT('Ctrl Pts',(19.3211545887425,0.000315695961457875,
4.59487351203822));
#40499=CARTESIAN_POINT('Ctrl Pts',(19.3356027965729,-0.178799726336078,
4.59372241551416));
#40500=CARTESIAN_POINT('Ctrl Pts',(19.3500510044034,-0.35887750705714,4.50729762043595));
#40501=CARTESIAN_POINT('Ctrl Pts',(19.3644992122339,-0.469016560662847,
4.36625733020606));
#40502=CARTESIAN_POINT('Ctrl Pts',(19.3804044909215,-0.590262902253753,
4.21099342837053));
#40503=CARTESIAN_POINT('Ctrl Pts',(19.3963097696091,-0.626752877433238,
3.98954286415574));
#40504=CARTESIAN_POINT('Ctrl Pts',(19.4122150482967,-0.561731832709929,
3.80358636875254));
#40505=CARTESIAN_POINT('Ctrl Pts',(19.4281203269843,-0.49671078798662,3.61762987334934));
#40506=CARTESIAN_POINT('Ctrl Pts',(19.4440256056719,-0.330178723360516,
3.46716744675772));
#40507=CARTESIAN_POINT('Ctrl Pts',(19.4599308843595,-0.138600118749324,
3.42128506802099));
#40508=CARTESIAN_POINT('Ctrl Pts',(19.4758361630471,0.0529784858618673,
3.37540268928427));
#40509=CARTESIAN_POINT('Ctrl Pts',(19.4917414417347,0.269603630458146,3.43410035840244));
#40510=CARTESIAN_POINT('Ctrl Pts',(19.5076467204224,0.411810215621333,3.57042659223364));
#40511=CARTESIAN_POINT('Ctrl Pts',(19.52355199911,0.554016800784528,3.70675282606484));
#40512=CARTESIAN_POINT('Ctrl Pts',(19.5394572777976,0.621804826514621,3.92070762460909));
#40513=CARTESIAN_POINT('Ctrl Pts',(19.5553625564852,0.584048894878601,4.11405198996909));
#40514=CARTESIAN_POINT('Ctrl Pts',(19.5712678351728,0.546292963242583,4.30739635532907));
#40515=CARTESIAN_POINT('Ctrl Pts',(19.5871731138604,0.402993074240464,4.4801302875048));
#40516=CARTESIAN_POINT('Ctrl Pts',(19.6030783925481,0.219946482677819,4.55294168410437));
#40517=CARTESIAN_POINT('Ctrl Pts',(19.6091037912795,0.150602919307179,4.5805248346624));
#40518=CARTESIAN_POINT('Ctrl Pts',(19.615129190011,0.0755552166468998,4.59376787586841));
#40519=CARTESIAN_POINT('Ctrl Pts',(19.6211545887425,0.000364945106097663,
4.59334757974602));
#40520=CARTESIAN_POINT('Origin',(4.,0.,4.));
#40521=CARTESIAN_POINT('',(20.0288454112575,-0.000266600559035268,4.5949350414008));
#40522=CARTESIAN_POINT('',(19.9211545887425,-0.000461335262921832,4.59353843444423));
#40523=CARTESIAN_POINT('',(4.,-7.27562663373442E-17,4.5941));
#40524=CARTESIAN_POINT('Ctrl Pts',(20.0288454112575,-0.000266600559035268,
4.5949350414008));
#40525=CARTESIAN_POINT('Ctrl Pts',(20.0141521649359,0.181839152323842,4.59391190659116));
#40526=CARTESIAN_POINT('Ctrl Pts',(19.9994589186142,0.364814066967773,4.50413264800542));
#40527=CARTESIAN_POINT('Ctrl Pts',(19.9847656722925,0.474598868642052,4.35899217880197));
#40528=CARTESIAN_POINT('Ctrl Pts',(19.9688603936049,0.593439717564554,4.20187920587587));
#40529=CARTESIAN_POINT('Ctrl Pts',(19.9529551149173,0.626517665065843,3.97989492921597));
#40530=CARTESIAN_POINT('Ctrl Pts',(19.9370498362297,0.558641803885684,3.79496194153783));
#40531=CARTESIAN_POINT('Ctrl Pts',(19.9211445575421,0.490765942705524,3.61002895385969));
#40532=CARTESIAN_POINT('Ctrl Pts',(19.9052392788545,0.321936272843916,3.46214725516331));
#40533=CARTESIAN_POINT('Ctrl Pts',(19.8893340001669,0.129673778938228,3.41921955761011));
#40534=CARTESIAN_POINT('Ctrl Pts',(19.8734287214793,-0.0625887149674591,
3.37629186005692));
#40535=CARTESIAN_POINT('Ctrl Pts',(19.8575234427916,-0.278284032917226,
3.43831816364691));
#40536=CARTESIAN_POINT('Ctrl Pts',(19.841618164104,-0.418374827314372,3.57681771754473));
#40537=CARTESIAN_POINT('Ctrl Pts',(19.8257128854164,-0.558465621711518,
3.71531727144255));
#40538=CARTESIAN_POINT('Ctrl Pts',(19.8098076067288,-0.622951892556044,
3.9302900756482));
#40539=CARTESIAN_POINT('Ctrl Pts',(19.7939023280412,-0.58222383973146,4.12303018792675));
#40540=CARTESIAN_POINT('Ctrl Pts',(19.7779970493536,-0.541495786906873,
4.3157703002053));
#40541=CARTESIAN_POINT('Ctrl Pts',(19.762091770666,-0.395553410413165,4.48627772055676));
#40542=CARTESIAN_POINT('Ctrl Pts',(19.7461864919784,-0.211407504401025,
4.55626240372308));
#40543=CARTESIAN_POINT('Ctrl Pts',(19.7404061317381,-0.144484459893097,
4.58169651826758));
#40544=CARTESIAN_POINT('Ctrl Pts',(19.7346257714978,-0.0725156072563085,
4.59385388977766));
#40545=CARTESIAN_POINT('Ctrl Pts',(19.7288454112575,-0.000401422265437046,
4.59340756962635));
#40546=CARTESIAN_POINT('Ctrl Pts',(19.6211545887425,0.000364945106097663,
4.59334757974602));
#40547=CARTESIAN_POINT('Ctrl Pts',(19.6310344686986,-0.122924963130536,
4.59265841784648));
#40548=CARTESIAN_POINT('Ctrl Pts',(19.6409143486547,-0.246598186964828,
4.55523353708024));
#40549=CARTESIAN_POINT('Ctrl Pts',(19.6507942286109,-0.346136160298313,
4.48405653351353));
#40550=CARTESIAN_POINT('Ctrl Pts',(19.6666995072985,-0.506378917588675,
4.36947112529969));
#40551=CARTESIAN_POINT('Ctrl Pts',(19.6826047859861,-0.60407113804621,4.16741144784858));
#40552=CARTESIAN_POINT('Ctrl Pts',(19.6985100646737,-0.5943566574826,3.97065479758251));
#40553=CARTESIAN_POINT('Ctrl Pts',(19.7144153433613,-0.584642176918989,
3.77389814731645));
#40554=CARTESIAN_POINT('Ctrl Pts',(19.7303206220489,-0.467520995334232,
3.58244452423543));
#40555=CARTESIAN_POINT('Ctrl Pts',(19.7462259007365,-0.296770260159971,
3.48420125495101));
#40556=CARTESIAN_POINT('Ctrl Pts',(19.7621311794242,-0.12601952498572,3.38595798566659));
#40557=CARTESIAN_POINT('Ctrl Pts',(19.7780364581118,0.098360763778029,3.38092507017875));
#40558=CARTESIAN_POINT('Ctrl Pts',(19.7939417367994,0.27334477570878,3.47141355644931));
#40559=CARTESIAN_POINT('Ctrl Pts',(19.809847015487,0.448328787639532,3.56190204271987));
#40560=CARTESIAN_POINT('Ctrl Pts',(19.8257522941746,0.573916522737285,3.74791193074883));
#40561=CARTESIAN_POINT('Ctrl Pts',(19.8416575728622,0.592443207149574,3.9440350735258));
#40562=CARTESIAN_POINT('Ctrl Pts',(19.8575628515498,0.610969891561863,4.14015821630277));
#40563=CARTESIAN_POINT('Ctrl Pts',(19.8734681302375,0.522435525288687,4.34639461382776));
#40564=CARTESIAN_POINT('Ctrl Pts',(19.8893734089251,0.367491719635661,4.46804975837363));
#40565=CARTESIAN_POINT('Ctrl Pts',(19.8999671355309,0.264291244586565,4.54907828775811));
#40566=CARTESIAN_POINT('Ctrl Pts',(19.9105608621367,0.131629953687138,4.59258455010229));
#40567=CARTESIAN_POINT('Ctrl Pts',(19.9211545887425,-0.000461335262921832,
4.59353843444423));
#40568=CARTESIAN_POINT('Origin',(4.,0.,4.));
#40569=CARTESIAN_POINT('',(20.3288454112575,0.000547175593784699,4.59423670486774));
#40570=CARTESIAN_POINT('',(20.2211545887425,-0.000159442692484791,4.59503650419094));
#40571=CARTESIAN_POINT('',(4.,-7.27562663373442E-17,4.5941));
#40572=CARTESIAN_POINT('Ctrl Pts',(20.3288454112575,0.000547175593784699,
4.59423670486774));
#40573=CARTESIAN_POINT('Ctrl Pts',(20.3254891157492,0.0422991098545892,
4.59465405164581));
#40574=CARTESIAN_POINT('Ctrl Pts',(20.3221328202408,0.0839734681026259,
4.59066114403672));
#40575=CARTESIAN_POINT('Ctrl Pts',(20.3187765247324,0.124636177719752,4.58197547152207));
#40576=CARTESIAN_POINT('Ctrl Pts',(20.3028712460448,0.317334266145104,4.54081460186972));
#40577=CARTESIAN_POINT('Ctrl Pts',(20.2869659673572,0.48731321493246,4.39426577643889));
#40578=CARTESIAN_POINT('Ctrl Pts',(20.2710606886696,0.556778600406793,4.20989870881916));
#40579=CARTESIAN_POINT('Ctrl Pts',(20.255155409982,0.626243985881127,4.02553164119943));
#40580=CARTESIAN_POINT('Ctrl Pts',(20.2392501312944,0.595195808042437,3.80334633139079));
#40581=CARTESIAN_POINT('Ctrl Pts',(20.2233448526068,0.477757630702126,3.64521515909767));
#40582=CARTESIAN_POINT('Ctrl Pts',(20.2074395739191,0.360319453361808,3.48708398680455));
#40583=CARTESIAN_POINT('Ctrl Pts',(20.1915342952315,0.156491276519859,3.39300695202695));
#40584=CARTESIAN_POINT('Ctrl Pts',(20.1756290165439,-0.04006765138094,3.40625706061923));
#40585=CARTESIAN_POINT('Ctrl Pts',(20.1597237378563,-0.236626579281727,
3.4195071692115));
#40586=CARTESIAN_POINT('Ctrl Pts',(20.1438184591687,-0.425916258241364,
3.54008442117362));
#40587=CARTESIAN_POINT('Ctrl Pts',(20.1279131804811,-0.521059912873915,
3.71258420787224));
#40588=CARTESIAN_POINT('Ctrl Pts',(20.1120079017935,-0.616203567506467,
3.88508399457085));
#40589=CARTESIAN_POINT('Ctrl Pts',(20.0961026231058,-0.617201197811932,
4.10950631600596));
#40590=CARTESIAN_POINT('Ctrl Pts',(20.0801973444182,-0.523575121773085,
4.28282745216878));
#40591=CARTESIAN_POINT('Ctrl Pts',(20.0642920657306,-0.429949045734243,
4.45614858833159));
#40592=CARTESIAN_POINT('Ctrl Pts',(20.048386787043,-0.241699263351099,4.57836853922213));
#40593=CARTESIAN_POINT('Ctrl Pts',(20.0324815083554,-0.0452724969876719,
4.59335768007126));
#40594=CARTESIAN_POINT('Ctrl Pts',(20.0312694759895,-0.030304158296608,
4.59449989984645));
#40595=CARTESIAN_POINT('Ctrl Pts',(20.0300574436235,-0.0152883365109376,
4.5950194388496));
#40596=CARTESIAN_POINT('Ctrl Pts',(20.0288454112575,-0.000266600559035268,
4.5949350414008));
#40597=CARTESIAN_POINT('Ctrl Pts',(19.9211545887425,-0.000461335262921832,
4.59353843444423));
#40598=CARTESIAN_POINT('Ctrl Pts',(19.9264661408243,-0.0666901315043342,
4.5940166992278));
#40599=CARTESIAN_POINT('Ctrl Pts',(19.9317776929061,-0.132775635823809,
4.58379778651276));
#40600=CARTESIAN_POINT('Ctrl Pts',(19.9370892449879,-0.194932679790098,
4.56224768701753));
#40601=CARTESIAN_POINT('Ctrl Pts',(19.9529945236755,-0.381060028529917,
4.49771657954882));
#40602=CARTESIAN_POINT('Ctrl Pts',(19.9688998023631,-0.531961480976676,
4.33158047304464));
#40603=CARTESIAN_POINT('Ctrl Pts',(19.9848050810507,-0.578348134104426,
4.14012389605102));
#40604=CARTESIAN_POINT('Ctrl Pts',(20.0007103597384,-0.624734787232175,
3.94866731905739));
#40605=CARTESIAN_POINT('Ctrl Pts',(20.016615638426,-0.566606641040915,3.73189027157431));
#40606=CARTESIAN_POINT('Ctrl Pts',(20.0325209171136,-0.430656211588969,
3.58932409618151));
#40607=CARTESIAN_POINT('Ctrl Pts',(20.0484261958012,-0.294705782137024,
3.44675792078871));
#40608=CARTESIAN_POINT('Ctrl Pts',(20.0643314744888,-0.080933069424392,
3.37840261748619));
#40609=CARTESIAN_POINT('Ctrl Pts',(20.0802367531764,0.112511319004002,3.41565067076361));
#40610=CARTESIAN_POINT('Ctrl Pts',(20.096142031864,0.305955707432406,3.45289872404102));
#40611=CARTESIAN_POINT('Ctrl Pts',(20.1120473105516,0.479071771576571,3.59575013389837));
#40612=CARTESIAN_POINT('Ctrl Pts',(20.1279525892393,0.552362916535151,3.77860107435498));
#40613=CARTESIAN_POINT('Ctrl Pts',(20.1438578679269,0.625654061493722,3.96145201481158));
#40614=CARTESIAN_POINT('Ctrl Pts',(20.1597631466145,0.599120287266732,4.18430248586742));
#40615=CARTESIAN_POINT('Ctrl Pts',(20.1756684253021,0.484961816589866,4.3448525870839));
#40616=CARTESIAN_POINT('Ctrl Pts',(20.1908304797822,0.376137759761604,4.49790047950022));
#40617=CARTESIAN_POINT('Ctrl Pts',(20.2059925342623,0.187686755696174,4.59433432972249));
#40618=CARTESIAN_POINT('Ctrl Pts',(20.2211545887425,-0.000159442692484791,
4.59503650419094));
#40619=CARTESIAN_POINT('Origin',(4.,0.,4.));
#40620=CARTESIAN_POINT('',(20.6288454112575,1.84392275237588E-6,4.59415158619139));
#40621=CARTESIAN_POINT('',(20.5211545887425,0.00014515264107467,4.59408556636595));
#40622=CARTESIAN_POINT('',(4.,-7.27562663373442E-17,4.5941));
#40623=CARTESIAN_POINT('Ctrl Pts',(20.6288454112575,1.84392275237588E-6,
4.59415158619139));
#40624=CARTESIAN_POINT('Ctrl Pts',(20.6209207878748,0.0985777406598016,
4.59414764832452));
#40625=CARTESIAN_POINT('Ctrl Pts',(20.6129961644921,0.197149291092008,4.56908802213256));
#40626=CARTESIAN_POINT('Ctrl Pts',(20.6050715411094,0.283761277174982,4.52200793915563));
#40627=CARTESIAN_POINT('Ctrl Pts',(20.5971189017656,0.370679463050262,4.47476141372331));
#40628=CARTESIAN_POINT('Ctrl Pts',(20.5891662624218,0.445553373684486,4.40533845822152));
#40629=CARTESIAN_POINT('Ctrl Pts',(20.581213623078,0.499196468040806,4.3222224876916));
#40630=CARTESIAN_POINT('Ctrl Pts',(20.5732609837342,0.552839562397126,4.23910651716169));
#40631=CARTESIAN_POINT('Ctrl Pts',(20.5653083443904,0.585251840475543,4.14229753160364));
#40632=CARTESIAN_POINT('Ctrl Pts',(20.5573557050466,0.592531230276538,4.04364021904617));
#40633=CARTESIAN_POINT('Ctrl Pts',(20.5494030657028,0.599810620077534,3.9449829064887));
#40634=CARTESIAN_POINT('Ctrl Pts',(20.541450426359,0.581957121601108,3.84447726693182));
#40635=CARTESIAN_POINT('Ctrl Pts',(20.5334977870152,0.541038843355354,3.75439549632807));
#40636=CARTESIAN_POINT('Ctrl Pts',(20.5255451476714,0.5001205651096,3.66431372572433));
#40637=CARTESIAN_POINT('Ctrl Pts',(20.5175925083276,0.436137507094518,3.58465582407373));
#40638=CARTESIAN_POINT('Ctrl Pts',(20.5096398689838,0.357128912623608,3.5251911792601));
#40639=CARTESIAN_POINT('Ctrl Pts',(20.50168722964,0.278120318152698,3.46572653444646));
#40640=CARTESIAN_POINT('Ctrl Pts',(20.4937345902962,0.184086187225959,3.42645514646979));
#40641=CARTESIAN_POINT('Ctrl Pts',(20.4857819509524,0.0861162623359374,
3.4121221101222));
#40642=CARTESIAN_POINT('Ctrl Pts',(20.4778293116085,-0.0118536625540841,
3.39778907377461));
#40643=CARTESIAN_POINT('Ctrl Pts',(20.4698766722647,-0.113759381407388,
3.4083943890561));
#40644=CARTESIAN_POINT('Ctrl Pts',(20.4619240329209,-0.206384677702653,
3.44274365129583));
#40645=CARTESIAN_POINT('Ctrl Pts',(20.4539713935771,-0.299009973997917,
3.47709291353557));
#40646=CARTESIAN_POINT('Ctrl Pts',(20.4460187542333,-0.382354847735142,
3.53518612273354));
#40647=CARTESIAN_POINT('Ctrl Pts',(20.4380661148895,-0.447563842371028,
3.60976099223211));
#40648=CARTESIAN_POINT('Ctrl Pts',(20.4301134755457,-0.512772837006921,
3.68433586173069));
#40649=CARTESIAN_POINT('Ctrl Pts',(20.4221608362019,-0.559845952541473,
3.77539239152987));
#40650=CARTESIAN_POINT('Ctrl Pts',(20.4142081968581,-0.580888308445953,
3.87190852591559));
#40651=CARTESIAN_POINT('Ctrl Pts',(20.3983029181705,-0.622973020254908,
4.06494079468701));
#40652=CARTESIAN_POINT('Ctrl Pts',(20.3823976394829,-0.5609346935436,4.27981148180459));
#40653=CARTESIAN_POINT('Ctrl Pts',(20.3664923607953,-0.422206916156273,
4.41936036842645));
#40654=CARTESIAN_POINT('Ctrl Pts',(20.353943377616,-0.312753156865475,4.52946196836027));
#40655=CARTESIAN_POINT('Ctrl Pts',(20.3413943944368,-0.155560747392339,
4.59267627084609));
#40656=CARTESIAN_POINT('Ctrl Pts',(20.3288454112575,0.000547175593784699,
4.59423670486774));
#40657=CARTESIAN_POINT('Ctrl Pts',(20.2211545887425,-0.000159442692484791,
4.59503650419094));
#40658=CARTESIAN_POINT('Ctrl Pts',(20.22189781295,-0.00936741923094289,
4.59507092387091));
#40659=CARTESIAN_POINT('Ctrl Pts',(20.2226410371574,-0.0185739425223631,
4.59487531632137));
#40660=CARTESIAN_POINT('Ctrl Pts',(20.2233842613649,-0.0277695625699301,
4.59444507412072));
#40661=CARTESIAN_POINT('Ctrl Pts',(20.2392895400526,-0.224559303926058,
4.58523772856393));
#40662=CARTESIAN_POINT('Ctrl Pts',(20.2551948187402,-0.416355619511548,
4.46857330607325));
#40663=CARTESIAN_POINT('Ctrl Pts',(20.2711000974278,-0.51503297954037,4.29810345018796));
#40664=CARTESIAN_POINT('Ctrl Pts',(20.2870053761154,-0.613710339569191,
4.12763359430267));
#40665=CARTESIAN_POINT('Ctrl Pts',(20.302910654803,-0.619268744041345,3.90335830502277));
#40666=CARTESIAN_POINT('Ctrl Pts',(20.3188159334906,-0.529271009537506,
3.72809546473432));
#40667=CARTESIAN_POINT('Ctrl Pts',(20.3347212121782,-0.439273275033663,
3.55283262444587));
#40668=CARTESIAN_POINT('Ctrl Pts',(20.3506264908658,-0.253719401553817,
3.42658223314887));
#40669=CARTESIAN_POINT('Ctrl Pts',(20.3665317695535,-0.0575887485100287,
3.40762076142476));
#40670=CARTESIAN_POINT('Ctrl Pts',(20.3824370482411,0.138541904533748,3.38865928970065));
#40671=CARTESIAN_POINT('Ctrl Pts',(20.3983423269287,0.345249337141466,3.47698673754941));
#40672=CARTESIAN_POINT('Ctrl Pts',(20.4142476056163,0.467192899405167,3.63141813202173));
#40673=CARTESIAN_POINT('Ctrl Pts',(20.4301528843039,0.589136461668875,3.78584952649406));
#40674=CARTESIAN_POINT('Ctrl Pts',(20.4460581629915,0.626316153588557,4.00638486758996));
#40675=CARTESIAN_POINT('Ctrl Pts',(20.4619634416791,0.562534942182983,4.19337293359078));
#40676=CARTESIAN_POINT('Ctrl Pts',(20.4699160810229,0.530644336480201,4.28686696659118));
#40677=CARTESIAN_POINT('Ctrl Pts',(20.4778687203667,0.473513504946115,4.3719741808178));
#40678=CARTESIAN_POINT('Ctrl Pts',(20.4858213597105,0.400240502138227,4.43864269813793));
#40679=CARTESIAN_POINT('Ctrl Pts',(20.4937739990544,0.326967499330329,4.50531121545807));
#40680=CARTESIAN_POINT('Ctrl Pts',(20.5017266383982,0.237552325248626,4.55354103587171));
#40681=CARTESIAN_POINT('Ctrl Pts',(20.509679277742,0.141619450488441,4.57712494713439));
#40682=CARTESIAN_POINT('Ctrl Pts',(20.5135043814088,0.0954771353210092,
4.58846846487098));
#40683=CARTESIAN_POINT('Ctrl Pts',(20.5173294850756,0.0478269697500401,
4.59411022582368));
#40684=CARTESIAN_POINT('Ctrl Pts',(20.5211545887425,0.00014515264107467,
4.59408556636595));
#40685=CARTESIAN_POINT('Origin',(4.,0.,4.));
#40686=CARTESIAN_POINT('',(20.9288454112575,-6.4040329070536E-6,4.59405282094147));
#40687=CARTESIAN_POINT('',(20.8211545887425,5.65245430726296E-6,4.59414685459231));
#40688=CARTESIAN_POINT('',(4.,-7.27562663373442E-17,4.5941));
#40689=CARTESIAN_POINT('Ctrl Pts',(20.9288454112575,-6.4040329070536E-6,
4.59405282094147));
#40690=CARTESIAN_POINT('Ctrl Pts',(20.9243050993443,0.0564994875152707,
4.59403151438501));
#40691=CARTESIAN_POINT('Ctrl Pts',(20.9197647874311,0.113011285737041,4.58603249222448));
#40692=CARTESIAN_POINT('Ctrl Pts',(20.9152244755179,0.167207550221224,4.57013805289591));
#40693=CARTESIAN_POINT('Ctrl Pts',(20.9072718361741,0.262135685878584,4.5422979516059));
#40694=CARTESIAN_POINT('Ctrl Pts',(20.8993191968303,0.349959832061366,4.49023494241839));
#40695=CARTESIAN_POINT('Ctrl Pts',(20.8913665574865,0.419942299057043,4.42031443844746));
#40696=CARTESIAN_POINT('Ctrl Pts',(20.8834139181427,0.489924766052721,4.35039393447653));
#40697=CARTESIAN_POINT('Ctrl Pts',(20.8754612787989,0.542065553861293,4.26261593572219));
#40698=CARTESIAN_POINT('Ctrl Pts',(20.8675086394551,0.569989725359365,4.16771249585991));
#40699=CARTESIAN_POINT('Ctrl Pts',(20.8595560001113,0.597913896857441,4.07280905599763));
#40700=CARTESIAN_POINT('Ctrl Pts',(20.8516033607674,0.601621452045013,3.97078017502742));
#40701=CARTESIAN_POINT('Ctrl Pts',(20.8436507214236,0.580659121393648,3.87410027737825));
#40702=CARTESIAN_POINT('Ctrl Pts',(20.8356980820798,0.559696790742287,3.77742037972911));
#40703=CARTESIAN_POINT('Ctrl Pts',(20.827745442736,0.514064574252002,3.686089465401));
#40704=CARTESIAN_POINT('Ctrl Pts',(20.8197928033922,0.44934157601673,3.61127397478397));
#40705=CARTESIAN_POINT('Ctrl Pts',(20.8118401640484,0.384618577781443,3.53645848416692));
#40706=CARTESIAN_POINT('Ctrl Pts',(20.8038875247046,0.300804797801161,3.47815841726095));
#40707=CARTESIAN_POINT('Ctrl Pts',(20.7959348853608,0.208147717693743,3.44350176598286));
#40708=CARTESIAN_POINT('Ctrl Pts',(20.787982246017,0.115490637586335,3.40884511470477));
#40709=CARTESIAN_POINT('Ctrl Pts',(20.7800296066732,0.0139902573517945,
3.39783187905454));
#40710=CARTESIAN_POINT('Ctrl Pts',(20.7720769673294,-0.0839438183138644,
3.41180854931868));
#40711=CARTESIAN_POINT('Ctrl Pts',(20.7641243279856,-0.181877893979523,
3.42578521958283));
#40712=CARTESIAN_POINT('Ctrl Pts',(20.7561716886418,-0.2762456650763,3.46475179576135));
#40713=CARTESIAN_POINT('Ctrl Pts',(20.748219049298,-0.355509010203556,3.52394413563581));
#40714=CARTESIAN_POINT('Ctrl Pts',(20.7402664099542,-0.434772355330821,
3.58313647551028));
#40715=CARTESIAN_POINT('Ctrl Pts',(20.7323137706103,-0.498931274488562,
3.66255457908069));
#40716=CARTESIAN_POINT('Ctrl Pts',(20.7243611312665,-0.54014217617541,3.75248840252759));
#40717=CARTESIAN_POINT('Ctrl Pts',(20.7164084919227,-0.581353077862249,
3.84242222597448));
#40718=CARTESIAN_POINT('Ctrl Pts',(20.7084558525789,-0.599615962078206,
3.94287176929784));
#40719=CARTESIAN_POINT('Ctrl Pts',(20.7005032132351,-0.592696601504336,
4.0415558946729));
#40720=CARTESIAN_POINT('Ctrl Pts',(20.6925505738913,-0.585777240930466,
4.14024002004797));
#40721=CARTESIAN_POINT('Ctrl Pts',(20.6845979345475,-0.553675635566762,
4.23715872747472));
#40722=CARTESIAN_POINT('Ctrl Pts',(20.6766452952037,-0.50031917594212,4.32046203197985));
#40723=CARTESIAN_POINT('Ctrl Pts',(20.6686926558599,-0.446962716317479,
4.40376533648498));
#40724=CARTESIAN_POINT('Ctrl Pts',(20.6607400165161,-0.3723514024319,4.47345323806848));
#40725=CARTESIAN_POINT('Ctrl Pts',(20.6527873771723,-0.285602702553558,
4.52100610813718));
#40726=CARTESIAN_POINT('Ctrl Pts',(20.6448347378285,-0.198854002675205,
4.56855897820588));
#40727=CARTESIAN_POINT('Ctrl Pts',(20.6368820984847,-0.099967916804087,
4.59397681675976));
#40728=CARTESIAN_POINT('Ctrl Pts',(20.6289294591409,-0.00104364331035449,
4.59415068835528));
#40729=CARTESIAN_POINT('Ctrl Pts',(20.6289014431798,-0.000695147863829354,
4.59415130087895));
#40730=CARTESIAN_POINT('Ctrl Pts',(20.6288734272186,-0.000346651943377611,
4.59415160011295));
#40731=CARTESIAN_POINT('Ctrl Pts',(20.6288454112575,1.84392275237588E-6,
4.59415158619139));
#40732=CARTESIAN_POINT('Ctrl Pts',(20.5211545887425,0.00014515264107467,
4.59408556636595));
#40733=CARTESIAN_POINT('Ctrl Pts',(20.5252821244194,-0.0513066296901884,
4.59405895720698));
#40734=CARTESIAN_POINT('Ctrl Pts',(20.5294096600964,-0.102795266482965,
4.58743447362686));
#40735=CARTESIAN_POINT('Ctrl Pts',(20.5335371957734,-0.152465997634008,
4.57425651377355));
#40736=CARTESIAN_POINT('Ctrl Pts',(20.5414898351172,-0.248167995557571,
4.5488661670383));
#40737=CARTESIAN_POINT('Ctrl Pts',(20.549442474461,-0.33712141596603,4.49914747145609));
#40738=CARTESIAN_POINT('Ctrl Pts',(20.5573951138048,-0.408848640915227,
4.43107686705031));
#40739=CARTESIAN_POINT('Ctrl Pts',(20.5653477531486,-0.480575865864423,
4.36300626264453));
#40740=CARTESIAN_POINT('Ctrl Pts',(20.5733003924924,-0.535076895354358,
4.27658374941519));
#40741=CARTESIAN_POINT('Ctrl Pts',(20.5812530318362,-0.565476628275392,
4.18243021985824));
#40742=CARTESIAN_POINT('Ctrl Pts',(20.58920567118,-0.595876361196427,4.08827669030129));
#40743=CARTESIAN_POINT('Ctrl Pts',(20.5971583105238,-0.602174797548561,
3.98639214441672));
#40744=CARTESIAN_POINT('Ctrl Pts',(20.6051109498677,-0.58371402745925,3.88920441471463));
#40745=CARTESIAN_POINT('Ctrl Pts',(20.6130635892115,-0.565253257369939,
3.79201668501254));
#40746=CARTESIAN_POINT('Ctrl Pts',(20.6210162285553,-0.522033280839182,
3.69952577149293));
#40747=CARTESIAN_POINT('Ctrl Pts',(20.6289688678991,-0.459278917219465,
3.62305528060961));
#40748=CARTESIAN_POINT('Ctrl Pts',(20.6369215072429,-0.396524553599749,
3.54658478972629));
#40749=CARTESIAN_POINT('Ctrl Pts',(20.6448741465867,-0.314235802891072,
3.48613472147926));
#40750=CARTESIAN_POINT('Ctrl Pts',(20.6528267859305,-0.222505051509483,
3.44908779917463));
#40751=CARTESIAN_POINT('Ctrl Pts',(20.6607794252743,-0.130774300127894,
3.41204087687));
#40752=CARTESIAN_POINT('Ctrl Pts',(20.6687320646181,-0.029601548073392,
3.39839710050778));
#40753=CARTESIAN_POINT('Ctrl Pts',(20.6766847039619,0.0686601223983595,
3.40982890848785));
#40754=CARTESIAN_POINT('Ctrl Pts',(20.6846373433057,0.1669217928701,3.42126071646792));
#40755=CARTESIAN_POINT('Ctrl Pts',(20.6925899826495,0.262272381759091,3.45776810879028));
#40756=CARTESIAN_POINT('Ctrl Pts',(20.7005426219933,0.343045155251024,3.51488528173127));
#40757=CARTESIAN_POINT('Ctrl Pts',(20.7084952613371,0.423817928742975,3.57200245467228));
#40758=CARTESIAN_POINT('Ctrl Pts',(20.7164479006809,0.490012886837861,3.64972940823193));
#40759=CARTESIAN_POINT('Ctrl Pts',(20.7244005400247,0.533541468465666,3.73856417004634));
#40760=CARTESIAN_POINT('Ctrl Pts',(20.7323531793686,0.577070050093471,3.82739893186076));
#40761=CARTESIAN_POINT('Ctrl Pts',(20.7403058187123,0.597932255254196,3.92734150192994));
#40762=CARTESIAN_POINT('Ctrl Pts',(20.7482584580562,0.593574919799613,4.02617190099588));
#40763=CARTESIAN_POINT('Ctrl Pts',(20.7562110974,0.589217584345031,4.1250023000618));
#40764=CARTESIAN_POINT('Ctrl Pts',(20.7641637367438,0.559640708275147,4.22272052812447));
#40765=CARTESIAN_POINT('Ctrl Pts',(20.7721163760876,0.508461778515953,4.30737953925928));
#40766=CARTESIAN_POINT('Ctrl Pts',(20.7800690154314,0.457282848756759,4.39203855039408));
#40767=CARTESIAN_POINT('Ctrl Pts',(20.7880216547752,0.384501865308254,4.46363834460102));
#40768=CARTESIAN_POINT('Ctrl Pts',(20.795974294119,0.299016600344635,4.51342469267633));
#40769=CARTESIAN_POINT('Ctrl Pts',(20.8039269334628,0.213531335381016,4.56321104075164));
#40770=CARTESIAN_POINT('Ctrl Pts',(20.8118795728066,0.115341788902283,4.59118394269532));
#40771=CARTESIAN_POINT('Ctrl Pts',(20.8198322121504,0.0164533379892873,
4.59392342516246));
#40772=CARTESIAN_POINT('Ctrl Pts',(20.8202730043478,0.0109722321971217,
4.59407526688998));
#40773=CARTESIAN_POINT('Ctrl Pts',(20.8207137965451,0.00548897925183007,
4.59414958726715));
#40774=CARTESIAN_POINT('Ctrl Pts',(20.8211545887425,5.65245430726296E-6,
4.59414685459231));
#40775=CARTESIAN_POINT('Origin',(4.,0.,4.));
#40776=CARTESIAN_POINT('',(21.2288454112575,1.28243205298473E-5,4.59412621697841));
#40777=CARTESIAN_POINT('',(21.1211545887425,-1.09306879613159E-5,4.5940621922514));
#40778=CARTESIAN_POINT('',(4.,-7.27562663373442E-17,4.5941));
#40779=CARTESIAN_POINT('Ctrl Pts',(21.2288454112575,1.28243205298473E-5,
4.59412621697841));
#40780=CARTESIAN_POINT('Ctrl Pts',(21.2276894108138,0.0143945780386088,
4.59413985249388));
#40781=CARTESIAN_POINT('Ctrl Pts',(21.2265334103701,0.028775363636007,4.59362827285675));
#40782=CARTESIAN_POINT('Ctrl Pts',(21.2253774099263,0.043117441953227,4.59258471957415));
#40783=CARTESIAN_POINT('Ctrl Pts',(21.2174247705826,0.141782954511012,4.58540565408365));
#40784=CARTESIAN_POINT('Ctrl Pts',(21.2094721312387,0.238616577754522,4.55305001116024));
#40785=CARTESIAN_POINT('Ctrl Pts',(21.2015194918949,0.321779082392626,4.49947370882601));
#40786=CARTESIAN_POINT('Ctrl Pts',(21.1935668525511,0.404941587030731,4.44589740649178));
#40787=CARTESIAN_POINT('Ctrl Pts',(21.1856142132073,0.474432973063433,4.37110044474674));
#40788=CARTESIAN_POINT('Ctrl Pts',(21.1776615738635,0.521756972098598,4.28422777087894));
#40789=CARTESIAN_POINT('Ctrl Pts',(21.1697089345197,0.569080971133768,4.19735509701114));
#40790=CARTESIAN_POINT('Ctrl Pts',(21.1617562951759,0.594237583171398,4.09840671102057));
#40791=CARTESIAN_POINT('Ctrl Pts',(21.1538036558321,0.594151069756079,3.9994804007435));
#40792=CARTESIAN_POINT('Ctrl Pts',(21.1458510164883,0.59406455634076,3.90055409046644));
#40793=CARTESIAN_POINT('Ctrl Pts',(21.1378983771445,0.568734917472505,3.80164985590287));
#40794=CARTESIAN_POINT('Ctrl Pts',(21.1299457378007,0.521259046500119,3.71486008677882));
#40795=CARTESIAN_POINT('Ctrl Pts',(21.1219930984569,0.473783175527722,3.62807031765475));
#40796=CARTESIAN_POINT('Ctrl Pts',(21.114040459113,0.40416107245118,3.5533950139702));
#40797=CARTESIAN_POINT('Ctrl Pts',(21.1060878197692,0.320904987578411,3.49996424865404));
#40798=CARTESIAN_POINT('Ctrl Pts',(21.0981351804254,0.237648902705652,3.44653348333788));
#40799=CARTESIAN_POINT('Ctrl Pts',(21.0901825410817,0.140758836036697,3.41434725639011));
#40800=CARTESIAN_POINT('Ctrl Pts',(21.0822299017378,0.042080917889342,3.40734077242984));
#40801=CARTESIAN_POINT('Ctrl Pts',(21.074277262394,-0.056597000258024,3.40033428846957));
#40802=CARTESIAN_POINT('Ctrl Pts',(21.0663246230502,-0.157062769883762,
3.41850754749682));
#40803=CARTESIAN_POINT('Ctrl Pts',(21.0583719837064,-0.247033082431791,
3.45963862106718));
#40804=CARTESIAN_POINT('Ctrl Pts',(21.0504193443626,-0.337003394979799,
3.50076969463752));
#40805=CARTESIAN_POINT('Ctrl Pts',(21.0424667050188,-0.416478250450111,
3.56485858275095));
#40806=CARTESIAN_POINT('Ctrl Pts',(21.034514065675,-0.475740765152555,3.644069545988));
#40807=CARTESIAN_POINT('Ctrl Pts',(21.0265614263312,-0.535003279855012,
3.72328050922507));
#40808=CARTESIAN_POINT('Ctrl Pts',(21.0186087869874,-0.574053453789596,
3.81761354758578));
#40809=CARTESIAN_POINT('Ctrl Pts',(21.0106561476436,-0.588116871685884,
3.91553516229212));
#40810=CARTESIAN_POINT('Ctrl Pts',(21.0027035082998,-0.60218028958217,4.01345677699845));
#40811=CARTESIAN_POINT('Ctrl Pts',(20.994750868956,-0.591256951440166,4.11496696805043));
#40812=CARTESIAN_POINT('Ctrl Pts',(20.9867982296121,-0.556682383467722,
4.20765473214191));
#40813=CARTESIAN_POINT('Ctrl Pts',(20.9788455902683,-0.522107815495282,
4.30034249623339));
#40814=CARTESIAN_POINT('Ctrl Pts',(20.9708929509246,-0.463882017692404,
4.38420783336438));
#40815=CARTESIAN_POINT('Ctrl Pts',(20.9629403115808,-0.389123888092725,
4.4489970636758));
#40816=CARTESIAN_POINT('Ctrl Pts',(20.9549876722369,-0.314365758493028,
4.51378629398723));
#40817=CARTESIAN_POINT('Ctrl Pts',(20.9470350328931,-0.223075297096518,
4.5594994174791));
#40818=CARTESIAN_POINT('Ctrl Pts',(20.9390823935493,-0.12641400383229,4.58054738252877));
#40819=CARTESIAN_POINT('Ctrl Pts',(20.9356700661187,-0.0849384674446181,
4.58957866703598));
#40820=CARTESIAN_POINT('Ctrl Pts',(20.9322577386881,-0.0424741039190781,
4.59406883414683));
#40821=CARTESIAN_POINT('Ctrl Pts',(20.9288454112575,-6.4040329070536E-6,
4.59405282094147));
#40822=CARTESIAN_POINT('Ctrl Pts',(20.8211545887425,5.65245430726296E-6,
4.59414685459231));
#40823=CARTESIAN_POINT('Ctrl Pts',(20.8286664358889,-0.0934395423672534,
4.59410028517524));
#40824=CARTESIAN_POINT('Ctrl Pts',(20.8361782830354,-0.18690618531264,4.57167601133058));
#40825=CARTESIAN_POINT('Ctrl Pts',(20.8436901301818,-0.270133012248912,
4.529191754035));
#40826=CARTESIAN_POINT('Ctrl Pts',(20.8516427695256,-0.358243556226857,
4.4842145374498));
#40827=CARTESIAN_POINT('Ctrl Pts',(20.8595954088694,-0.434877288835492,
4.41675404128879));
#40828=CARTESIAN_POINT('Ctrl Pts',(20.8675480482133,-0.490664589397756,
4.33505825661903));
#40829=CARTESIAN_POINT('Ctrl Pts',(20.8755006875571,-0.546451889960021,
4.25336247194927));
#40830=CARTESIAN_POINT('Ctrl Pts',(20.8834533269009,-0.581392758475918,
4.15743139877076));
#40831=CARTESIAN_POINT('Ctrl Pts',(20.8914059662447,-0.591215252505097,
4.05899390323763));
#40832=CARTESIAN_POINT('Ctrl Pts',(20.8993586055885,-0.601037746534278,
3.96055640770449));
#40833=CARTESIAN_POINT('Ctrl Pts',(20.9073112449323,-0.585741866076735,
3.85961248981672));
#40834=CARTESIAN_POINT('Ctrl Pts',(20.9152638842761,-0.547197711916726,
3.76850392583047));
#40835=CARTESIAN_POINT('Ctrl Pts',(20.9232165236199,-0.508653557756717,
3.67739536184422));
#40836=CARTESIAN_POINT('Ctrl Pts',(20.9311691629637,-0.446861129894262,
3.59612215175949));
#40837=CARTESIAN_POINT('Ctrl Pts',(20.9391218023075,-0.369375409551539,
3.53462104847409));
#40838=CARTESIAN_POINT('Ctrl Pts',(20.9470744416513,-0.291889689208826,
3.4731199451887));
#40839=CARTESIAN_POINT('Ctrl Pts',(20.9550270809951,-0.198710676385865,
3.43139094870266));
#40840=CARTESIAN_POINT('Ctrl Pts',(20.9629797203389,-0.101230766359376,
3.41453599926792));
#40841=CARTESIAN_POINT('Ctrl Pts',(20.9709323596827,-0.00375085633288601,
3.39768104983318));
#40842=CARTESIAN_POINT('Ctrl Pts',(20.9788849990265,0.0980299508971346,
3.40570014744973));
#40843=CARTESIAN_POINT('Ctrl Pts',(20.9868376383704,0.191667561123074,3.43761284710704));
#40844=CARTESIAN_POINT('Ctrl Pts',(20.9947902777142,0.285305171349014,3.46952554676435));
#40845=CARTESIAN_POINT('Ctrl Pts',(21.002742917058,0.37079958457088,3.52533184846243));
#40846=CARTESIAN_POINT('Ctrl Pts',(21.0106955564018,0.437697946637459,3.59820867233944));
#40847=CARTESIAN_POINT('Ctrl Pts',(21.0186481957456,0.504596308704037,3.67108549621644));
#40848=CARTESIAN_POINT('Ctrl Pts',(21.0266008350894,0.552898619615334,3.76103284227238));
#40849=CARTESIAN_POINT('Ctrl Pts',(21.0345534744332,0.576699262792956,3.8570534220826));
#40850=CARTESIAN_POINT('Ctrl Pts',(21.042506113777,0.600499905970578,3.95307400189282));
#40851=CARTESIAN_POINT('Ctrl Pts',(21.0504587531208,0.599798881414527,4.05516781545734));
#40852=CARTESIAN_POINT('Ctrl Pts',(21.0584113924646,0.574681899562831,4.15085250374278));
#40853=CARTESIAN_POINT('Ctrl Pts',(21.0663640318084,0.549564917711138,4.24653719202821));
#40854=CARTESIAN_POINT('Ctrl Pts',(21.0743166711522,0.500031978563804,4.33581275503458));
#40855=CARTESIAN_POINT('Ctrl Pts',(21.082269310496,0.432139158218639,4.40776403918836));
#40856=CARTESIAN_POINT('Ctrl Pts',(21.0902219498398,0.364246337873458,4.47971532334216));
#40857=CARTESIAN_POINT('Ctrl Pts',(21.0981745891836,0.277993636330433,4.53434232864337));
#40858=CARTESIAN_POINT('Ctrl Pts',(21.1061272285274,0.183926621270441,4.56496615973523));
#40859=CARTESIAN_POINT('Ctrl Pts',(21.1111363485991,0.124676735433976,4.5842551580617));
#40860=CARTESIAN_POINT('Ctrl Pts',(21.1161454686708,0.0623266393968894,
4.59402126159141));
#40861=CARTESIAN_POINT('Ctrl Pts',(21.1211545887425,-1.09306879613159E-5,
4.5940621922514));
#40862=CARTESIAN_POINT('Origin',(4.,0.,4.));
#40863=CARTESIAN_POINT('',(21.5288454112575,-1.51073027558624E-5,4.59408477831653));
#40864=CARTESIAN_POINT('',(21.4211545887425,1.51733402061755E-5,4.59410821609125));
#40865=CARTESIAN_POINT('',(4.,-7.27562663373442E-17,4.5941));
#40866=CARTESIAN_POINT('Ctrl Pts',(21.5288454112575,-1.51073027558624E-5,
4.59408477831653));
#40867=CARTESIAN_POINT('Ctrl Pts',(21.5231210829395,0.0712153309254728,
4.59401644885886));
#40868=CARTESIAN_POINT('Ctrl Pts',(21.5173967546214,0.142469702059594,4.58119587380047));
#40869=CARTESIAN_POINT('Ctrl Pts',(21.5116724263034,0.209120766622247,4.55613331912479));
#40870=CARTESIAN_POINT('Ctrl Pts',(21.5037197869596,0.301717111362981,4.52131465616629));
#40871=CARTESIAN_POINT('Ctrl Pts',(21.4957671476158,0.385428743083265,4.46286809139133));
#40872=CARTESIAN_POINT('Ctrl Pts',(21.4878145082719,0.450020774675764,4.38793951336988));
#40873=CARTESIAN_POINT('Ctrl Pts',(21.4798618689281,0.514612806268249,4.31301093534845));
#40874=CARTESIAN_POINT('Ctrl Pts',(21.4719092295843,0.560085237732952,4.22160034408054));
#40875=CARTESIAN_POINT('Ctrl Pts',(21.4639565902405,0.58087844500124,4.1248839293359));
#40876=CARTESIAN_POINT('Ctrl Pts',(21.4560039508967,0.601671652269532,4.02816751459124));
#40877=CARTESIAN_POINT('Ctrl Pts',(21.4480513115529,0.597785635341394,3.92614527636987));
#40878=CARTESIAN_POINT('Ctrl Pts',(21.4400986722091,0.569695512712777,3.83129082280931));
#40879=CARTESIAN_POINT('Ctrl Pts',(21.4321460328653,0.541605390084162,3.73643636924876));
#40880=CARTESIAN_POINT('Ctrl Pts',(21.4241933935215,0.489311161755075,3.64874970034904));
#40881=CARTESIAN_POINT('Ctrl Pts',(21.4162407541777,0.419206509371839,3.57895170565158));
#40882=CARTESIAN_POINT('Ctrl Pts',(21.4082881148339,0.349101856988603,3.50915371095413));
#40883=CARTESIAN_POINT('Ctrl Pts',(21.4003354754901,0.261186780551223,3.45724439045894));
#40884=CARTESIAN_POINT('Ctrl Pts',(21.3923828361463,0.16621009553345,3.42957036558731));
#40885=CARTESIAN_POINT('Ctrl Pts',(21.3844301968025,0.0712334105156764,
3.40189634071567));
#40886=CARTESIAN_POINT('Ctrl Pts',(21.3764775574587,-0.0308048830825163,
3.3984576114676));
#40887=CARTESIAN_POINT('Ctrl Pts',(21.3685249181149,-0.127429214135013,
3.41967460932821));
#40888=CARTESIAN_POINT('Ctrl Pts',(21.360572278771,-0.22405354518751,3.44089160718882));
#40889=CARTESIAN_POINT('Ctrl Pts',(21.3526196394272,-0.315263913694308,
3.4867643321581));
#40890=CARTESIAN_POINT('Ctrl Pts',(21.3446670000834,-0.389908609845283,
3.5516842188346));
#40891=CARTESIAN_POINT('Ctrl Pts',(21.3367143607396,-0.464553305996249,
3.6166041055111));
#40892=CARTESIAN_POINT('Ctrl Pts',(21.3287617213958,-0.522632329791381,
3.70057115389483));
#40893=CARTESIAN_POINT('Ctrl Pts',(21.320809082052,-0.557044729551177,3.79331924871262));
#40894=CARTESIAN_POINT('Ctrl Pts',(21.3128564427082,-0.591457129310977,
3.88606734353042));
#40895=CARTESIAN_POINT('Ctrl Pts',(21.3049038033644,-0.602202905035458,
3.9875964847823));
#40896=CARTESIAN_POINT('Ctrl Pts',(21.2969511640206,-0.587968239287942,
4.08549335215105));
#40897=CARTESIAN_POINT('Ctrl Pts',(21.2889985246768,-0.573733573540424,
4.18339021951981));
#40898=CARTESIAN_POINT('Ctrl Pts',(21.281045885333,-0.534518466320906,4.27765481300544));
#40899=CARTESIAN_POINT('Ctrl Pts',(21.2730932459892,-0.47511749858569,4.35676200219639));
#40900=CARTESIAN_POINT('Ctrl Pts',(21.2651406066454,-0.415716530850488,
4.43586919138732));
#40901=CARTESIAN_POINT('Ctrl Pts',(21.2571879673016,-0.336129702599601,
4.49981897628356));
#40902=CARTESIAN_POINT('Ctrl Pts',(21.2492353279577,-0.246087587538132,
4.54079262470289));
#40903=CARTESIAN_POINT('Ctrl Pts',(21.2424386890577,-0.169134048541188,
4.57581031891556));
#40904=CARTESIAN_POINT('Ctrl Pts',(21.2356420501576,-0.0845438791841879,
4.59404604774026));
#40905=CARTESIAN_POINT('Ctrl Pts',(21.2288454112575,1.28243205298473E-5,
4.59412621697841));
#40906=CARTESIAN_POINT('Ctrl Pts',(21.1211545887425,-1.09306879613159E-5,
4.5940621922514));
#40907=CARTESIAN_POINT('Ctrl Pts',(21.1240981080146,-0.0366424819978743,
4.5940862444172));
#40908=CARTESIAN_POINT('Ctrl Pts',(21.1270416272867,-0.0732697079540161,
4.59075208378119));
#40909=CARTESIAN_POINT('Ctrl Pts',(21.1299851465589,-0.109260984540888,
4.58401866488291));
#40910=CARTESIAN_POINT('Ctrl Pts',(21.1379377859027,-0.20650024671525,4.56582668205621));
#40911=CARTESIAN_POINT('Ctrl Pts',(21.1458904252465,-0.299097442487026,
4.52282205952027));
#40912=CARTESIAN_POINT('Ctrl Pts',(21.1538430645903,-0.375731303474415,
4.46026269810429));
#40913=CARTESIAN_POINT('Ctrl Pts',(21.1617957039341,-0.452365164461805,
4.3977033366883));
#40914=CARTESIAN_POINT('Ctrl Pts',(21.1697483432779,-0.513035690664809,
4.31558923639226));
#40915=CARTESIAN_POINT('Ctrl Pts',(21.1777009826217,-0.550325083965727,
4.22395996434209));
#40916=CARTESIAN_POINT('Ctrl Pts',(21.1856536219655,-0.587614477266646,
4.13233069229192));
#40917=CARTESIAN_POINT('Ctrl Pts',(21.1936062613093,-0.601522737665479,
4.03118624848761));
#40918=CARTESIAN_POINT('Ctrl Pts',(21.2015589006531,-0.590349390887683,
3.93289291874755));
#40919=CARTESIAN_POINT('Ctrl Pts',(21.2095115399969,-0.579176044109886,
3.83459958900749));
#40920=CARTESIAN_POINT('Ctrl Pts',(21.2174641793407,-0.542921090155459,
3.73915737333167));
#40921=CARTESIAN_POINT('Ctrl Pts',(21.2254168186845,-0.486017190935348,
3.65823538248142));
#40922=CARTESIAN_POINT('Ctrl Pts',(21.2333694580283,-0.429113291715238,
3.57731339163117));
#40923=CARTESIAN_POINT('Ctrl Pts',(21.2413220973721,-0.351560447229444,
3.51091162560648));
#40924=CARTESIAN_POINT('Ctrl Pts',(21.249274736716,-0.262840548960938,3.46714860467879));
#40925=CARTESIAN_POINT('Ctrl Pts',(21.2572273760598,-0.174120650692433,
3.4233855837511));
#40926=CARTESIAN_POINT('Ctrl Pts',(21.2651800154036,-0.0742336986412151,
3.40226130792041));
#40927=CARTESIAN_POINT('Ctrl Pts',(21.2731326547474,0.0246077668693877,
3.40635850761334));
#40928=CARTESIAN_POINT('Ctrl Pts',(21.2810852940912,0.123449232380002,3.41045570730627));
#40929=CARTESIAN_POINT('Ctrl Pts',(21.289037933435,0.221245211350001,3.43977438252282));
#40930=CARTESIAN_POINT('Ctrl Pts',(21.2969905727788,0.306038813396919,3.49072992590572));
#40931=CARTESIAN_POINT('Ctrl Pts',(21.3049432121226,0.390832415443818,3.54168546928862));
#40932=CARTESIAN_POINT('Ctrl Pts',(21.3128958514664,0.462623640567642,3.61427788083785));
#40933=CARTESIAN_POINT('Ctrl Pts',(21.3208484908102,0.512635033719562,3.69963174955258));
#40934=CARTESIAN_POINT('Ctrl Pts',(21.328801130154,0.562646426871494,3.78498561826733));
#40935=CARTESIAN_POINT('Ctrl Pts',(21.3367537694978,0.590877988051513,3.88310094414759));
#40936=CARTESIAN_POINT('Ctrl Pts',(21.3447064088416,0.59387802439953,3.98198179230066));
#40937=CARTESIAN_POINT('Ctrl Pts',(21.3526590481854,0.596878060747546,4.08086264045372));
#40938=CARTESIAN_POINT('Ctrl Pts',(21.3606116875293,0.574646572263566,4.1805090108796));
#40939=CARTESIAN_POINT('Ctrl Pts',(21.3685643268731,0.529901661201384,4.26873777763737));
#40940=CARTESIAN_POINT('Ctrl Pts',(21.3765169662169,0.485156750139203,4.35696654439514));
#40941=CARTESIAN_POINT('Ctrl Pts',(21.3844696055607,0.417898416498819,4.4337777074848));
#40942=CARTESIAN_POINT('Ctrl Pts',(21.3924222449045,0.336349907607971,4.48978005607163));
#40943=CARTESIAN_POINT('Ctrl Pts',(21.4003748842483,0.254801398717122,4.54578240465847));
#40944=CARTESIAN_POINT('Ctrl Pts',(21.4083275235921,0.158962714575808,4.58097593874246));
#40945=CARTESIAN_POINT('Ctrl Pts',(21.4162801629359,0.0605514396169286,
4.59105776945554));
#40946=CARTESIAN_POINT('Ctrl Pts',(21.4179049715381,0.0404449719157324,
4.59311759444699));
#40947=CARTESIAN_POINT('Ctrl Pts',(21.4195297801403,0.0202311170044278,
4.59412918598148));
#40948=CARTESIAN_POINT('Ctrl Pts',(21.4211545887425,1.51733402061755E-5,
4.59410821609125));
#40949=CARTESIAN_POINT('Origin',(4.,0.,4.));
#40950=CARTESIAN_POINT('',(21.8288454112575,1.47252919898561E-5,4.59408074293421));
#40951=CARTESIAN_POINT('',(21.7211545887425,-1.54601956517634E-5,4.59410286710644));
#40952=CARTESIAN_POINT('',(4.,-7.27562663373442E-17,4.5941));
#40953=CARTESIAN_POINT('Ctrl Pts',(21.8288454112575,1.47252919898561E-5,
4.59408074293421));
#40954=CARTESIAN_POINT('Ctrl Pts',(21.826505394409,0.0291331941223908,4.59410767674242));
#40955=CARTESIAN_POINT('Ctrl Pts',(21.8241653775604,0.0582478076928112,
4.59200528777341));
#40956=CARTESIAN_POINT('Ctrl Pts',(21.8218253607118,0.0870422430987805,
4.58774093918134));
#40957=CARTESIAN_POINT('Ctrl Pts',(21.813872721368,0.184901264939656,4.57324838268129));
#40958=CARTESIAN_POINT('Ctrl Pts',(21.8059200820242,0.279062206656402,4.53378504179028));
#40959=CARTESIAN_POINT('Ctrl Pts',(21.7979674426804,0.358012610677869,4.47417584741217));
#40960=CARTESIAN_POINT('Ctrl Pts',(21.7900148033366,0.436963014699336,4.41456665303406));
#40961=CARTESIAN_POINT('Ctrl Pts',(21.7820621639928,0.500702881025523,4.33481160516884));
#40962=CARTESIAN_POINT('Ctrl Pts',(21.774109524649,0.541439142878506,4.24466184465998));
#40963=CARTESIAN_POINT('Ctrl Pts',(21.7661568853052,0.58217540473149,4.15451208415111));
#40964=CARTESIAN_POINT('Ctrl Pts',(21.7582042459614,0.599908062111268,4.0539676109986));
#40965=CARTESIAN_POINT('Ctrl Pts',(21.7502516066176,0.59246905613922,3.95532135643358));
#40966=CARTESIAN_POINT('Ctrl Pts',(21.7422989672738,0.585030050167171,3.85667510186855));
#40967=CARTESIAN_POINT('Ctrl Pts',(21.73434632793,0.552419380843296,3.759927065891));
#40968=CARTESIAN_POINT('Ctrl Pts',(21.7263936885861,0.498624146640836,3.67690601358098));
#40969=CARTESIAN_POINT('Ctrl Pts',(21.7184410492423,0.444828912438376,3.59388496127097));
#40970=CARTESIAN_POINT('Ctrl Pts',(21.7104884098985,0.369849113357332,3.52459089262848));
#40971=CARTESIAN_POINT('Ctrl Pts',(21.7025357705547,0.28285205103972,3.47749595131133));
#40972=CARTESIAN_POINT('Ctrl Pts',(21.6945831312109,0.195854988722108,3.43040100999418));
#40973=CARTESIAN_POINT('Ctrl Pts',(21.6866304918671,0.0968406631679286,
3.40550519600236));
#40974=CARTESIAN_POINT('Ctrl Pts',(21.6786778525233,-0.00208507577578169,
3.40585236167057));
#40975=CARTESIAN_POINT('Ctrl Pts',(21.6707252131795,-0.101010814719503,
3.40619952733877));
#40976=CARTESIAN_POINT('Ctrl Pts',(21.6627725738357,-0.199847967052756,
3.431789672667));
#40977=CARTESIAN_POINT('Ctrl Pts',(21.6548199344919,-0.28651234476781,3.47949405385809));
#40978=CARTESIAN_POINT('Ctrl Pts',(21.6468672951481,-0.373176722482865,
3.52719843504918));
#40979=CARTESIAN_POINT('Ctrl Pts',(21.6389146558043,-0.44766832557972,3.59701705210314));
#40980=CARTESIAN_POINT('Ctrl Pts',(21.6309620164605,-0.500879541024521,
3.68041362817464));
#40981=CARTESIAN_POINT('Ctrl Pts',(21.6230093771167,-0.55409075646931,3.76381020424612));
#40982=CARTESIAN_POINT('Ctrl Pts',(21.6150567377728,-0.586021584262053,
3.86078473933514));
#40983=CARTESIAN_POINT('Ctrl Pts',(21.607104098429,-0.592768045815946,3.95948077576042));
#40984=CARTESIAN_POINT('Ctrl Pts',(21.5991514590852,-0.599514507369841,
4.05817681218572));
#40985=CARTESIAN_POINT('Ctrl Pts',(21.5911988197414,-0.581076602684875,
4.15859434994728));
#40986=CARTESIAN_POINT('Ctrl Pts',(21.5832461803976,-0.539708616728004,
4.24845597739434));
#40987=CARTESIAN_POINT('Ctrl Pts',(21.5752935410538,-0.498340630771147,
4.33831760484137));
#40988=CARTESIAN_POINT('Ctrl Pts',(21.56734090171,-0.434042563542403,4.41762332197391));
#40989=CARTESIAN_POINT('Ctrl Pts',(21.5593882623662,-0.354675729482573,
4.47667692475034));
#40990=CARTESIAN_POINT('Ctrl Pts',(21.5514356230224,-0.275308895422716,
4.53573052752678));
#40991=CARTESIAN_POINT('Ctrl Pts',(21.5434829836786,-0.180873294531764,
4.57453201594709));
#40992=CARTESIAN_POINT('Ctrl Pts',(21.5355303443348,-0.0829149652056982,
4.58833737958621));
#40993=CARTESIAN_POINT('Ctrl Pts',(21.533302033309,-0.055467269432644,4.59220561033096));
#40994=CARTESIAN_POINT('Ctrl Pts',(21.5310737222833,-0.0277430016607059,
4.5941113769453));
#40995=CARTESIAN_POINT('Ctrl Pts',(21.5288454112575,-1.51073027558624E-5,
4.59408477831653));
#40996=CARTESIAN_POINT('Ctrl Pts',(21.4211545887425,1.51733402061755E-5,
4.59410821609125));
#40997=CARTESIAN_POINT('Ctrl Pts',(21.4274824194841,-0.0787159889745399,
4.59402654867773));
#40998=CARTESIAN_POINT('Ctrl Pts',(21.4338102502257,-0.15747883181342,4.57828382012605));
#40999=CARTESIAN_POINT('Ctrl Pts',(21.4401380809673,-0.230053504748576,
4.54780575811717));
#41000=CARTESIAN_POINT('Ctrl Pts',(21.4480907203111,-0.321263308378747,
4.50950178872359));
#41001=CARTESIAN_POINT('Ctrl Pts',(21.4560433596549,-0.402699049862651,
4.44792372259427));
#41002=CARTESIAN_POINT('Ctrl Pts',(21.4639959989987,-0.464404100671371,
4.37060031698995));
#41003=CARTESIAN_POINT('Ctrl Pts',(21.4719486383425,-0.526109151480106,
4.2932769113856));
#41004=CARTESIAN_POINT('Ctrl Pts',(21.4799012776864,-0.568083511613643,
4.20020816630624));
#41005=CARTESIAN_POINT('Ctrl Pts',(21.4878539170302,-0.585195243866348,
4.10277300340868));
#41006=CARTESIAN_POINT('Ctrl Pts',(21.495806556374,-0.602306976119048,4.00533784051114));
#41007=CARTESIAN_POINT('Ctrl Pts',(21.5037591957178,-0.594556080490919,
3.90353625979537));
#41008=CARTESIAN_POINT('Ctrl Pts',(21.5117118350616,-0.562890209537588,
3.80981489101362));
#41009=CARTESIAN_POINT('Ctrl Pts',(21.5196644744054,-0.53122433858425,3.71609352223184));
#41010=CARTESIAN_POINT('Ctrl Pts',(21.5276171137492,-0.47564349230572,3.63045236538409));
#41011=CARTESIAN_POINT('Ctrl Pts',(21.535569753093,-0.402943186155437,3.56336221830407));
#41012=CARTESIAN_POINT('Ctrl Pts',(21.5435223924368,-0.330242880005154,
3.49627207122406));
#41013=CARTESIAN_POINT('Ctrl Pts',(21.5514750317806,-0.24042311398314,3.44773293391182));
#41014=CARTESIAN_POINT('Ctrl Pts',(21.5594276711244,-0.144465577806233,
3.42367937699355));
#41015=CARTESIAN_POINT('Ctrl Pts',(21.5673803104682,-0.0485080416293372,
3.39962582007528));
#41016=CARTESIAN_POINT('Ctrl Pts',(21.575332949812,0.0535872647024426,3.40005784355098));
#41017=CARTESIAN_POINT('Ctrl Pts',(21.5832855891558,0.149337799479898,3.42492262666669));
#41018=CARTESIAN_POINT('Ctrl Pts',(21.5912382284996,0.245088334257342,3.44978740978241));
#41019=CARTESIAN_POINT('Ctrl Pts',(21.5991908678434,0.33449409748049,3.49908495253815));
#41020=CARTESIAN_POINT('Ctrl Pts',(21.6071435071872,0.406624016913212,3.56678795891296));
#41021=CARTESIAN_POINT('Ctrl Pts',(21.6150961465311,0.478753936345942,3.63449096528778));
#41022=CARTESIAN_POINT('Ctrl Pts',(21.6230487858749,0.533608011988269,3.72059943528167));
#41023=CARTESIAN_POINT('Ctrl Pts',(21.6310014252187,0.564479585995414,3.81458543566408));
#41024=CARTESIAN_POINT('Ctrl Pts',(21.6389540645625,0.595351160002559,3.90857143604649));
#41025=CARTESIAN_POINT('Ctrl Pts',(21.6469067039063,0.602240232374519,4.0104349668174));
#41026=CARTESIAN_POINT('Ctrl Pts',(21.6548593432501,0.584304520186539,4.10772182398666));
#41027=CARTESIAN_POINT('Ctrl Pts',(21.6628119825939,0.566368807998562,4.2050086811559));
#41028=CARTESIAN_POINT('Ctrl Pts',(21.6707646219377,0.523608311250652,4.29771886472347));
#41029=CARTESIAN_POINT('Ctrl Pts',(21.6787172612815,0.461251083056512,4.37451729206089));
#41030=CARTESIAN_POINT('Ctrl Pts',(21.6866699006253,0.398893854862358,4.45131571939834));
#41031=CARTESIAN_POINT('Ctrl Pts',(21.6946225399691,0.316939895221968,4.51220239050563));
#41032=CARTESIAN_POINT('Ctrl Pts',(21.7025751793129,0.225409191891896,4.54973308058009));
#41033=CARTESIAN_POINT('Ctrl Pts',(21.7087683157894,0.15412944274098,4.5789601931952));
#41034=CARTESIAN_POINT('Ctrl Pts',(21.7149614522659,0.0770418275534371,
4.59402294959611));
#41035=CARTESIAN_POINT('Ctrl Pts',(21.7211545887425,-1.54601956517634E-5,
4.59410286710644));
#41036=CARTESIAN_POINT('Origin',(4.,0.,4.));
#41037=CARTESIAN_POINT('',(22.1288454112575,-1.19684274697274E-5,4.59413016891312));
#41038=CARTESIAN_POINT('',(22.0211545887425,1.20066176157995E-5,4.59406577061205));
#41039=CARTESIAN_POINT('',(4.,-7.27562663373442E-17,4.5941));
#41040=CARTESIAN_POINT('Ctrl Pts',(22.1288454112575,-1.19684274697274E-5,
4.59413016891312));
#41041=CARTESIAN_POINT('Ctrl Pts',(22.1219370665346,0.0859328098890183,
4.59405244111828));
#41042=CARTESIAN_POINT('Ctrl Pts',(22.1150287218117,0.171910584533005,4.57519344187135));
#41043=CARTESIAN_POINT('Ctrl Pts',(22.1081203770888,0.24987714748571,4.53905210772026));
#41044=CARTESIAN_POINT('Ctrl Pts',(22.100167737745,0.339629466009183,4.49744749656716));
#41045=CARTESIAN_POINT('Ctrl Pts',(22.0922150984012,0.418765494330909,4.4329406966096));
#41046=CARTESIAN_POINT('Ctrl Pts',(22.0842624590574,0.477609775176754,4.35341854270704));
#41047=CARTESIAN_POINT('Ctrl Pts',(22.0763098197136,0.536454056022584,4.2738963888045));
#41048=CARTESIAN_POINT('Ctrl Pts',(22.0683571803698,0.575006589392542,4.17935888095698));
#41049=CARTESIAN_POINT('Ctrl Pts',(22.060404541026,0.588553803007579,4.081364517074));
#41050=CARTESIAN_POINT('Ctrl Pts',(22.0524519016822,0.60210101662262,3.983370153191));
#41051=CARTESIAN_POINT('Ctrl Pts',(22.0444992623384,0.590642910482727,3.88191893327255));
#41052=CARTESIAN_POINT('Ctrl Pts',(22.0365466229946,0.55558039411957,3.78941465069146));
#41053=CARTESIAN_POINT('Ctrl Pts',(22.0285939836508,0.520517877756421,3.69691036811039));
#41054=CARTESIAN_POINT('Ctrl Pts',(22.020641344307,0.461850951170019,3.61335302286667));
#41055=CARTESIAN_POINT('Ctrl Pts',(22.0126887049632,0.386752445163155,3.5489586384446));
#41056=CARTESIAN_POINT('Ctrl Pts',(22.0047360656194,0.311653939156274,3.48456425402251));
#41057=CARTESIAN_POINT('Ctrl Pts',(21.9967834262756,0.220123853728924,3.43933283042207));
#41058=CARTESIAN_POINT('Ctrl Pts',(21.9888307869318,0.123352988439278,3.41879452521803));
#41059=CARTESIAN_POINT('Ctrl Pts',(21.980878147588,0.0265821231496428,3.398256220014));
#41060=CARTESIAN_POINT('Ctrl Pts',(21.9729255082441,-0.075429522002288,
3.40241103320635));
#41061=CARTESIAN_POINT('Ctrl Pts',(21.9649728689003,-0.170209634025949,
3.43075098229493));
#41062=CARTESIAN_POINT('Ctrl Pts',(21.9570202295565,-0.26498974604961,3.4590909313835));
#41063=CARTESIAN_POINT('Ctrl Pts',(21.9490675902127,-0.352538324945002,
3.5116160163683));
#41064=CARTESIAN_POINT('Ctrl Pts',(21.9411149508689,-0.422151364554475,
3.58190433023263));
#41065=CARTESIAN_POINT('Ctrl Pts',(21.9331623115251,-0.491764404163956,
3.65219264409696));
#41066=CARTESIAN_POINT('Ctrl Pts',(21.9252096721813,-0.543441904487514,
3.74024418684083));
#41067=CARTESIAN_POINT('Ctrl Pts',(21.9172570328375,-0.570865587277161,
3.83529345812586));
#41068=CARTESIAN_POINT('Ctrl Pts',(21.9093043934937,-0.598289270066803,
3.93034272941087));
#41069=CARTESIAN_POINT('Ctrl Pts',(21.9013517541499,-0.601459135322544,
4.03238972923704));
#41070=CARTESIAN_POINT('Ctrl Pts',(21.8933991148061,-0.579987623844179,
4.12895782202339));
#41071=CARTESIAN_POINT('Ctrl Pts',(21.8854464754623,-0.558516112365809,
4.22552591480976));
#41072=CARTESIAN_POINT('Ctrl Pts',(21.8774938361185,-0.512403224153321,
4.31661510055631));
#41073=CARTESIAN_POINT('Ctrl Pts',(21.8695411967747,-0.447286887835617,
4.39108848569571));
#41074=CARTESIAN_POINT('Ctrl Pts',(21.8615885574308,-0.38217055151792,4.46556187083511));
#41075=CARTESIAN_POINT('Ctrl Pts',(21.853635918087,-0.298050767095013,4.52341945536736));
#41076=CARTESIAN_POINT('Ctrl Pts',(21.8456832787432,-0.205212323901057,
4.55758736157894));
#41077=CARTESIAN_POINT('Ctrl Pts',(21.840070656248,-0.139691040693493,4.58170156451555));
#41078=CARTESIAN_POINT('Ctrl Pts',(21.8344580337528,-0.0698270680627233,
4.59401614113532));
#41079=CARTESIAN_POINT('Ctrl Pts',(21.8288454112575,1.47252919898561E-5,
4.59408074293421));
#41080=CARTESIAN_POINT('Ctrl Pts',(21.7211545887425,-1.54601956517634E-5,
4.59410286710644));
#41081=CARTESIAN_POINT('Ctrl Pts',(21.7229140916097,-0.0219078436841643,
4.59412557209431));
#41082=CARTESIAN_POINT('Ctrl Pts',(21.724673594477,-0.0437977792686499,
4.59293892497318));
#41083=CARTESIAN_POINT('Ctrl Pts',(21.7264330973443,-0.0655513867134097,
4.59052415646896));
#41084=CARTESIAN_POINT('Ctrl Pts',(21.7343857366881,-0.163873814968881,
4.57960983324176));
#41085=CARTESIAN_POINT('Ctrl Pts',(21.742338376032,-0.259411224460086,4.54360647774573));
#41086=CARTESIAN_POINT('Ctrl Pts',(21.7502910153758,-0.340482865683332,
4.48691599054611));
#41087=CARTESIAN_POINT('Ctrl Pts',(21.7582436547196,-0.421554506906578,
4.4302255033465));
#41088=CARTESIAN_POINT('Ctrl Pts',(21.7661962940634,-0.488160379861865,
4.3528478844433));
#41089=CARTESIAN_POINT('Ctrl Pts',(21.7741489334072,-0.532157009426634,
4.26424360160945));
#41090=CARTESIAN_POINT('Ctrl Pts',(21.782101572751,-0.576153638991403,4.1756393187756));
#41091=CARTESIAN_POINT('Ctrl Pts',(21.7900542120948,-0.597541025165654,
4.0758083720111));
#41092=CARTESIAN_POINT('Ctrl Pts',(21.7980068514386,-0.593704268699233,
3.9769564542281));
#41093=CARTESIAN_POINT('Ctrl Pts',(21.8059594907824,-0.589867512232813,
3.87810453644509));
#41094=CARTESIAN_POINT('Ctrl Pts',(21.8139121301262,-0.560806613125721,
3.78023164764359));
#41095=CARTESIAN_POINT('Ctrl Pts',(21.82186476947,-0.510074662095298,3.69530408148155));
#41096=CARTESIAN_POINT('Ctrl Pts',(21.8298174088138,-0.459342711064876,
3.61037651531951));
#41097=CARTESIAN_POINT('Ctrl Pts',(21.8377700481576,-0.386939708111122,
3.53839427179695));
#41098=CARTESIAN_POINT('Ctrl Pts',(21.8457226875014,-0.301717906454235,
3.48815816056295));
#41099=CARTESIAN_POINT('Ctrl Pts',(21.8536753268452,-0.216496104797349,
3.43792204932895));
#41100=CARTESIAN_POINT('Ctrl Pts',(21.8616279661891,-0.118455504437329,
3.40943207038352));
#41101=CARTESIAN_POINT('Ctrl Pts',(21.8695806055329,-0.0195829040543552,
3.40617151167847));
#41102=CARTESIAN_POINT('Ctrl Pts',(21.8775332448767,0.0792896963286298,
3.40291095297342));
#41103=CARTESIAN_POINT('Ctrl Pts',(21.8854858842205,0.178994296734569,3.42487981450875));
#41104=CARTESIAN_POINT('Ctrl Pts',(21.8934385235643,0.267340651814441,3.46939210375187));
#41105=CARTESIAN_POINT('Ctrl Pts',(21.9013911629081,0.355687006894294,3.51390439299499));
#41106=CARTESIAN_POINT('Ctrl Pts',(21.9093438022519,0.432675116648084,3.58096010994589));
#41107=CARTESIAN_POINT('Ctrl Pts',(21.9172964415957,0.488892136101412,3.66236077992681));
#41108=CARTESIAN_POINT('Ctrl Pts',(21.9252490809395,0.545109155554752,3.74376144990775));
#41109=CARTESIAN_POINT('Ctrl Pts',(21.9332017202833,0.580555084707621,3.8395070729187));
#41110=CARTESIAN_POINT('Ctrl Pts',(21.9411543596271,0.590896175957217,3.93789144251738));
#41111=CARTESIAN_POINT('Ctrl Pts',(21.9491069989709,0.601237267206812,4.03627581211605));
#41112=CARTESIAN_POINT('Ctrl Pts',(21.9570596383147,0.58647352055314,4.13729892830245));
#41113=CARTESIAN_POINT('Ctrl Pts',(21.9650122776585,0.548410005102802,4.22860933921557));
#41114=CARTESIAN_POINT('Ctrl Pts',(21.9729649170023,0.510346489652465,4.31991975012869));
#41115=CARTESIAN_POINT('Ctrl Pts',(21.9809175563462,0.448983205405461,4.40151745576853));
#41116=CARTESIAN_POINT('Ctrl Pts',(21.98887019569,0.371822649612145,4.46342602528218));
#41117=CARTESIAN_POINT('Ctrl Pts',(21.9968228350338,0.29466209381883,4.52533459479583));
#41118=CARTESIAN_POINT('Ctrl Pts',(22.0047754743776,0.201704266479203,4.5675540281833));
#41119=CARTESIAN_POINT('Ctrl Pts',(22.0127281137214,0.104314528045707,4.58492242469582));
#41120=CARTESIAN_POINT('Ctrl Pts',(22.0155369387284,0.069917050565085,4.59105683924014));
#41121=CARTESIAN_POINT('Ctrl Pts',(22.0183457637354,0.0349667096964542,
4.59409118517947));
#41122=CARTESIAN_POINT('Ctrl Pts',(22.0211545887425,1.20066176157995E-5,
4.59406577061205));
#41123=CARTESIAN_POINT('Origin',(4.,0.,4.));
#41124=CARTESIAN_POINT('',(22.4288454112575,5.18920962550018E-6,4.59405135764298));
#41125=CARTESIAN_POINT('',(22.3211545887424,-7.30827440488969E-6,4.59414400810326));
#41126=CARTESIAN_POINT('',(4.,-7.27562663373442E-17,4.5941));
#41127=CARTESIAN_POINT('Ctrl Pts',(22.4288454112575,5.18920962550018E-6,
4.59405135764298));
#41128=CARTESIAN_POINT('Ctrl Pts',(22.4253213780041,0.0438634191921666,
4.5940647188338));
#41129=CARTESIAN_POINT('Ctrl Pts',(22.4217973447507,0.0877187745911938,
4.589273164082));
#41130=CARTESIAN_POINT('Ctrl Pts',(22.4182733114973,0.130485535360993,4.57964583089408));
#41131=CARTESIAN_POINT('Ctrl Pts',(22.4103206721535,0.226996720088313,4.55791995512033));
#41132=CARTESIAN_POINT('Ctrl Pts',(22.4023680328097,0.317964089339764,4.51156722320365));
#41133=CARTESIAN_POINT('Ctrl Pts',(22.3944153934659,0.392265646131591,4.44625488916104));
#41134=CARTESIAN_POINT('Ctrl Pts',(22.3864627541221,0.4665672029234,4.38094255511845));
#41135=CARTESIAN_POINT('Ctrl Pts',(22.3785101147783,0.524202947255594,4.29667061894994));
#41136=CARTESIAN_POINT('Ctrl Pts',(22.3705574754345,0.558126122886914,4.20374247196213));
#41137=CARTESIAN_POINT('Ctrl Pts',(22.3626048360906,0.592049298518242,4.11081432497429));
#41138=CARTESIAN_POINT('Ctrl Pts',(22.3546521967468,0.602259905448686,4.00922996716717));
#41139=CARTESIAN_POINT('Ctrl Pts',(22.346699557403,0.587509558716917,3.91140947017845));
#41140=CARTESIAN_POINT('Ctrl Pts',(22.3387469180592,0.572759211985149,3.81358897318973));
#41141=CARTESIAN_POINT('Ctrl Pts',(22.3307942787154,0.533047911591167,3.71953233701942));
#41142=CARTESIAN_POINT('Ctrl Pts',(22.3228416393716,0.473230904440663,3.6407392662825));
#41143=CARTESIAN_POINT('Ctrl Pts',(22.3148890000278,0.413413897290173,3.5619461955456));
#41144=CARTESIAN_POINT('Ctrl Pts',(22.306936360684,0.333491183383171,3.49841669024209));
#41145=CARTESIAN_POINT('Ctrl Pts',(22.2989837213402,0.243234403245124,3.45791809774646));
#41146=CARTESIAN_POINT('Ctrl Pts',(22.2910310819964,0.152977623107077,3.41741950525082));
#41147=CARTESIAN_POINT('Ctrl Pts',(22.2830784426526,0.0523867767379842,
3.39995182556307));
#41148=CARTESIAN_POINT('Ctrl Pts',(22.2751258033088,-0.0462395349927855,
3.40765072037886));
#41149=CARTESIAN_POINT('Ctrl Pts',(22.267173163965,-0.144865846723578,3.41534961519466));
#41150=CARTESIAN_POINT('Ctrl Pts',(22.2592205246212,-0.241527623816046,
3.448215084514));
#41151=CARTESIAN_POINT('Ctrl Pts',(22.2512678852774,-0.324406647450603,
3.50222887712101));
#41152=CARTESIAN_POINT('Ctrl Pts',(22.2433152459336,-0.40728567108515,3.55624266972802));
#41153=CARTESIAN_POINT('Ctrl Pts',(22.2353626065897,-0.476381941261788,
3.63140478562268));
#41154=CARTESIAN_POINT('Ctrl Pts',(22.2274099672459,-0.523247497912515,
3.71852563243507));
#41155=CARTESIAN_POINT('Ctrl Pts',(22.2194573279021,-0.570113054563243,
3.80564647924745));
#41156=CARTESIAN_POINT('Ctrl Pts',(22.2115046885583,-0.59474789768806,3.90472605697756));
#41157=CARTESIAN_POINT('Ctrl Pts',(22.2035520492145,-0.594140082177443,
4.00365053781872));
#41158=CARTESIAN_POINT('Ctrl Pts',(22.1955994098707,-0.593532266666827,
4.10257501865988));
#41159=CARTESIAN_POINT('Ctrl Pts',(22.1876467705269,-0.567681792520777,
4.2013444026121));
#41160=CARTESIAN_POINT('Ctrl Pts',(22.1796941311831,-0.519749232289404,
4.2878827872712));
#41161=CARTESIAN_POINT('Ctrl Pts',(22.1717414918393,-0.471816672058032,
4.37442117193029));
#41162=CARTESIAN_POINT('Ctrl Pts',(22.1637888524955,-0.401802025741336,
4.44872855729627));
#41163=CARTESIAN_POINT('Ctrl Pts',(22.1558362131517,-0.318265537426909,
4.50171985346399));
#41164=CARTESIAN_POINT('Ctrl Pts',(22.1478835738079,-0.234729049112483,
4.55471114963171));
#41165=CARTESIAN_POINT('Ctrl Pts',(22.1399309344641,-0.137670718800326,
4.58638635660118));
#41166=CARTESIAN_POINT('Ctrl Pts',(22.1319782951203,-0.0389572492816432,
4.5928727489116));
#41167=CARTESIAN_POINT('Ctrl Pts',(22.1309340004994,-0.0259947671705595,
4.5937245044491));
#41168=CARTESIAN_POINT('Ctrl Pts',(22.1298897058784,-0.0130037447923657,
4.5941419185755));
#41169=CARTESIAN_POINT('Ctrl Pts',(22.1288454112575,-1.19684274697274E-5,
4.59413016891312));
#41170=CARTESIAN_POINT('Ctrl Pts',(22.0211545887425,1.20066176157995E-5,
4.59406577061205));
#41171=CARTESIAN_POINT('Ctrl Pts',(22.0262984030792,-0.064000704172389,
4.59401922879619));
#41172=CARTESIAN_POINT('Ctrl Pts',(22.031442217416,-0.128028044405449,4.5837112392356));
#41173=CARTESIAN_POINT('Ctrl Pts',(22.0365860317528,-0.188701337098646,
4.56338935830438));
#41174=CARTESIAN_POINT('Ctrl Pts',(22.0445386710966,-0.282505814282095,
4.53197053576284));
#41175=CARTESIAN_POINT('Ctrl Pts',(22.0524913104404,-0.368293119121642,
4.4766155310422));
#41176=CARTESIAN_POINT('Ctrl Pts',(22.0604439497842,-0.435574585201076,
4.40409224738955));
#41177=CARTESIAN_POINT('Ctrl Pts',(22.068396589128,-0.502856051280518,4.33156896373689));
#41178=CARTESIAN_POINT('Ctrl Pts',(22.0763492284718,-0.551631678599843,
4.24187740115222));
#41179=CARTESIAN_POINT('Ctrl Pts',(22.0843018678156,-0.575937982408454,
4.14598357473613));
#41180=CARTESIAN_POINT('Ctrl Pts',(22.0922545071594,-0.600244286217068,
4.05008974832002));
#41181=CARTESIAN_POINT('Ctrl Pts',(22.1002071465032,-0.600081266514962,
3.94799365807249));
#41182=CARTESIAN_POINT('Ctrl Pts',(22.1081597858471,-0.575468854681199,
3.85217794154701));
#41183=CARTESIAN_POINT('Ctrl Pts',(22.1161124251909,-0.550856442847438,
3.75636222502155));
#41184=CARTESIAN_POINT('Ctrl Pts',(22.1240650645347,-0.501794638882025,
3.66682688221814));
#41185=CARTESIAN_POINT('Ctrl Pts',(22.1320177038785,-0.434281916527717,
3.5945188282416));
#41186=CARTESIAN_POINT('Ctrl Pts',(22.1399703432223,-0.366769194173409,
3.52221077426505));
#41187=CARTESIAN_POINT('Ctrl Pts',(22.1479229825661,-0.280805553430205,
3.46713000911538));
#41188=CARTESIAN_POINT('Ctrl Pts',(22.1558756219099,-0.186901220180937,
3.43601090651668));
#41189=CARTESIAN_POINT('Ctrl Pts',(22.1638282612537,-0.0929968869316588,
3.40489180391798));
#41190=CARTESIAN_POINT('Ctrl Pts',(22.1717809005975,0.00884813882368474,
3.39773436387026));
#41191=CARTESIAN_POINT('Ctrl Pts',(22.1797335399413,0.106181915586414,3.41541368090248));
#41192=CARTESIAN_POINT('Ctrl Pts',(22.1876861792851,0.203515692349121,3.4330929979347));
#41193=CARTESIAN_POINT('Ctrl Pts',(22.1956388186289,0.296338220119215,3.47560907204686));
#41194=CARTESIAN_POINT('Ctrl Pts',(22.2035914579727,0.373300680656879,3.53776373412001));
#41195=CARTESIAN_POINT('Ctrl Pts',(22.2115440973165,0.450263141194552,3.59991839619317));
#41196=CARTESIAN_POINT('Ctrl Pts',(22.2194967366603,0.511365534499791,3.68171164622733));
#41197=CARTESIAN_POINT('Ctrl Pts',(22.2274493760041,0.549137260797828,3.7731431454068));
#41198=CARTESIAN_POINT('Ctrl Pts',(22.2354020153479,0.586908987095865,3.86457464458628));
#41199=CARTESIAN_POINT('Ctrl Pts',(22.2433546546918,0.6013500463867,3.96564439291107));
#41200=CARTESIAN_POINT('Ctrl Pts',(22.2513072940356,0.590694822479903,4.06399523710107));
#41201=CARTESIAN_POINT('Ctrl Pts',(22.2592599333794,0.580039598573106,4.16234608129106));
#41202=CARTESIAN_POINT('Ctrl Pts',(22.2672125727232,0.544288091468676,4.25797802134625));
#41203=CARTESIAN_POINT('Ctrl Pts',(22.275165212067,0.487811409852587,4.33919875012361));
#41204=CARTESIAN_POINT('Ctrl Pts',(22.2831178514108,0.431334728236497,4.42041947890096));
#41205=CARTESIAN_POINT('Ctrl Pts',(22.2910704907546,0.354132872108749,4.48722899640046));
#41206=CARTESIAN_POINT('Ctrl Pts',(22.2990231300984,0.265644819817582,4.53145892916239));
#41207=CARTESIAN_POINT('Ctrl Pts',(22.3064002829798,0.183560135512932,4.57248819778762));
#41208=CARTESIAN_POINT('Ctrl Pts',(22.3137774358611,0.0917635873240076,
4.59408754951618));
#41209=CARTESIAN_POINT('Ctrl Pts',(22.3211545887424,-7.30827440488969E-6,
4.59414400810326));
#41210=CARTESIAN_POINT('Origin',(4.,0.,4.));
#41211=CARTESIAN_POINT('',(22.7288454112575,-7.11440487624268E-7,4.59414971000239));
#41212=CARTESIAN_POINT('',(22.6211545887425,-1.51245797256638E-7,4.59404869726453));
#41213=CARTESIAN_POINT('',(4.,-7.27562663373442E-17,4.5941));
#41214=CARTESIAN_POINT('Ctrl Pts',(22.7288454112575,-7.11440487624268E-7,
4.59414971000239));
#41215=CARTESIAN_POINT('Ctrl Pts',(22.7287056894736,0.0017373052546791,
4.59414999869406));
#41216=CARTESIAN_POINT('Ctrl Pts',(22.7285659676897,0.0034753215591825,
4.59414251282321));
#41217=CARTESIAN_POINT('Ctrl Pts',(22.7284262459057,0.00521327185949689,
4.59412723628209));
#41218=CARTESIAN_POINT('Ctrl Pts',(22.7204736065619,0.104133365400505,4.59325773105135));
#41219=CARTESIAN_POINT('Ctrl Pts',(22.7125209672181,0.202839630323109,4.56714939948764));
#41220=CARTESIAN_POINT('Ctrl Pts',(22.7045683278743,0.289252680684759,4.51898953373575));
#41221=CARTESIAN_POINT('Ctrl Pts',(22.6966156885305,0.375665731046408,4.47082966798385));
#41222=CARTESIAN_POINT('Ctrl Pts',(22.6886630491867,0.449785566847107,4.40061826804377));
#41223=CARTESIAN_POINT('Ctrl Pts',(22.6807104098429,0.502555912967013,4.31694216252228));
#41224=CARTESIAN_POINT('Ctrl Pts',(22.6727577704991,0.555326259086918,4.23326605700079));
#41225=CARTESIAN_POINT('Ctrl Pts',(22.6648051311553,0.586747115526033,4.13612524589788));
#41226=CARTESIAN_POINT('Ctrl Pts',(22.6568524918115,0.592973744123511,4.03739517928057));
#41227=CARTESIAN_POINT('Ctrl Pts',(22.6488998524677,0.59920037272099,3.93866511266326));
#41228=CARTESIAN_POINT('Ctrl Pts',(22.6409472131239,0.580232773476834,3.83834579053153));
#41229=CARTESIAN_POINT('Ctrl Pts',(22.6329945737801,0.538391640361539,3.74870332422701));
#41230=CARTESIAN_POINT('Ctrl Pts',(22.6250419344363,0.496550507246239,3.65906085792248));
#41231=CARTESIAN_POINT('Ctrl Pts',(22.6170892950925,0.431835840259791,3.58009524744515));
#41232=CARTESIAN_POINT('Ctrl Pts',(22.6091366557487,0.35215901686313,3.52146073929621));
#41233=CARTESIAN_POINT('Ctrl Pts',(22.6011840164048,0.272482193466486,3.46282623114728));
#41234=CARTESIAN_POINT('Ctrl Pts',(22.593231377061,0.17784321365963,3.42452282532672));
#41235=CARTESIAN_POINT('Ctrl Pts',(22.5852787377172,0.0798134434713266,
3.41123383340666));
#41236=CARTESIAN_POINT('Ctrl Pts',(22.5773260983734,-0.0182163267169884,
3.3979448414866));
#41237=CARTESIAN_POINT('Ctrl Pts',(22.5693734590296,-0.119636887286728,
3.40967026346704));
#41238=CARTESIAN_POINT('Ctrl Pts',(22.5614208196858,-0.212048437952692,
3.44497640167274));
#41239=CARTESIAN_POINT('Ctrl Pts',(22.553468180342,-0.304459988618666,3.48028253987845));
#41240=CARTESIAN_POINT('Ctrl Pts',(22.5455155409982,-0.387862529380837,
3.53916939430943));
#41241=CARTESIAN_POINT('Ctrl Pts',(22.5375629016544,-0.452058834188948,
3.61443730067171));
#41242=CARTESIAN_POINT('Ctrl Pts',(22.5296102623106,-0.516255138997059,
3.689705207034));
#41243=CARTESIAN_POINT('Ctrl Pts',(22.5216576229668,-0.561245207851117,
3.7813541653276));
#41244=CARTESIAN_POINT('Ctrl Pts',(22.513704983623,-0.581528460676763,3.87817881267738));
#41245=CARTESIAN_POINT('Ctrl Pts',(22.5057523442792,-0.601811713502406,
3.97500346002715));
#41246=CARTESIAN_POINT('Ctrl Pts',(22.4977997049354,-0.597388150299644,
4.07700379643311));
#41247=CARTESIAN_POINT('Ctrl Pts',(22.4898470655916,-0.568798575589296,
4.17170890717095));
#41248=CARTESIAN_POINT('Ctrl Pts',(22.4818944262477,-0.540209000878948,
4.26641401790879));
#41249=CARTESIAN_POINT('Ctrl Pts',(22.4739417869039,-0.487453414661012,
4.35382390297851));
#41250=CARTESIAN_POINT('Ctrl Pts',(22.4659891475601,-0.416981925106977,
4.42325150516024));
#41251=CARTESIAN_POINT('Ctrl Pts',(22.4580365082163,-0.346510435552941,
4.49267910734197));
#41252=CARTESIAN_POINT('Ctrl Pts',(22.4500838688725,-0.258323042662803,
4.54412442663572));
#41253=CARTESIAN_POINT('Ctrl Pts',(22.4421312295287,-0.163201846116148,
4.57129757646718));
#41254=CARTESIAN_POINT('Ctrl Pts',(22.4377026234383,-0.11023146834083,4.58642955613285));
#41255=CARTESIAN_POINT('Ctrl Pts',(22.4332740173479,-0.0551108697057404,
4.59403456681078));
#41256=CARTESIAN_POINT('Ctrl Pts',(22.4288454112575,5.18920962550018E-6,
4.59405135764298));
#41257=CARTESIAN_POINT('Ctrl Pts',(22.3211545887424,-7.30827440488969E-6,
4.59414400810326));
#41258=CARTESIAN_POINT('Ctrl Pts',(22.3217300752049,-0.00716629073194701,
4.59414841239758));
#41259=CARTESIAN_POINT('Ctrl Pts',(22.3223055616673,-0.0143251170819474,
4.59402171850555));
#41260=CARTESIAN_POINT('Ctrl Pts',(22.3228810481298,-0.0214791647150919,
4.59376292335171));
#41261=CARTESIAN_POINT('Ctrl Pts',(22.3308336874736,-0.120340848501978,
4.59018663675477));
#41262=CARTESIAN_POINT('Ctrl Pts',(22.3387863268174,-0.218289967621164,
4.56138371553656));
#41263=CARTESIAN_POINT('Ctrl Pts',(22.3467389661612,-0.303350908332583,
4.51087570903952));
#41264=CARTESIAN_POINT('Ctrl Pts',(22.3546916055051,-0.388411849044011,
4.46036770254246));
#41265=CARTESIAN_POINT('Ctrl Pts',(22.3626442448489,-0.460584611347669,
4.38815461076656));
#41266=CARTESIAN_POINT('Ctrl Pts',(22.3705968841927,-0.511045091866278,
4.3030654678256));
#41267=CARTESIAN_POINT('Ctrl Pts',(22.3785495235365,-0.561505572384874,
4.21797632488466));
#41268=CARTESIAN_POINT('Ctrl Pts',(22.3865021628803,-0.590253771118432,
4.12001113077866));
#41269=CARTESIAN_POINT('Ctrl Pts',(22.3944548022241,-0.593774829630164,
4.02114746451658));
#41270=CARTESIAN_POINT('Ctrl Pts',(22.4024074415679,-0.597295888141896,
3.92228379825449));
#41271=CARTESIAN_POINT('Ctrl Pts',(22.4103600809117,-0.575589806431797,
3.82252165983632));
#41272=CARTESIAN_POINT('Ctrl Pts',(22.4183127202555,-0.531310447862662,
3.73405832985033));
#41273=CARTESIAN_POINT('Ctrl Pts',(22.4262653595993,-0.487031089293526,
3.64559499986435));
#41274=CARTESIAN_POINT('Ctrl Pts',(22.4342179989431,-0.420178453865353,
3.56843047831055));
#41275=CARTESIAN_POINT('Ctrl Pts',(22.4421706382869,-0.338926188203527,
3.51199917808983));
#41276=CARTESIAN_POINT('Ctrl Pts',(22.4501232776307,-0.257673922541701,
3.45556787786912));
#41277=CARTESIAN_POINT('Ctrl Pts',(22.4580759169745,-0.162022026646223,
3.41986979898149));
#41278=CARTESIAN_POINT('Ctrl Pts',(22.4660285563183,-0.0636652448434586,
3.40926951931498));
#41279=CARTESIAN_POINT('Ctrl Pts',(22.4739811956621,0.0346915369593057,
3.39866923964846));
#41280=CARTESIAN_POINT('Ctrl Pts',(22.4819338350059,0.135753204669356,3.41316675920307));
#41281=CARTESIAN_POINT('Ctrl Pts',(22.4898864743497,0.227163587879617,3.45098955584192));
#41282=CARTESIAN_POINT('Ctrl Pts',(22.4978391136936,0.318573971089878,3.48881235248077));
#41283=CARTESIAN_POINT('Ctrl Pts',(22.5057917530374,0.40033306980035,3.54996042620388));
#41284=CARTESIAN_POINT('Ctrl Pts',(22.5137443923812,0.462444730281743,3.62695759769032));
#41285=CARTESIAN_POINT('Ctrl Pts',(22.521697031725,0.524556390763143,3.70395476917678));
#41286=CARTESIAN_POINT('Ctrl Pts',(22.5296496710688,0.567020613015458,3.79680103842659));
#41287=CARTESIAN_POINT('Ctrl Pts',(22.5376023104126,0.584645549343987,3.89414467407578));
#41288=CARTESIAN_POINT('Ctrl Pts',(22.5455549497564,0.602270485672515,3.99148830972497));
#41289=CARTESIAN_POINT('Ctrl Pts',(22.5535075891002,0.595056136077256,4.09332931177355));
#41290=CARTESIAN_POINT('Ctrl Pts',(22.561460228444,0.563884587368514,4.18721625032571));
#41291=CARTESIAN_POINT('Ctrl Pts',(22.5694128677878,0.532713038659782,4.28110318887784));
#41292=CARTESIAN_POINT('Ctrl Pts',(22.5773655071316,0.477584290837583,4.36703606393356));
#41293=CARTESIAN_POINT('Ctrl Pts',(22.5853181464754,0.405238519368296,4.43450837402952));
#41294=CARTESIAN_POINT('Ctrl Pts',(22.5932707858192,0.332892747898984,4.5019806841255));
#41295=CARTESIAN_POINT('Ctrl Pts',(22.601223425163,0.24332995278257,4.55099242926169));
#41296=CARTESIAN_POINT('Ctrl Pts',(22.6091760645068,0.14750052788588,4.57555132613148));
#41297=CARTESIAN_POINT('Ctrl Pts',(22.6131689059187,0.0993867282199646,
4.58788179608141));
#41298=CARTESIAN_POINT('Ctrl Pts',(22.6171617473306,0.0496932250345643,
4.5940481472271));
#41299=CARTESIAN_POINT('Ctrl Pts',(22.6211545887425,-1.51173456864708E-7,
4.59404872180247));
#41300=CARTESIAN_POINT('Origin',(3.42660065607856,0.,4.));
#41301=CARTESIAN_POINT('',(22.7766006560786,-4.98014040841517E-7,4.41590979742004));
#41302=CARTESIAN_POINT('',(22.8,4.87367679877478E-13,4.415875));
#41303=CARTESIAN_POINT('',(3.42660065607856,4.87367679877478E-13,4.415875));
#41304=CARTESIAN_POINT('',(22.8,-0.195748955928421,4.36692555359082));
#41305=CARTESIAN_POINT('Ctrl Pts',(22.7766006560786,-4.98014040834069E-7,
4.41590979742004));
#41306=CARTESIAN_POINT('Ctrl Pts',(22.7844004373857,-0.0679170312443507,
4.41589851620688));
#41307=CARTESIAN_POINT('Ctrl Pts',(22.7922002186928,-0.135834416676695,
4.39892762624317));
#41308=CARTESIAN_POINT('Ctrl Pts',(22.8,-0.195762566582618,4.36695865185838));
#41309=CARTESIAN_POINT('Origin',(22.8,0.,4.));
#41310=CARTESIAN_POINT('Origin',(3.42660065607856,0.,4.));
#41311=CARTESIAN_POINT('',(22.4766006560785,3.63249072247605E-6,4.41584094994071));
#41312=CARTESIAN_POINT('',(22.5733993439214,-1.05822049303872E-7,4.41583910483016));
#41313=CARTESIAN_POINT('',(3.42660065607856,4.87367679877478E-13,4.415875));
#41314=CARTESIAN_POINT('Ctrl Pts',(22.4766006560785,3.63249072248342E-6,
4.41584094994071));
#41315=CARTESIAN_POINT('Ctrl Pts',(22.4810292621689,-0.0385780726118879,
4.41582919621688));
#41316=CARTESIAN_POINT('Ctrl Pts',(22.4934105076031,-0.146451497349971,
4.40094585736882));
#41317=CARTESIAN_POINT('Ctrl Pts',(22.5137443923812,-0.304292138366774,
4.30886736509782));
#41318=CARTESIAN_POINT('Ctrl Pts',(22.5376023104126,-0.415080201412036,
4.12530439950267));
#41319=CARTESIAN_POINT('Ctrl Pts',(22.561460228444,-0.424369795825249,3.91110111771763));
#41320=CARTESIAN_POINT('Ctrl Pts',(22.5853181464754,-0.329889515310188,
3.71863599132299));
#41321=CARTESIAN_POINT('Ctrl Pts',(22.6091760645068,-0.154742073939436,
3.59497211022641));
#41322=CARTESIAN_POINT('Ctrl Pts',(22.6330339825383,0.0582436639512456,
3.57034842802071));
#41323=CARTESIAN_POINT('Ctrl Pts',(22.6568919005697,0.256987911016647,3.65078654733876));
#41324=CARTESIAN_POINT('Ctrl Pts',(22.6807498186011,0.39289034562191,3.81661632308649));
#41325=CARTESIAN_POINT('Ctrl Pts',(22.7046077366325,0.432722782933869,4.02728943245291));
#41326=CARTESIAN_POINT('Ctrl Pts',(22.7284656546639,0.366738191089385,4.2312875884069));
#41327=CARTESIAN_POINT('Ctrl Pts',(22.7523235726953,0.211084664509997,4.37873330099785));
#41328=CARTESIAN_POINT('Ctrl Pts',(22.7683685731669,0.0716802821347026,
4.41560650088387));
#41329=CARTESIAN_POINT('Ctrl Pts',(22.7764609342946,0.00121612829983627,
4.41590999950663));
#41330=CARTESIAN_POINT('Ctrl Pts',(22.7766006560786,-4.98014040834069E-7,
4.41590979742004));
#41331=CARTESIAN_POINT('',(22.8,0.415641328671541,4.01393920819689));
#41332=CARTESIAN_POINT('Origin',(22.8,0.,4.));
#41333=CARTESIAN_POINT('Ctrl Pts',(22.5733993439214,-1.0582204931428E-7,
4.41583910483016));
#41334=CARTESIAN_POINT('Ctrl Pts',(22.5773591418533,-0.034498011376554,
4.41583950370926));
#41335=CARTESIAN_POINT('Ctrl Pts',(22.5892715791291,-0.138279341065089,
4.40307041914735));
#41336=CARTESIAN_POINT('Ctrl Pts',(22.6091366557487,-0.295063722636797,
4.31769517074077));
#41337=CARTESIAN_POINT('Ctrl Pts',(22.6329945737801,-0.411209141905604,
4.13747522778479));
#41338=CARTESIAN_POINT('Ctrl Pts',(22.6568524918115,-0.426804986482714,
3.92363755172126));
#41339=CARTESIAN_POINT('Ctrl Pts',(22.6807104098429,-0.33803111495158,3.72847502015617));
#41340=CARTESIAN_POINT('Ctrl Pts',(22.7045683278743,-0.16660749730952,3.59970312177549));
#41341=CARTESIAN_POINT('Ctrl Pts',(22.7284262459057,0.0455714674079685,
3.56882345794434));
#41342=CARTESIAN_POINT('Ctrl Pts',(22.7522841639372,0.246577802732478,3.64336153500176));
#41343=CARTESIAN_POINT('Ctrl Pts',(22.7761420819686,0.387346815298129,3.80514019809748));
#41344=CARTESIAN_POINT('Ctrl Pts',(22.7920473606562,0.417963038852713,3.94471011778788));
#41345=CARTESIAN_POINT('Ctrl Pts',(22.8,0.415641328671541,4.01393920819689));
#41346=CARTESIAN_POINT('Origin',(3.42660065607856,0.,4.));
#41347=CARTESIAN_POINT('',(22.1766006560786,-8.37799962078257E-6,4.41589611849309));
#41348=CARTESIAN_POINT('',(22.2733993439214,-5.11585294796223E-6,4.41590580604266));
#41349=CARTESIAN_POINT('',(3.42660065607856,4.87367679877478E-13,4.415875));
#41350=CARTESIAN_POINT('Ctrl Pts',(22.1766006560786,-8.37799962077716E-6,
4.41589611849309));
#41351=CARTESIAN_POINT('Ctrl Pts',(22.1776449506995,-0.0091027307950905,
4.41590434335565));
#41352=CARTESIAN_POINT('Ctrl Pts',(22.1866418846642,-0.0874489573854402,
4.4133870032437));
#41353=CARTESIAN_POINT('Ctrl Pts',(22.2035914579727,-0.232253957950086,
4.36612956178204));
#41354=CARTESIAN_POINT('Ctrl Pts',(22.2274493760041,-0.379286482964224,
4.21008217638027));
#41355=CARTESIAN_POINT('Ctrl Pts',(22.2513072940356,-0.433573131350875,
4.00266397632408));
#41356=CARTESIAN_POINT('Ctrl Pts',(22.275165212067,-0.381839338801546,3.79459436150246));
#41357=CARTESIAN_POINT('Ctrl Pts',(22.2990231300984,-0.236735426869051,
3.63675202040985));
#41358=CARTESIAN_POINT('Ctrl Pts',(22.3228810481298,-0.0337432544318164,
3.56773370504276));
#41359=CARTESIAN_POINT('Ctrl Pts',(22.3467389661613,0.177500062688638,3.60441627341574));
#41360=CARTESIAN_POINT('Ctrl Pts',(22.3705968841926,0.345339779804043,3.73782983856348));
#41361=CARTESIAN_POINT('Ctrl Pts',(22.3944548022241,0.428734513273282,3.93535114928888));
#41362=CARTESIAN_POINT('Ctrl Pts',(22.4183127202555,0.407291980919218,4.1486808655136));
#41363=CARTESIAN_POINT('Ctrl Pts',(22.4421706382869,0.286255462618544,4.32565405918856));
#41364=CARTESIAN_POINT('Ctrl Pts',(22.4615999502279,0.130682174689606,4.40492695636159));
#41365=CARTESIAN_POINT('Ctrl Pts',(22.4730766228251,0.0307047625933256,
4.41585030288671));
#41366=CARTESIAN_POINT('Ctrl Pts',(22.4766006560785,3.63249072248342E-6,
4.41584094994071));
#41367=CARTESIAN_POINT('Ctrl Pts',(22.2733993439214,-5.11585294797612E-6,
4.41590580604266));
#41368=CARTESIAN_POINT('Ctrl Pts',(22.2739748303838,-0.0050164638240448,
4.41590888908576));
#41369=CARTESIAN_POINT('Ctrl Pts',(22.2825029561901,-0.0792779396689182,
4.41459464077989));
#41370=CARTESIAN_POINT('Ctrl Pts',(22.2989837213402,-0.221370022215225,
4.37281103827166));
#41371=CARTESIAN_POINT('Ctrl Pts',(22.3228416393716,-0.372934645290675,
4.22116172228637));
#41372=CARTESIAN_POINT('Ctrl Pts',(22.346699557403,-0.43330658847365,4.01543234121164));
#41373=CARTESIAN_POINT('Ctrl Pts',(22.3705574754345,-0.387723268841402,
3.80592933171158));
#41374=CARTESIAN_POINT('Ctrl Pts',(22.3944153934659,-0.247331046528593,
3.64388188817752));
#41375=CARTESIAN_POINT('Ctrl Pts',(22.4182733114973,-0.0464596501027702,
3.56891502119853));
#41376=CARTESIAN_POINT('Ctrl Pts',(22.4421312295287,0.165772403721094,3.59936017830047));
#41377=CARTESIAN_POINT('Ctrl Pts',(22.4659891475602,0.337468575289321,3.7277726770023));
#41378=CARTESIAN_POINT('Ctrl Pts',(22.4898470655915,0.426644514167594,3.92275218663495));
#41379=CARTESIAN_POINT('Ctrl Pts',(22.513704983623,0.411494197867752,4.13662086224655));
#41380=CARTESIAN_POINT('Ctrl Pts',(22.5375629016544,0.295722435535401,4.31708206952049));
#41381=CARTESIAN_POINT('Ctrl Pts',(22.5574610217539,0.138855410360913,4.40292493148274));
#41382=CARTESIAN_POINT('Ctrl Pts',(22.5694065025095,0.0347856757474044,
4.41583870262252));
#41383=CARTESIAN_POINT('Ctrl Pts',(22.5733993439214,-1.0582204931428E-7,
4.41583910483016));
#41384=CARTESIAN_POINT('Origin',(3.42660065607856,0.,4.));
#41385=CARTESIAN_POINT('',(21.8766006560786,1.03078286340212E-5,4.41586151989188));
#41386=CARTESIAN_POINT('',(21.9733993439214,8.40473402259622E-6,4.41585103914036));
#41387=CARTESIAN_POINT('',(3.42660065607856,4.87367679877478E-13,4.415875));
#41388=CARTESIAN_POINT('Ctrl Pts',(21.8766006560786,1.03078286340201E-5,
4.41586151989188));
#41389=CARTESIAN_POINT('Ctrl Pts',(21.8822132785738,-0.0488795353146484,
4.415816298089));
#41390=CARTESIAN_POINT('Ctrl Pts',(21.8957785404128,-0.167079919178725,
4.39498170153279));
#41391=CARTESIAN_POINT('Ctrl Pts',(21.9172964415957,-0.326407159500644,
4.28539643168872));
#41392=CARTESIAN_POINT('Ctrl Pts',(21.9411543596271,-0.423245389017799,
4.09410684177624));
#41393=CARTESIAN_POINT('Ctrl Pts',(21.9650122776585,-0.416588591947193,
3.87980556563057));
#41394=CARTESIAN_POINT('Ctrl Pts',(21.98887019569,-0.30806453650007,3.69489510271888));
#41395=CARTESIAN_POINT('Ctrl Pts',(22.0127281137213,-0.12421031036921,3.58459109808296));
#41396=CARTESIAN_POINT('Ctrl Pts',(22.0365860317528,0.0900167200678817,
3.57586588547707));
#41397=CARTESIAN_POINT('Ctrl Pts',(22.0604439497842,0.282232210442068,3.67085301705332));
#41398=CARTESIAN_POINT('Ctrl Pts',(22.0843018678157,0.405434237512275,3.8463255517439));
#41399=CARTESIAN_POINT('Ctrl Pts',(22.108159785847,0.429496549703537,4.05937567504088));
#41400=CARTESIAN_POINT('Ctrl Pts',(22.1320177038785,0.348535256241736,4.25790682842971));
#41401=CARTESIAN_POINT('Ctrl Pts',(22.1548313272889,0.18962186617866,4.38744320371645));
#41402=CARTESIAN_POINT('Ctrl Pts',(22.1696923113557,0.0601536901409818,
4.41584170838249));
#41403=CARTESIAN_POINT('Ctrl Pts',(22.1766006560786,-8.37799962077716E-6,
4.41589611849309));
#41404=CARTESIAN_POINT('Ctrl Pts',(21.9733993439214,8.40473402260317E-6,
4.41585103914036));
#41405=CARTESIAN_POINT('Ctrl Pts',(21.9785431582582,-0.044801031555974,
4.41581845947763));
#41406=CARTESIAN_POINT('Ctrl Pts',(21.9916396119388,-0.158914563981884,
4.39744691543598));
#41407=CARTESIAN_POINT('Ctrl Pts',(22.0126887049632,-0.317860118355158,
4.29488591379237));
#41408=CARTESIAN_POINT('Ctrl Pts',(22.0365466229946,-0.420290167226249,
4.10653136780738));
#41409=CARTESIAN_POINT('Ctrl Pts',(22.060404541026,-0.419947821735935,3.89212700053744));
#41410=CARTESIAN_POINT('Ctrl Pts',(22.0842624590574,-0.316916794682727,
3.70410052003731));
#41411=CARTESIAN_POINT('Ctrl Pts',(22.1081203770888,-0.136390978688423,
3.58842952252864));
#41412=CARTESIAN_POINT('Ctrl Pts',(22.1319782951203,0.0774861468089536,
3.57339871771534));
#41413=CARTESIAN_POINT('Ctrl Pts',(22.1558362131517,0.27241579873489,3.66268354680831));
#41414=CARTESIAN_POINT('Ctrl Pts',(22.1796941311831,0.400732367405962,3.83445143701846));
#41415=CARTESIAN_POINT('Ctrl Pts',(22.2035520492145,0.431058956528623,4.04670046033727));
#41416=CARTESIAN_POINT('Ctrl Pts',(22.227409967246,0.355979888945518,4.24752994899471));
#41417=CARTESIAN_POINT('Ctrl Pts',(22.2506923988149,0.197764744804664,4.38444734931837));
#41418=CARTESIAN_POINT('Ctrl Pts',(22.26602219104,0.064235283418036,4.41586628455644));
#41419=CARTESIAN_POINT('Ctrl Pts',(22.2733993439214,-5.11585294797612E-6,
4.41590580604266));
#41420=CARTESIAN_POINT('Origin',(3.42660065607856,0.,4.));
#41421=CARTESIAN_POINT('',(21.5766006560785,-1.05752387382048E-5,4.41586434469346));
#41422=CARTESIAN_POINT('',(21.6733993439214,-1.08222664516599E-5,4.41587700699864));
#41423=CARTESIAN_POINT('',(3.42660065607856,4.87367679877478E-13,4.415875));
#41424=CARTESIAN_POINT('Ctrl Pts',(21.5766006560785,-1.05752387381843E-5,
4.41586434469346));
#41425=CARTESIAN_POINT('Ctrl Pts',(21.5788289671043,-0.0194203346498642,
4.41588296395747));
#41426=CARTESIAN_POINT('Ctrl Pts',(21.5890099174739,-0.10809016089515,4.40978779866957));
#41427=CARTESIAN_POINT('Ctrl Pts',(21.6071435071872,-0.258824259222961,
4.34785450957493));
#41428=CARTESIAN_POINT('Ctrl Pts',(21.6310014252187,-0.39385182381868,4.18131050126406));
#41429=CARTESIAN_POINT('Ctrl Pts',(21.6548593432501,-0.432571889182456,
3.97043113659525));
#41430=CARTESIAN_POINT('Ctrl Pts',(21.6787172612815,-0.365516344619441,
3.76678216446856));
#41431=CARTESIAN_POINT('Ctrl Pts',(21.702575179313,-0.209082097331647,3.62016130585559));
#41432=CARTESIAN_POINT('Ctrl Pts',(21.7264330973443,-0.00152158196427748,
3.56642135455923));
#41433=CARTESIAN_POINT('Ctrl Pts',(21.7502910153758,0.206411001640417,3.61870319251831));
#41434=CARTESIAN_POINT('Ctrl Pts',(21.7741489334072,0.363870472821225,3.76422248622317));
#41435=CARTESIAN_POINT('Ctrl Pts',(21.7980068514386,0.432353701764573,3.96739580449697));
#41436=CARTESIAN_POINT('Ctrl Pts',(21.82186476947,0.395114673548107,4.17854173669174));
#41437=CARTESIAN_POINT('Ctrl Pts',(21.8457226875014,0.261259344941517,4.3460293508861));
#41438=CARTESIAN_POINT('Ctrl Pts',(21.8639679830376,0.110037800305057,4.4094070875278));
#41439=CARTESIAN_POINT('Ctrl Pts',(21.87426063923,0.0203934810735595,4.41588037378429));
#41440=CARTESIAN_POINT('Ctrl Pts',(21.8766006560786,1.03078286340201E-5,
4.41586151989188));
#41441=CARTESIAN_POINT('Ctrl Pts',(21.6733993439214,-1.0822266451653E-5,
4.41587700699864));
#41442=CARTESIAN_POINT('Ctrl Pts',(21.6751588467887,-0.0153356749568721,
4.41589290068126));
#41443=CARTESIAN_POINT('Ctrl Pts',(21.6848709889998,-0.0999166717736498,
4.41130778913604));
#41444=CARTESIAN_POINT('Ctrl Pts',(21.7025357705547,-0.248467031045983,
4.35532645760922));
#41445=CARTESIAN_POINT('Ctrl Pts',(21.7263936885861,-0.388341045935521,
4.1928315042612));
#41446=CARTESIAN_POINT('Ctrl Pts',(21.7502516066176,-0.433255096896122,
3.98318399549658));
#41447=CARTESIAN_POINT('Ctrl Pts',(21.774109524649,-0.372226475033738,3.77764845789182));
#41448=CARTESIAN_POINT('Ctrl Pts',(21.7979674426804,-0.220178340780001,
3.62648392906691));
#41449=CARTESIAN_POINT('Ctrl Pts',(21.8218253607118,-0.0142906046679706,
3.56665425395863));
#41450=CARTESIAN_POINT('Ctrl Pts',(21.8456832787432,0.195091573553633,3.61278941785858));
#41451=CARTESIAN_POINT('Ctrl Pts',(21.8695411967747,0.356768547853618,3.75360811649661));
#41452=CARTESIAN_POINT('Ctrl Pts',(21.8933991148061,0.431205894023261,3.95467634223136));
#41453=CARTESIAN_POINT('Ctrl Pts',(21.9172570328375,0.400201653291494,4.16682743688221));
#41454=CARTESIAN_POINT('Ctrl Pts',(21.941114950869,0.271337207055788,4.33818467892719));
#41455=CARTESIAN_POINT('Ctrl Pts',(21.9598290545635,0.118211900824938,4.40773087908456));
#41456=CARTESIAN_POINT('Ctrl Pts',(21.9705905189143,0.0244769910710258,
4.41586882955141));
#41457=CARTESIAN_POINT('Ctrl Pts',(21.9733993439214,8.40473402260317E-6,
4.41585103914036));
#41458=CARTESIAN_POINT('Origin',(3.42660065607856,0.,4.));
#41459=CARTESIAN_POINT('',(21.2766006560785,8.9771325895615E-6,4.41589335210553));
#41460=CARTESIAN_POINT('',(21.3733993439214,1.06214664634743E-5,4.41588075133303));
#41461=CARTESIAN_POINT('',(3.42660065607856,4.87367679877478E-13,4.415875));
#41462=CARTESIAN_POINT('Ctrl Pts',(21.2766006560785,8.97713258955941E-6,
4.41589335210553));
#41463=CARTESIAN_POINT('Ctrl Pts',(21.2833972949786,-0.0591814269577189,
4.41583723296416));
#41464=CARTESIAN_POINT('Ctrl Pts',(21.2981465732225,-0.187680420990878,
4.38813575385326));
#41465=CARTESIAN_POINT('Ctrl Pts',(21.3208484908102,-0.346716519889314,
4.26034671465164));
#41466=CARTESIAN_POINT('Ctrl Pts',(21.3447064088417,-0.429069235164158,
4.0623886883135));
#41467=CARTESIAN_POINT('Ctrl Pts',(21.368564326873,-0.406502834830527,3.8491749282489));
#41468=CARTESIAN_POINT('Ctrl Pts',(21.3924222449045,-0.284535418465691,
3.67284200661995));
#41469=CARTESIAN_POINT('Ctrl Pts',(21.4162801629359,-0.0929913416969399,
3.5765081259772));
#41470=CARTESIAN_POINT('Ctrl Pts',(21.4401380809674,0.121291651150069,3.58372954422009));
#41471=CARTESIAN_POINT('Ctrl Pts',(21.4639959989987,0.305915531372611,3.69274042788069));
#41472=CARTESIAN_POINT('Ctrl Pts',(21.4878539170302,0.415734731202803,3.87688464650718));
#41473=CARTESIAN_POINT('Ctrl Pts',(21.5117118350615,0.423895464867194,4.09113392265755));
#41474=CARTESIAN_POINT('Ctrl Pts',(21.535569753093,0.328402210690932,4.28309847227994));
#41475=CARTESIAN_POINT('Ctrl Pts',(21.5571993600986,0.169024930905334,4.39437398220882));
#41476=CARTESIAN_POINT('Ctrl Pts',(21.5708763277605,0.0498513310028489,
4.41581651349798));
#41477=CARTESIAN_POINT('Ctrl Pts',(21.5766006560785,-1.05752387381843E-5,
4.41586434469346));
#41478=CARTESIAN_POINT('Ctrl Pts',(21.3733993439214,1.06214664634605E-5,
4.41588075133303));
#41479=CARTESIAN_POINT('Ctrl Pts',(21.379727174663,-0.0551018547626871,
4.41582358345633));
#41480=CARTESIAN_POINT('Ctrl Pts',(21.3940076447484,-0.1795281855266,4.39095386216025));
#41481=CARTESIAN_POINT('Ctrl Pts',(21.4162407541777,-0.338898428465248,
4.27044521104599));
#41482=CARTESIAN_POINT('Ctrl Pts',(21.4400986722091,-0.427045644525908,
4.07499849655415));
#41483=CARTESIAN_POINT('Ctrl Pts',(21.4639565902406,-0.410768568010174,
3.86121260673678));
#41484=CARTESIAN_POINT('Ctrl Pts',(21.4878145082719,-0.294047387504818,
3.68136401506497));
#41485=CARTESIAN_POINT('Ctrl Pts',(21.5116724263034,-0.105423611064507,
3.57943060117972));
#41486=CARTESIAN_POINT('Ctrl Pts',(21.5355303443348,0.108979109962582,3.58033786138646));
#41487=CARTESIAN_POINT('Ctrl Pts',(21.5593882623662,0.296733470072461,3.68386394585134));
#41488=CARTESIAN_POINT('Ctrl Pts',(21.5832461803976,0.411928413892185,3.86469390692879));
#41489=CARTESIAN_POINT('Ctrl Pts',(21.6071040984291,0.426395639810567,4.07860989342611));
#41490=CARTESIAN_POINT('Ctrl Pts',(21.6309620164605,0.33659751701124,4.27330361969026));
#41491=CARTESIAN_POINT('Ctrl Pts',(21.6530604316246,0.177184770587036,4.39173732935402));
#41492=CARTESIAN_POINT('Ctrl Pts',(21.6672062074449,0.0539299276789421,
4.41582106406873));
#41493=CARTESIAN_POINT('Ctrl Pts',(21.6733993439214,-1.0822266451653E-5,
4.41587700699864));
#41494=CARTESIAN_POINT('Origin',(3.42660065607856,0.,4.));
#41495=CARTESIAN_POINT('',(20.9766006560786,-4.48287659654576E-6,4.41584197426197));
#41496=CARTESIAN_POINT('',(21.0733993439214,-7.65157297119567E-6,4.41584853425778));
#41497=CARTESIAN_POINT('',(3.42660065607856,4.87367679877478E-13,4.415875));
#41498=CARTESIAN_POINT('Ctrl Pts',(20.9766006560786,-4.48287659652116E-6,
4.41584197426197));
#41499=CARTESIAN_POINT('Ctrl Pts',(20.9800129835092,-0.0297322302090305,
4.41585318364051));
#41500=CARTESIAN_POINT('Ctrl Pts',(20.9913779502836,-0.128734546054536,
4.40538471300776));
#41501=CARTESIAN_POINT('Ctrl Pts',(21.0106955564018,-0.28396276796243,4.32765515869354));
#41502=CARTESIAN_POINT('Ctrl Pts',(21.0345534744332,-0.40623841344949,4.15153583326342));
#41503=CARTESIAN_POINT('Ctrl Pts',(21.0584113924646,-0.429177699343215,
3.93836186909709));
#41504=CARTESIAN_POINT('Ctrl Pts',(21.082269310496,-0.347171348131155,3.74026010679315));
#41505=CARTESIAN_POINT('Ctrl Pts',(21.1061272285274,-0.180272145040548,
3.605671823621));
#41506=CARTESIAN_POINT('Ctrl Pts',(21.1299851465589,0.0307085077608185,
3.56750752082027));
#41507=CARTESIAN_POINT('Ctrl Pts',(21.1538430645903,0.234180094072738,3.63509941005724));
#41508=CARTESIAN_POINT('Ctrl Pts',(21.1777009826217,0.380388268371489,3.79191943321731));
#41509=CARTESIAN_POINT('Ctrl Pts',(21.2015589006531,0.433581149524578,3.99962082296209));
#41510=CARTESIAN_POINT('Ctrl Pts',(21.2254168186846,0.380751629084578,4.2074149318183));
#41511=CARTESIAN_POINT('Ctrl Pts',(21.2492747367159,0.234817963878357,4.36449043997717));
#41512=CARTESIAN_POINT('Ctrl Pts',(21.2663360158473,0.0893960873046664,
4.41308118928586));
#41513=CARTESIAN_POINT('Ctrl Pts',(21.2754446556348,0.0100763257733538,
4.41590289708112));
#41514=CARTESIAN_POINT('Ctrl Pts',(21.2766006560785,8.97713258955941E-6,
4.41589335210553));
#41515=CARTESIAN_POINT('Ctrl Pts',(21.0733993439214,-7.65157297121996E-6,
4.41584853425778));
#41516=CARTESIAN_POINT('Ctrl Pts',(21.0763428631935,-0.0256500457845501,
4.41586537097631));
#41517=CARTESIAN_POINT('Ctrl Pts',(21.0872390218095,-0.120560449820324,
4.40722571769055));
#41518=CARTESIAN_POINT('Ctrl Pts',(21.1060878197692,-0.274189543318984,
4.33587624407661));
#41519=CARTESIAN_POINT('Ctrl Pts',(21.1299457378007,-0.401599180171465,
4.16343456021562));
#41520=CARTESIAN_POINT('Ctrl Pts',(21.1538036558321,-0.430806878168669,
3.95102867450389));
#41521=CARTESIAN_POINT('Ctrl Pts',(21.1776615738635,-0.354670559489406,
3.75059761183336));
#41522=CARTESIAN_POINT('Ctrl Pts',(21.2015194918949,-0.191807627993766,
3.61115222665144));
#41523=CARTESIAN_POINT('Ctrl Pts',(21.2253774099264,0.0179574932869785,
3.56679071405539));
#41524=CARTESIAN_POINT('Ctrl Pts',(21.2492353279577,0.223331518303719,3.62836067225603));
#41525=CARTESIAN_POINT('Ctrl Pts',(21.2730932459892,0.374094903668402,3.78080656934254));
#41526=CARTESIAN_POINT('Ctrl Pts',(21.2969511640206,0.433381894944723,3.98685123093373));
#41527=CARTESIAN_POINT('Ctrl Pts',(21.320809082052,0.386695207821707,4.19611112472705));
#41528=CARTESIAN_POINT('Ctrl Pts',(21.3446670000834,0.245451009020076,4.35741650656472));
#41529=CARTESIAN_POINT('Ctrl Pts',(21.3621970873732,0.0975684711839555,
4.41172139589413));
#41530=CARTESIAN_POINT('Ctrl Pts',(21.3717745353192,0.014161952170494,4.41589543043265));
#41531=CARTESIAN_POINT('Ctrl Pts',(21.3733993439214,1.06214664634605E-5,
4.41588075133303));
#41532=CARTESIAN_POINT('Origin',(3.42660065607856,0.,4.));
#41533=CARTESIAN_POINT('',(20.6766006560786,1.29204965968245E-6,4.41591114679826));
#41534=CARTESIAN_POINT('',(20.7733993439214,3.9567662055099E-6,4.41590779860895));
#41535=CARTESIAN_POINT('',(3.42660065607856,4.87367679877478E-13,4.415875));
#41536=CARTESIAN_POINT('Ctrl Pts',(20.6766006560786,1.29076178055295E-6,
4.41591111076812));
#41537=CARTESIAN_POINT('Ctrl Pts',(20.6766286720397,-0.000242659277546582,
4.41591112051333));
#41538=CARTESIAN_POINT('Ctrl Pts',(20.6846093273446,-0.0697345275278937,
4.41585145172406));
#41539=CARTESIAN_POINT('Ctrl Pts',(20.7005426219933,-0.208420567790133,
4.38020336888205));
#41540=CARTESIAN_POINT('Ctrl Pts',(20.7244005400248,-0.365106210756856,
4.23385701605743));
#41541=CARTESIAN_POINT('Ctrl Pts',(20.7482584580562,-0.432520392530856,
4.03032528343114));
#41542=CARTESIAN_POINT('Ctrl Pts',(20.7721163760876,-0.394167874571092,
3.81937870627435));
#41543=CARTESIAN_POINT('Ctrl Pts',(20.795974294119,-0.259432524437891,3.65259868360638));
#41544=CARTESIAN_POINT('Ctrl Pts',(20.8198322121504,-0.0612578225112809,
3.57076788979259));
#41545=CARTESIAN_POINT('Ctrl Pts',(20.8436901301819,0.151895538690754,3.5938959627232));
#41546=CARTESIAN_POINT('Ctrl Pts',(20.8675480482132,0.327906592802717,3.71632757520176));
#41547=CARTESIAN_POINT('Ctrl Pts',(20.8914059662447,0.423735399567132,3.90812480123879));
#41548=CARTESIAN_POINT('Ctrl Pts',(20.9152638842761,0.415949440063929,4.12238802732943));
#41549=CARTESIAN_POINT('Ctrl Pts',(20.9391218023075,0.30645246920106,4.30672404095661));
#41550=CARTESIAN_POINT('Ctrl Pts',(20.9595673929083,0.148398440326279,4.40042000858165));
#41551=CARTESIAN_POINT('Ctrl Pts',(20.9720603441653,0.0395501167658222,
4.4158270594931));
#41552=CARTESIAN_POINT('Ctrl Pts',(20.9766006560786,-4.48287659652116E-6,
4.41584197426197));
#41553=CARTESIAN_POINT('Ctrl Pts',(20.7733993439214,3.95676620551077E-6,
4.41590779860895));
#41554=CARTESIAN_POINT('Ctrl Pts',(20.7809111910678,-0.0654084660523611,
4.41587519962517));
#41555=CARTESIAN_POINT('Ctrl Pts',(20.7963756775582,-0.200102595337945,
4.3835597345012));
#41556=CARTESIAN_POINT('Ctrl Pts',(20.8197928033922,-0.358062019934396,
4.24450842127602));
#41557=CARTESIAN_POINT('Ctrl Pts',(20.8436507214237,-0.431438726014498,
4.04305074550709));
#41558=CARTESIAN_POINT('Ctrl Pts',(20.867508639455,-0.399316990859146,3.83106596928302));
#41559=CARTESIAN_POINT('Ctrl Pts',(20.8913665574865,-0.269551332195825,
3.66039017609669));
#41560=CARTESIAN_POINT('Ctrl Pts',(20.9152244755179,-0.0738730526583281,
3.57275822989076));
#41561=CARTESIAN_POINT('Ctrl Pts',(20.9390823935493,0.139869212314499,3.58959853735383));
#41562=CARTESIAN_POINT('Ctrl Pts',(20.9629403115807,0.319409638666883,3.70679317993256));
#41563=CARTESIAN_POINT('Ctrl Pts',(20.9867982296122,0.420845711130686,3.8956848776653));
#41564=CARTESIAN_POINT('Ctrl Pts',(21.0106561476436,0.419373541863394,4.11008446384341));
#41565=CARTESIAN_POINT('Ctrl Pts',(21.034514065675,0.315353119032788,4.29756540021079));
#41566=CARTESIAN_POINT('Ctrl Pts',(21.0554284644342,0.156567902793621,4.39812991232556));
#41567=CARTESIAN_POINT('Ctrl Pts',(21.0683902238497,0.0436291721249729,
4.41581988245125));
#41568=CARTESIAN_POINT('Ctrl Pts',(21.0733993439214,-7.65157297121996E-6,
4.41584853425778));
#41569=CARTESIAN_POINT('Origin',(3.42660065607856,0.,4.));
#41570=CARTESIAN_POINT('',(20.3766006560786,0.000383027521040961,4.41597069455794));
#41571=CARTESIAN_POINT('',(20.4733993439214,0.000101608071013781,4.41586489633469));
#41572=CARTESIAN_POINT('',(3.42660065607856,4.87367679877478E-13,4.415875));
#41573=CARTESIAN_POINT('Ctrl Pts',(20.3766006560786,0.000383027521040954,
4.41597069455794));
#41574=CARTESIAN_POINT('Ctrl Pts',(20.3891496392578,-0.108893832387875,
4.41487837761012));
#41575=CARTESIAN_POINT('Ctrl Pts',(20.4176039011246,-0.35839559572325,4.31454223548297));
#41576=CARTESIAN_POINT('Ctrl Pts',(20.4540108023354,-0.457800032585507,
3.97025345815189));
#41577=CARTESIAN_POINT('Ctrl Pts',(20.4858213597105,-0.325993724402262,
3.71529210935379));
#41578=CARTESIAN_POINT('Ctrl Pts',(20.509679277742,-0.15096738523986,3.59329490328468));
#41579=CARTESIAN_POINT('Ctrl Pts',(20.5335371957734,0.0630371972956549,
3.57102347342756));
#41580=CARTESIAN_POINT('Ctrl Pts',(20.5573951138048,0.260511246441404,3.65349437971329));
#41581=CARTESIAN_POINT('Ctrl Pts',(20.5812530318362,0.394877283734959,3.82077798440408));
#41582=CARTESIAN_POINT('Ctrl Pts',(20.6051109498677,0.432370081305563,4.03184236506754));
#41583=CARTESIAN_POINT('Ctrl Pts',(20.6289688678991,0.364303478986858,4.23514367899931));
#41584=CARTESIAN_POINT('Ctrl Pts',(20.6527987699694,0.207251017164088,4.38076243960928));
#41585=CARTESIAN_POINT('Ctrl Pts',(20.6686760326959,0.0690052481014253,
4.41590835422812));
#41586=CARTESIAN_POINT('Ctrl Pts',(20.6766006560786,1.29076178055295E-6,
4.41591111076812));
#41587=CARTESIAN_POINT('Ctrl Pts',(20.4733993439214,0.000101608071013788,
4.4158648963347));
#41588=CARTESIAN_POINT('Ctrl Pts',(20.4775268795984,-0.0359150725839473,
4.41584626969953));
#41589=CARTESIAN_POINT('Ctrl Pts',(20.4896070546192,-0.141401612166324,
4.40227446254147));
#41590=CARTESIAN_POINT('Ctrl Pts',(20.5096398689838,-0.298255971346869,
4.31460392554555));
#41591=CARTESIAN_POINT('Ctrl Pts',(20.5334977870152,-0.412709509332759,
4.13311446574462));
#41592=CARTESIAN_POINT('Ctrl Pts',(20.5573557050466,-0.425936384696969,
3.91915434697803));
#41593=CARTESIAN_POINT('Ctrl Pts',(20.581213623078,-0.335173342752607,3.72492109335083));
#41594=CARTESIAN_POINT('Ctrl Pts',(20.6050715411095,-0.162364888615448,
3.59797442377207));
#41595=CARTESIAN_POINT('Ctrl Pts',(20.6289294591408,0.0501004451364318,
3.56932214892951));
#41596=CARTESIAN_POINT('Ctrl Pts',(20.6527873771723,0.250339089241223,3.64598859455508));
#41597=CARTESIAN_POINT('Ctrl Pts',(20.6766452952037,0.389350172549011,3.80921715950176));
#41598=CARTESIAN_POINT('Ctrl Pts',(20.7005032132352,0.433161330121289,4.01909908002448));
#41599=CARTESIAN_POINT('Ctrl Pts',(20.7243611312665,0.371049143609512,4.22430982617278));
#41600=CARTESIAN_POINT('Ctrl Pts',(20.748219049298,0.218207240773441,4.37467120177868));
#41601=CARTESIAN_POINT('Ctrl Pts',(20.7645651201829,0.0769305199015265,
4.41491906931248));
#41602=CARTESIAN_POINT('Ctrl Pts',(20.772958551724,0.00384233167249433,
4.41590971150433));
#41603=CARTESIAN_POINT('Ctrl Pts',(20.7733993439214,3.95676620551077E-6,
4.41590779860895));
#41604=CARTESIAN_POINT('Origin',(3.42660065607856,0.,4.));
#41605=CARTESIAN_POINT('',(20.0766006560786,-0.000186622634748148,4.41645953600834));
#41606=CARTESIAN_POINT('',(20.1733993439214,-0.000111611226006447,4.41653056081536));
#41607=CARTESIAN_POINT('',(3.42660065607856,4.87367679877478E-13,4.415875));
#41608=CARTESIAN_POINT('Ctrl Pts',(20.0766006560786,-0.000186622634748109,
4.41645953600834));
#41609=CARTESIAN_POINT('Ctrl Pts',(20.0778126884445,-0.0107019642254321,
4.4165186149328));
#41610=CARTESIAN_POINT('Ctrl Pts',(20.0949299994981,-0.159149739060163,
4.41138240526969));
#41611=CARTESIAN_POINT('Ctrl Pts',(20.1279525892393,-0.432744382500041,
4.23375285658289));
#41612=CARTESIAN_POINT('Ctrl Pts',(20.1756684253021,-0.430649333670284,
3.76246031529274));
#41613=CARTESIAN_POINT('Ctrl Pts',(20.223384261365,-0.033136228617316,3.50924504180455));
#41614=CARTESIAN_POINT('Ctrl Pts',(20.2711000974278,0.394908089060633,3.70680919012016));
#41615=CARTESIAN_POINT('Ctrl Pts',(20.3188159334906,0.460110046434968,4.17340395051402));
#41616=CARTESIAN_POINT('Ctrl Pts',(20.3539827863742,0.197028357007358,4.40022211154544));
#41617=CARTESIAN_POINT('Ctrl Pts',(20.3732443605702,0.0296097328916507,
4.416262840815));
#41618=CARTESIAN_POINT('Ctrl Pts',(20.3766006560786,0.000383027521040954,
4.41597069455794));
#41619=CARTESIAN_POINT('Ctrl Pts',(20.1733993439214,-0.000111611226006447,
4.41653056081536));
#41620=CARTESIAN_POINT('Ctrl Pts',(20.1741425681289,-0.00655727229825777,
4.41655465488103));
#41621=CARTESIAN_POINT('Ctrl Pts',(20.190791071024,-0.150919726673813,4.41348743992374));
#41622=CARTESIAN_POINT('Ctrl Pts',(20.2233448526067,-0.425711472830213,
4.24633918020534));
#41623=CARTESIAN_POINT('Ctrl Pts',(20.2710606886696,-0.437384262562023,
3.77535541015343));
#41624=CARTESIAN_POINT('Ctrl Pts',(20.3187765247324,-0.0477164433392854,
3.51022640082505));
#41625=CARTESIAN_POINT('Ctrl Pts',(20.3664923607953,0.386374384143037,3.69571627142296));
#41626=CARTESIAN_POINT('Ctrl Pts',(20.4062555575143,0.45143962727185,4.08165775845481));
#41627=CARTESIAN_POINT('Ctrl Pts',(20.4380661148895,0.291471375703242,4.31996082336987));
#41628=CARTESIAN_POINT('Ctrl Pts',(20.4577964972439,0.136183087716603,4.40372206768731));
#41629=CARTESIAN_POINT('Ctrl Pts',(20.4695742402546,0.0334792813416625,
4.41588215816259));
#41630=CARTESIAN_POINT('Ctrl Pts',(20.4733993439214,0.000101608071013788,
4.4158648963347));
#41631=CARTESIAN_POINT('Origin',(3.42660065607856,0.,4.));
#41632=CARTESIAN_POINT('',(19.7766006560786,-0.000280998963924209,4.41539029291088));
#41633=CARTESIAN_POINT('',(19.8733993439214,-0.000322938566065189,4.41548189938477));
#41634=CARTESIAN_POINT('',(3.42660065607856,4.87367679877478E-13,4.415875));
#41635=CARTESIAN_POINT('Ctrl Pts',(19.7766006560786,-0.000280998963924181,
4.41539029291088));
#41636=CARTESIAN_POINT('Ctrl Pts',(19.7823810163188,-0.0507615353771658,
4.41570272077311));
#41637=CARTESIAN_POINT('Ctrl Pts',(19.8040666552467,-0.23976299482565,4.3837755623668));
#41638=CARTESIAN_POINT('Ctrl Pts',(19.8416575728622,-0.481212499922896,
4.10168523844358));
#41639=CARTESIAN_POINT('Ctrl Pts',(19.8893734089251,-0.345789702982467,
3.65023692191923));
#41640=CARTESIAN_POINT('Ctrl Pts',(19.9370892449879,0.107175910646637,3.51998011832295));
#41641=CARTESIAN_POINT('Ctrl Pts',(19.9848050810508,0.461722480014006,3.83053541934297));
#41642=CARTESIAN_POINT('Ctrl Pts',(20.0313088847476,0.394022427012164,4.28486673161383));
#41643=CARTESIAN_POINT('Ctrl Pts',(20.0619074097569,0.127288937001902,4.4157433330307));
#41644=CARTESIAN_POINT('Ctrl Pts',(20.0766006560786,-0.000186622634748109,
4.41645953600834));
#41645=CARTESIAN_POINT('Ctrl Pts',(19.8733993439214,-0.000322938566065196,
4.41548189938477));
#41646=CARTESIAN_POINT('Ctrl Pts',(19.8787108960032,-0.0466836533228258,
4.41581668875846));
#41647=CARTESIAN_POINT('Ctrl Pts',(19.8999277267727,-0.231469429366377,
4.38724295332581));
#41648=CARTESIAN_POINT('Ctrl Pts',(19.9370498362297,-0.47800980043334,4.11581244897344));
#41649=CARTESIAN_POINT('Ctrl Pts',(19.9847656722926,-0.355939225796451,
3.66057517601247));
#41650=CARTESIAN_POINT('Ctrl Pts',(20.0324815083554,0.0929888682922082,
3.51702731322357));
#41651=CARTESIAN_POINT('Ctrl Pts',(20.0801973444182,0.456536973876988,3.81701888067549));
#41652=CARTESIAN_POINT('Ctrl Pts',(20.1271699562736,0.401683300383188,4.27772103607547));
#41653=CARTESIAN_POINT('Ctrl Pts',(20.1582372894413,0.131382308576697,4.41603903277767));
#41654=CARTESIAN_POINT('Ctrl Pts',(20.1733993439214,-0.000111611226006447,
4.41653056081536));
#41655=CARTESIAN_POINT('Origin',(3.42660065607856,0.,4.));
#41656=CARTESIAN_POINT('',(19.4766006560786,0.000302289446139524,4.41543216566181));
#41657=CARTESIAN_POINT('',(19.5733993439214,0.000255464646300079,4.41534829948978));
#41658=CARTESIAN_POINT('',(3.42660065607856,4.87367679877478E-13,4.415875));
#41659=CARTESIAN_POINT('Ctrl Pts',(19.4766006560786,0.000302289446139546,
4.41543216566181));
#41660=CARTESIAN_POINT('Ctrl Pts',(19.4869493441932,-0.0900510892866153,
4.41482666801407));
#41661=CARTESIAN_POINT('Ctrl Pts',(19.5132033109954,-0.320168095705801,
4.3413809155508));
#41662=CARTESIAN_POINT('Ctrl Pts',(19.5553625564852,-0.490312813065352,
3.96128857502183));
#41663=CARTESIAN_POINT('Ctrl Pts',(19.603078392548,-0.232620797759261,3.56664935826393));
#41664=CARTESIAN_POINT('Ctrl Pts',(19.6507942286109,0.238690449241969,3.56996267500769));
#41665=CARTESIAN_POINT('Ctrl Pts',(19.6985100646737,0.490808633485035,3.96818593857384));
#41666=CARTESIAN_POINT('Ctrl Pts',(19.7404455404963,0.316268156276861,4.34384396940031));
#41667=CARTESIAN_POINT('Ctrl Pts',(19.7664757376312,0.0881410531427697,
4.41484304213512));
#41668=CARTESIAN_POINT('Ctrl Pts',(19.7766006560786,-0.000280998963924181,
4.41539029291088));
#41669=CARTESIAN_POINT('Ctrl Pts',(19.5733993439214,0.000255464646300094,
4.41534829948978));
#41670=CARTESIAN_POINT('Ctrl Pts',(19.5832792238775,-0.0860485087386658,
4.41486588036018));
#41671=CARTESIAN_POINT('Ctrl Pts',(19.6090643825213,-0.311990568344336,
4.34649332259355));
#41672=CARTESIAN_POINT('Ctrl Pts',(19.6507548198527,-0.491240257057309,
3.97574594767572));
#41673=CARTESIAN_POINT('Ctrl Pts',(19.6984706559155,-0.245282818621706,
3.57368850533185));
#41674=CARTESIAN_POINT('Ctrl Pts',(19.7461864919783,0.225921452997342,3.56311925573479));
#41675=CARTESIAN_POINT('Ctrl Pts',(19.7939023280412,0.489658867576397,3.95374471702426));
#41676=CARTESIAN_POINT('Ctrl Pts',(19.8363066120222,0.324430886710512,4.33863507066385));
#41677=CARTESIAN_POINT('Ctrl Pts',(19.8628056173156,0.0921420753912029,
4.4148141723173));
#41678=CARTESIAN_POINT('Ctrl Pts',(19.8733993439214,-0.000322938566065196,
4.41548189938477));
#41679=CARTESIAN_POINT('Origin',(3.42660065607856,0.,4.));
#41680=CARTESIAN_POINT('',(19.1766006560786,0.000155842099650094,4.41649089206047));
#41681=CARTESIAN_POINT('',(19.2733993439214,0.000220989830587742,4.4164164649367));
#41682=CARTESIAN_POINT('',(3.42660065607856,4.87367679877478E-13,4.415875));
#41683=CARTESIAN_POINT('Ctrl Pts',(19.1766006560786,0.000155842099650088,
4.41649089206047));
#41684=CARTESIAN_POINT('Ctrl Pts',(19.1915176720675,-0.129233580897558,
4.41587069825202));
#41685=CARTESIAN_POINT('Ctrl Pts',(19.2223399667441,-0.397695790553126,
4.28149179527637));
#41686=CARTESIAN_POINT('Ctrl Pts',(19.2690675401082,-0.459293044881286,
3.82405931712685));
#41687=CARTESIAN_POINT('Ctrl Pts',(19.316783376171,-0.100417177000157,3.51852142809106));
#41688=CARTESIAN_POINT('Ctrl Pts',(19.3644992122339,0.350673329058588,3.65513271950473));
#41689=CARTESIAN_POINT('Ctrl Pts',(19.4122150482967,0.479735122332443,4.10844094226069));
#41690=CARTESIAN_POINT('Ctrl Pts',(19.4495821962449,0.235804435834584,4.38544967282755));
#41691=CARTESIAN_POINT('Ctrl Pts',(19.4710440655056,0.0488163355692654,
4.4157572795781));
#41692=CARTESIAN_POINT('Ctrl Pts',(19.4766006560786,0.000302289446139546,
4.41543216566181));
#41693=CARTESIAN_POINT('Ctrl Pts',(19.2733993439214,0.000220989830587761,
4.4164164649367));
#41694=CARTESIAN_POINT('Ctrl Pts',(19.2878475517519,-0.125161313229646,
4.41561068768233));
#41695=CARTESIAN_POINT('Ctrl Pts',(19.31820103827,-0.389985711500173,4.28851341748863));
#41696=CARTESIAN_POINT('Ctrl Pts',(19.3644598034757,-0.464275578741542,
3.8376626582024));
#41697=CARTESIAN_POINT('Ctrl Pts',(19.4121756395385,-0.114554038379521,
3.52168776344319));
#41698=CARTESIAN_POINT('Ctrl Pts',(19.4598914756013,0.340364234683876,3.64495435060606));
#41699=CARTESIAN_POINT('Ctrl Pts',(19.5076073116642,0.482720800247919,4.09426482953845));
#41700=CARTESIAN_POINT('Ctrl Pts',(19.5454432677708,0.244097666198316,4.38190156491584));
#41701=CARTESIAN_POINT('Ctrl Pts',(19.5673739451899,0.0528892875329133,
4.41564251031262));
#41702=CARTESIAN_POINT('Ctrl Pts',(19.5733993439214,0.000255464646300094,
4.41534829948978));
#41703=CARTESIAN_POINT('Origin',(3.42660065607856,0.,4.));
#41704=CARTESIAN_POINT('',(18.8766006560785,-0.00038196507782994,4.41590683121974));
#41705=CARTESIAN_POINT('',(18.9733993439214,-0.000368287616214491,4.41603142687637));
#41706=CARTESIAN_POINT('',(3.42660065607856,4.87367679877478E-13,4.415875));
#41707=CARTESIAN_POINT('Ctrl Pts',(18.8766006560785,-0.000381965077829925,
4.41590683121974));
#41708=CARTESIAN_POINT('Ctrl Pts',(18.8801807212542,-0.0315488007868432,
4.41619587167324));
#41709=CARTESIAN_POINT('Ctrl Pts',(18.8996660651174,-0.200861076696893,
4.39874895857547));
#41710=CARTESIAN_POINT('Ctrl Pts',(18.9350566876684,-0.462607878309702,
4.16703046362027));
#41711=CARTESIAN_POINT('Ctrl Pts',(18.9827725237311,-0.39069124519864,3.70122654773242));
#41712=CARTESIAN_POINT('Ctrl Pts',(19.030488359794,0.0400031699426168,3.50979089028978));
#41713=CARTESIAN_POINT('Ctrl Pts',(19.0782041958568,0.433962058584907,3.76852180111673));
#41714=CARTESIAN_POINT('Ctrl Pts',(19.1259200319197,0.429406911488226,4.23982270375453));
#41715=CARTESIAN_POINT('Ctrl Pts',(19.1587188519936,0.155221332864305,4.41240136130926));
#41716=CARTESIAN_POINT('Ctrl Pts',(19.1756123933799,0.00872798149047904,
4.41653198033223));
#41717=CARTESIAN_POINT('Ctrl Pts',(19.1766006560786,0.000155842099650088,
4.41649089206047));
#41718=CARTESIAN_POINT('Ctrl Pts',(18.9733993439214,-0.000368287616214533,
4.41603142687637));
#41719=CARTESIAN_POINT('Ctrl Pts',(18.9765106009386,-0.0274330213022572,
4.4162811262788));
#41720=CARTESIAN_POINT('Ctrl Pts',(18.9955271366434,-0.192586232161443,
4.40152565608163));
#41721=CARTESIAN_POINT('Ctrl Pts',(19.0304489510358,-0.457487847288108,
4.18058265263639));
#41722=CARTESIAN_POINT('Ctrl Pts',(19.0781647870987,-0.399321187381313,
3.71286272589862));
#41723=CARTESIAN_POINT('Ctrl Pts',(19.1258806231614,0.0255482632835279,
3.50882537619781));
#41724=CARTESIAN_POINT('Ctrl Pts',(19.1735964592243,0.426956350589889,3.75584124112414));
#41725=CARTESIAN_POINT('Ctrl Pts',(19.2213122952871,0.436283851722622,4.22707185138688));
#41726=CARTESIAN_POINT('Ctrl Pts',(19.2545799235195,0.163455264474221,4.41023200720537));
#41727=CARTESIAN_POINT('Ctrl Pts',(19.2719422730642,0.0128655269200745,
4.41649772584937));
#41728=CARTESIAN_POINT('Ctrl Pts',(19.2733993439214,0.000220989830587761,
4.4164164649367));
#41729=CARTESIAN_POINT('Origin',(3.42660065607856,0.,4.));
#41730=CARTESIAN_POINT('',(18.5766006560786,2.82854505807383E-5,4.41518799822097));
#41731=CARTESIAN_POINT('',(18.6733993439214,-3.94222854199766E-5,4.41518963037823));
#41732=CARTESIAN_POINT('',(3.42660065607856,4.87367679877478E-13,4.415875));
#41733=CARTESIAN_POINT('Ctrl Pts',(18.5766006560786,2.82854505807215E-5,
4.41518799822097));
#41734=CARTESIAN_POINT('Ctrl Pts',(18.5847490491285,-0.0712192880865648,
4.41514491699706));
#41735=CARTESIAN_POINT('Ctrl Pts',(18.6088027208661,-0.281596950705947,
4.36382162423513));
#41736=CARTESIAN_POINT('Ctrl Pts',(18.6487616712913,-0.49096944006335,4.0292272779409));
#41737=CARTESIAN_POINT('Ctrl Pts',(18.6964775073541,-0.290120809601049,
3.60284116440841));
#41738=CARTESIAN_POINT('Ctrl Pts',(18.744193343417,0.177150224400508,3.54117212067402));
#41739=CARTESIAN_POINT('Ctrl Pts',(18.7919091794797,0.481741481528227,3.90085177849878));
#41740=CARTESIAN_POINT('Ctrl Pts',(18.836044950367,0.354281053487698,4.31776308733785));
#41741=CARTESIAN_POINT('Ctrl Pts',(18.8642754425666,0.106917172161326,4.4149117417093));
#41742=CARTESIAN_POINT('Ctrl Pts',(18.8766006560785,-0.000381965077829925,
4.41590683121974));
#41743=CARTESIAN_POINT('Ctrl Pts',(18.6733993439214,-3.94222854199489E-5,
4.41518963037823));
#41744=CARTESIAN_POINT('Ctrl Pts',(18.6810789288129,-0.0671871929144198,
4.41524623173262));
#41745=CARTESIAN_POINT('Ctrl Pts',(18.704663792392,-0.273330541024821,4.36810584919535));
#41746=CARTESIAN_POINT('Ctrl Pts',(18.7441539346588,-0.489895661254576,
4.0436745456279));
#41747=CARTESIAN_POINT('Ctrl Pts',(18.7918697707216,-0.301692008317894,
3.6115580391236));
#41748=CARTESIAN_POINT('Ctrl Pts',(18.8395856067845,0.163560057986223,3.53615376224111));
#41749=CARTESIAN_POINT('Ctrl Pts',(18.8873014428472,0.478612406344963,3.88670662268212));
#41750=CARTESIAN_POINT('Ctrl Pts',(18.9319060218929,0.362263203066427,4.31165738429376));
#41751=CARTESIAN_POINT('Ctrl Pts',(18.960605322251,0.110926532249199,4.41500462017153));
#41752=CARTESIAN_POINT('Ctrl Pts',(18.9733993439214,-0.000368287616214533,
4.41603142687637));
#41753=CARTESIAN_POINT('Origin',(3.42660065607856,0.,4.));
#41754=CARTESIAN_POINT('',(18.2766006560786,0.000371443240938316,4.41601098728712));
#41755=CARTESIAN_POINT('',(18.3733993439214,0.000382963303967143,4.41588626824893));
#41756=CARTESIAN_POINT('',(3.42660065607856,4.87367679877478E-13,4.415875));
#41757=CARTESIAN_POINT('Ctrl Pts',(18.2766006560785,0.000371443240938293,
4.41601098728712));
#41758=CARTESIAN_POINT('Ctrl Pts',(18.2893173770028,-0.110264925490287,
4.41498710445335));
#41759=CARTESIAN_POINT('Ctrl Pts',(18.3179393766147,-0.360950442388199,
4.31267773405576));
#41760=CARTESIAN_POINT('Ctrl Pts',(18.3624666549143,-0.479157019140895,
3.88903254594255));
#41761=CARTESIAN_POINT('Ctrl Pts',(18.4101824909771,-0.165810997523729,
3.5369536330429));
#41762=CARTESIAN_POINT('Ctrl Pts',(18.4578983270399,0.299801814449608,3.61009732380414));
#41763=CARTESIAN_POINT('Ctrl Pts',(18.5056141631028,0.49010200717001,4.04129464153984));
#41764=CARTESIAN_POINT('Ctrl Pts',(18.5451816061157,0.274694351318236,4.36741107590602));
#41765=CARTESIAN_POINT('Ctrl Pts',(18.5688437704409,0.0678526130816757,
4.41522900951301));
#41766=CARTESIAN_POINT('Ctrl Pts',(18.5766006560786,2.82854505807215E-5,
4.41518799822097));
#41767=CARTESIAN_POINT('Ctrl Pts',(18.3733993439214,0.000382963303967157,
4.41588626824893));
#41768=CARTESIAN_POINT('Ctrl Pts',(18.3856472566872,-0.106256708375174,
4.41489942083623));
#41769=CARTESIAN_POINT('Ctrl Pts',(18.4138004481407,-0.352960303644862,
4.31875095920395));
#41770=CARTESIAN_POINT('Ctrl Pts',(18.4578589182817,-0.482217355384067,
3.90319273261591));
#41771=CARTESIAN_POINT('Ctrl Pts',(18.5055747543446,-0.179376629827252,
3.54203793877243));
#41772=CARTESIAN_POINT('Ctrl Pts',(18.5532905904074,0.288188414964166,3.60143675240633));
#41773=CARTESIAN_POINT('Ctrl Pts',(18.6010064264702,0.491105603945206,4.02684232898929));
#41774=CARTESIAN_POINT('Ctrl Pts',(18.6410426776416,0.282958802096416,4.36309886994028));
#41775=CARTESIAN_POINT('Ctrl Pts',(18.6651736501253,0.0718833454275778,
4.41512900400112));
#41776=CARTESIAN_POINT('Ctrl Pts',(18.6733993439214,-3.94222854199489E-5,
4.41518963037823));
#41777=CARTESIAN_POINT('Origin',(3.42660065607856,0.,4.));
#41778=CARTESIAN_POINT('',(17.9766006560786,-0.000210814279110197,4.41643020456723));
#41779=CARTESIAN_POINT('',(18.0733993439214,-0.000144384975211464,4.41650095473263));
#41780=CARTESIAN_POINT('',(3.42660065607856,4.87367679877478E-13,4.415875));
#41781=CARTESIAN_POINT('Ctrl Pts',(17.9766006560786,-0.000210814279110157,
4.41643020456723));
#41782=CARTESIAN_POINT('Ctrl Pts',(17.9779804261896,-0.0121834889824064,
4.41650424974197));
#41783=CARTESIAN_POINT('Ctrl Pts',(17.9952654749882,-0.162096873242269,
4.41059855206721));
#41784=CARTESIAN_POINT('Ctrl Pts',(18.0284558024744,-0.435175833605105,
4.22918817311999));
#41785=CARTESIAN_POINT('Ctrl Pts',(18.0761716385373,-0.428137176707308,
3.75791781814212));
#41786=CARTESIAN_POINT('Ctrl Pts',(18.1238874746,-0.0279335627019553,3.5089552556775));
#41787=CARTESIAN_POINT('Ctrl Pts',(18.1716033106629,0.397921871745719,3.71092663761881));
#41788=CARTESIAN_POINT('Ctrl Pts',(18.2193191467257,0.458359528554279,4.17835853620019));
#41789=CARTESIAN_POINT('Ctrl Pts',(18.2543182618643,0.193950155243433,4.40107745006558));
#41790=CARTESIAN_POINT('Ctrl Pts',(18.2734120983152,0.0281121206155762,
4.41626771302466));
#41791=CARTESIAN_POINT('Ctrl Pts',(18.2766006560785,0.000371443240938293,
4.41601098728712));
#41792=CARTESIAN_POINT('Ctrl Pts',(18.0733993439214,-0.000144384975211439,
4.41650095473263));
#41793=CARTESIAN_POINT('Ctrl Pts',(18.0743103058739,-0.00804551399413891,
4.41653639380418));
#41794=CARTESIAN_POINT('Ctrl Pts',(18.0911265465141,-0.153864670001157,
4.41274680364665));
#41795=CARTESIAN_POINT('Ctrl Pts',(18.1238480658419,-0.428237044548737,
4.24190547436581));
#41796=CARTESIAN_POINT('Ctrl Pts',(18.1715639019047,-0.435081213444543,
3.7706322547532));
#41797=CARTESIAN_POINT('Ctrl Pts',(18.2192797379675,-0.0423836094492617,
3.50999096487715));
#41798=CARTESIAN_POINT('Ctrl Pts',(18.2669955740304,0.389235515258945,3.69933251171255));
#41799=CARTESIAN_POINT('Ctrl Pts',(18.3147114100932,0.463413677146622,4.16478163940629));
#41800=CARTESIAN_POINT('Ctrl Pts',(18.3501793333902,0.202226156869028,4.39827758107438));
#41801=CARTESIAN_POINT('Ctrl Pts',(18.3697419779996,0.0322267809866215,
4.41618095209965));
#41802=CARTESIAN_POINT('Ctrl Pts',(18.3733993439214,0.000382963303967157,
4.41588626824893));
#41803=CARTESIAN_POINT('Origin',(3.42660065607856,0.,4.));
#41804=CARTESIAN_POINT('',(17.6766006560786,-0.000263771022561219,4.41536107794487));
#41805=CARTESIAN_POINT('',(17.7733993439214,-0.000309142357869163,4.41544738986064));
#41806=CARTESIAN_POINT('',(3.42660065607856,4.87367679877478E-13,4.415875));
#41807=CARTESIAN_POINT('Ctrl Pts',(17.6766006560786,-0.000263771022561289,
4.41536107794487));
#41808=CARTESIAN_POINT('Ctrl Pts',(17.6825487540639,-0.0522183410383149,
4.41566152300153));
#41809=CARTESIAN_POINT('Ctrl Pts',(17.7044021307368,-0.24273028972288,4.38249735042552));
#41810=CARTESIAN_POINT('Ctrl Pts',(17.7421607860973,-0.48225726547346,4.09660825404716));
#41811=CARTESIAN_POINT('Ctrl Pts',(17.7898766221602,-0.342084653792828,
3.64661166616396));
#41812=CARTESIAN_POINT('Ctrl Pts',(17.837592458223,0.112229559114723,3.52113702282083));
#41813=CARTESIAN_POINT('Ctrl Pts',(17.8853082942859,0.463481641013499,3.83540961967535));
#41814=CARTESIAN_POINT('Ctrl Pts',(17.9316443602377,0.391261919872151,4.28736986940801));
#41815=CARTESIAN_POINT('Ctrl Pts',(17.962075147502,0.125831334120538,4.41565069513148));
#41816=CARTESIAN_POINT('Ctrl Pts',(17.9766006560786,-0.000210814279110157,
4.41643020456723));
#41817=CARTESIAN_POINT('Ctrl Pts',(17.7733993439214,-0.000309142357869142,
4.41544738986064));
#41818=CARTESIAN_POINT('Ctrl Pts',(17.7788786337482,-0.0481438769258273,
4.41577602216682));
#41819=CARTESIAN_POINT('Ctrl Pts',(17.8002632022627,-0.23443694547481,4.38601982759396));
#41820=CARTESIAN_POINT('Ctrl Pts',(17.8375530494648,-0.479202773223469,
4.11076970247734));
#41821=CARTESIAN_POINT('Ctrl Pts',(17.8852688855277,-0.352344189444135,
3.65683998336499));
#41822=CARTESIAN_POINT('Ctrl Pts',(17.9329847215905,0.0980774850139738,
3.51803938772416));
#41823=CARTESIAN_POINT('Ctrl Pts',(17.9807005576534,0.458433095867658,3.82183063825345));
#41824=CARTESIAN_POINT('Ctrl Pts',(18.0275054317636,0.3989600628602,4.28031410431705));
#41825=CARTESIAN_POINT('Ctrl Pts',(18.0584050271863,0.129907183855675,4.41591763216682));
#41826=CARTESIAN_POINT('Ctrl Pts',(18.0733993439214,-0.000144384975211439,
4.41650095473263));
#41827=CARTESIAN_POINT('Origin',(3.42660065607856,0.,4.));
#41828=CARTESIAN_POINT('',(17.3766006560786,0.000316824918469052,4.41546566829253));
#41829=CARTESIAN_POINT('',(17.4733993439214,0.000273208168652644,4.41537657040552));
#41830=CARTESIAN_POINT('',(3.42660065607856,4.87367679877478E-13,4.415875));
#41831=CARTESIAN_POINT('Ctrl Pts',(17.3766006560786,0.000316824918469058,
4.41546566829253));
#41832=CARTESIAN_POINT('Ctrl Pts',(17.3871170819382,-0.0914824399419538,
4.4148173972429));
#41833=CARTESIAN_POINT('Ctrl Pts',(17.4135387864855,-0.323087181591141,
4.33950699049548));
#41834=CARTESIAN_POINT('Ctrl Pts',(17.4558657697204,-0.489877595596684,
3.956123284257));
#41835=CARTESIAN_POINT('Ctrl Pts',(17.5035816057832,-0.228040769637767,
3.56422180844494));
#41836=CARTESIAN_POINT('Ctrl Pts',(17.551297441846,0.243209403937772,3.57250215124727));
#41837=CARTESIAN_POINT('Ctrl Pts',(17.5990132779089,0.491116639619549,3.97336034645914));
#41838=CARTESIAN_POINT('Ctrl Pts',(17.6407810159864,0.313340775136121,4.34566293955037));
#41839=CARTESIAN_POINT('Ctrl Pts',(17.6666434753763,0.0867087440962768,
4.41485812965324));
#41840=CARTESIAN_POINT('Ctrl Pts',(17.6766006560786,-0.000263771022561289,
4.41536107794487));
#41841=CARTESIAN_POINT('Ctrl Pts',(17.4733993439214,0.000273208168652693,
4.41537657040552));
#41842=CARTESIAN_POINT('Ctrl Pts',(17.4834469616226,-0.0874810350323011,
4.41484969107387));
#41843=CARTESIAN_POINT('Ctrl Pts',(17.5093998580114,-0.314919534962053,
4.34468516187688));
#41844=CARTESIAN_POINT('Ctrl Pts',(17.5512580330878,-0.490957336521241,
3.97057010757845));
#41845=CARTESIAN_POINT('Ctrl Pts',(17.5989738691507,-0.240776309167652,
3.57112706567612));
#41846=CARTESIAN_POINT('Ctrl Pts',(17.6466897052135,0.230513307714322,3.56552463842171));
#41847=CARTESIAN_POINT('Ctrl Pts',(17.6944055412763,0.490119007219086,3.95890762096741));
#41848=CARTESIAN_POINT('Ctrl Pts',(17.7366420875123,0.321513805022658,4.34052027563639));
#41849=CARTESIAN_POINT('Ctrl Pts',(17.7629733550606,0.090710757213051,4.41482206853766));
#41850=CARTESIAN_POINT('Ctrl Pts',(17.7733993439214,-0.000309142357869142,
4.41544738986064));
#41851=CARTESIAN_POINT('Origin',(3.42660065607856,0.,4.));
#41852=CARTESIAN_POINT('',(17.0766006560786,0.000130763213737631,4.41651185352269));
#41853=CARTESIAN_POINT('',(17.1733993439214,0.000198609043858391,4.41644558073401));
#41854=CARTESIAN_POINT('',(3.42660065607856,4.87367679877478E-13,4.415875));
#41855=CARTESIAN_POINT('Ctrl Pts',(17.0766006560786,0.000130763213737628,
4.41651185352269));
#41856=CARTESIAN_POINT('Ctrl Pts',(17.0916854098125,-0.130696083011285,
4.41597403242798));
#41857=CARTESIAN_POINT('Ctrl Pts',(17.1226754422341,-0.400436570105288,
4.2789290971087));
#41858=CARTESIAN_POINT('Ctrl Pts',(17.1695707533433,-0.457413284126125,
3.81922856321607));
#41859=CARTESIAN_POINT('Ctrl Pts',(17.2172865894061,-0.0953372598908034,
3.51748986360026));
#41860=CARTESIAN_POINT('Ctrl Pts',(17.265002425469,0.354288437054553,3.6588476466131));
#41861=CARTESIAN_POINT('Ctrl Pts',(17.3127182615318,0.478565610824392,4.11349088504481));
#41862=CARTESIAN_POINT('Ctrl Pts',(17.349917671735,0.232837083242772,4.38668157013213));
#41863=CARTESIAN_POINT('Ctrl Pts',(17.3712118032506,0.0473568302064652,
4.41579785693967));
#41864=CARTESIAN_POINT('Ctrl Pts',(17.3766006560786,0.000316824918469058,
4.41546566829253));
#41865=CARTESIAN_POINT('Ctrl Pts',(17.1733993439214,0.000198609043858397,
4.41644558073401));
#41866=CARTESIAN_POINT('Ctrl Pts',(17.1880152894969,-0.126615914365149,
4.41569892234974));
#41867=CARTESIAN_POINT('Ctrl Pts',(17.2185365137601,-0.392752582168809,
4.28602487069057));
#41868=CARTESIAN_POINT('Ctrl Pts',(17.2649630167107,-0.462538907526291,
3.83277863809798));
#41869=CARTESIAN_POINT('Ctrl Pts',(17.3126788527736,-0.109506707187599,
3.52050703244687));
#41870=CARTESIAN_POINT('Ctrl Pts',(17.3603946888365,0.344087187338735,3.64856119684745));
#41871=CARTESIAN_POINT('Ctrl Pts',(17.4081105248993,0.481700523269991,4.09934702176407));
#41872=CARTESIAN_POINT('Ctrl Pts',(17.4457787432609,0.241130489326423,4.3831889686244));
#41873=CARTESIAN_POINT('Ctrl Pts',(17.467541682935,0.0514330574063097,4.41568373580506));
#41874=CARTESIAN_POINT('Ctrl Pts',(17.4733993439214,0.000273208168652693,
4.41537657040552));
#41875=CARTESIAN_POINT('Origin',(3.42660065607856,0.,4.));
#41876=CARTESIAN_POINT('',(16.7766006560786,-0.000383680820852129,4.41586226484778));
#41877=CARTESIAN_POINT('',(16.8733993439214,-0.000374684679869397,4.41598699190495));
#41878=CARTESIAN_POINT('',(3.42660065607856,4.87367679877478E-13,4.415875));
#41879=CARTESIAN_POINT('Ctrl Pts',(16.7766006560786,-0.000383680820852189,
4.41586226484779));
#41880=CARTESIAN_POINT('Ctrl Pts',(16.7803484589992,-0.0330197262611539,
4.41616320579436));
#41881=CARTESIAN_POINT('Ctrl Pts',(16.8000015406075,-0.203823433586872,
4.39772119122577));
#41882=CARTESIAN_POINT('Ctrl Pts',(16.8355599009034,-0.464342533291602,
4.16214572651883));
#41883=CARTESIAN_POINT('Ctrl Pts',(16.8832757369663,-0.387520750342007,
3.69712561530174));
#41884=CARTESIAN_POINT('Ctrl Pts',(16.9309915730291,0.0451673004198413,
3.51023971187451));
#41885=CARTESIAN_POINT('Ctrl Pts',(16.978707409092,0.436377524217892,3.7731082169636));
#41886=CARTESIAN_POINT('Ctrl Pts',(17.0264232451548,0.426855552995382,4.24433493759383));
#41887=CARTESIAN_POINT('Ctrl Pts',(17.0590543274837,0.152277829190936,4.41314658311127));
#41888=CARTESIAN_POINT('Ctrl Pts',(17.0757801311249,0.00724700082869906,
4.41654110793655));
#41889=CARTESIAN_POINT('Ctrl Pts',(17.0766006560786,0.000130763213737628,
4.41651185352269));
#41890=CARTESIAN_POINT('Ctrl Pts',(16.8733993439214,-0.000374684679869387,
4.41598699190495));
#41891=CARTESIAN_POINT('Ctrl Pts',(16.8766783386836,-0.0289064002234668,
4.4162516892709));
#41892=CARTESIAN_POINT('Ctrl Pts',(16.8958626121335,-0.195546116663039,
4.40054826733105));
#41893=CARTESIAN_POINT('Ctrl Pts',(16.9309521642709,-0.459365614209645,
4.17575112327883));
#41894=CARTESIAN_POINT('Ctrl Pts',(16.9786680003337,-0.396272847821079,
3.70867019559999));
#41895=CARTESIAN_POINT('Ctrl Pts',(17.0263838363966,0.0307233721630972,
3.5091219099869));
#41896=CARTESIAN_POINT('Ctrl Pts',(17.0740996724594,0.429505846750062,3.76035452756312));
#41897=CARTESIAN_POINT('Ctrl Pts',(17.1218155085223,0.433866493469502,4.23165726989771));
#41898=CARTESIAN_POINT('Ctrl Pts',(17.1549153990096,0.160507997039396,4.41102293437065));
#41899=CARTESIAN_POINT('Ctrl Pts',(17.1721100108093,0.0113854435377776,
4.41651144656345));
#41900=CARTESIAN_POINT('Ctrl Pts',(17.1733993439214,0.000198609043858397,
4.41644558073401));
#41901=CARTESIAN_POINT('Origin',(3.42660065607856,0.,4.));
#41902=CARTESIAN_POINT('',(16.4766006560786,5.2409936866527E-5,4.41519222098806));
#41903=CARTESIAN_POINT('',(16.5733993439214,-1.52272386678698E-5,4.41518677123726));
#41904=CARTESIAN_POINT('',(3.42660065607856,4.87367679877478E-13,4.415875));
#41905=CARTESIAN_POINT('Ctrl Pts',(16.4766006560786,5.2409936866539E-5,
4.41519222098806));
#41906=CARTESIAN_POINT('Ctrl Pts',(16.4849167868736,-0.0726599781719204,
4.41511070701236));
#41907=CARTESIAN_POINT('Ctrl Pts',(16.5091381963562,-0.284551613766983,
4.36224737480062));
#41908=CARTESIAN_POINT('Ctrl Pts',(16.5492648845264,-0.4912502013546,4.02405128938415));
#41909=CARTESIAN_POINT('Ctrl Pts',(16.5969807205893,-0.285919008936969,
3.59980561575594));
#41910=CARTESIAN_POINT('Ctrl Pts',(16.6446965566521,0.181976008816936,3.54306460296116));
#41911=CARTESIAN_POINT('Ctrl Pts',(16.6924123927149,0.482759657613431,3.90593439612197));
#41912=CARTESIAN_POINT('Ctrl Pts',(16.7363804258571,0.351413532087107,4.31989995948535));
#41913=CARTESIAN_POINT('Ctrl Pts',(16.7644431803116,0.105484194296011,4.41488604428797));
#41914=CARTESIAN_POINT('Ctrl Pts',(16.7766006560786,-0.000383680820852189,
4.41586226484779));
#41915=CARTESIAN_POINT('Ctrl Pts',(16.5733993439214,-1.52272386678906E-5,
4.41518677123726));
#41916=CARTESIAN_POINT('Ctrl Pts',(16.5812466665579,-0.0686308195205231,
4.41520910309265));
#41917=CARTESIAN_POINT('Ctrl Pts',(16.6049992678821,-0.276289552895371,
4.36659242126669));
#41918=CARTESIAN_POINT('Ctrl Pts',(16.6446571478939,-0.490328743065594,
4.03850907134293));
#41919=CARTESIAN_POINT('Ctrl Pts',(16.6923729839567,-0.297581432841348,
3.60840005658827));
#41920=CARTESIAN_POINT('Ctrl Pts',(16.7400888200196,0.168439486040012,3.53790329540825));
#41921=CARTESIAN_POINT('Ctrl Pts',(16.7878046560824,0.479779833116189,3.89175704832657));
#41922=CARTESIAN_POINT('Ctrl Pts',(16.832241497383,0.359412856911567,4.31386464726761));
#41923=CARTESIAN_POINT('Ctrl Pts',(16.860773059996,0.109491163683573,4.41496773315674));
#41924=CARTESIAN_POINT('Ctrl Pts',(16.8733993439214,-0.000374684679869387,
4.41598699190495));
#41925=CARTESIAN_POINT('Origin',(3.42660065607856,0.,4.));
#41926=CARTESIAN_POINT('',(16.1766006560786,0.000364146841390381,4.41605523138122));
#41927=CARTESIAN_POINT('',(16.2733993439214,0.000380345806842055,4.41593091837313));
#41928=CARTESIAN_POINT('',(3.42660065607856,4.87367679877478E-13,4.415875));
#41929=CARTESIAN_POINT('Ctrl Pts',(16.1766006560786,0.000364146841390366,
4.41605523138122));
#41930=CARTESIAN_POINT('Ctrl Pts',(16.1894851147479,-0.111700864104492,
4.41502624848758));
#41931=CARTESIAN_POINT('Ctrl Pts',(16.2182748521048,-0.363797281821349,
4.31045679267864));
#41932=CARTESIAN_POINT('Ctrl Pts',(16.2629698681494,-0.477960913216358,
3.88398883549692));
#41933=CARTESIAN_POINT('Ctrl Pts',(16.3106857042122,-0.160921706883503,
3.53523185446324));
#41934=CARTESIAN_POINT('Ctrl Pts',(16.358401540275,0.303894378979202,3.6132786128531));
#41935=CARTESIAN_POINT('Ctrl Pts',(16.4061173763379,0.489639580609251,4.04645757153336));
#41936=CARTESIAN_POINT('Ctrl Pts',(16.4455170816057,0.271734615807756,4.36891289568356));
#41937=CARTESIAN_POINT('Ctrl Pts',(16.4690115081859,0.0664083969439258,
4.41526660914191));
#41938=CARTESIAN_POINT('Ctrl Pts',(16.4766006560786,5.2409936866539E-5,
4.41519222098806));
#41939=CARTESIAN_POINT('Ctrl Pts',(16.2733993439214,0.000380345806842052,
4.41593091837313));
#41940=CARTESIAN_POINT('Ctrl Pts',(16.2858149944323,-0.107690075887363,
4.41492720978183));
#41941=CARTESIAN_POINT('Ctrl Pts',(16.3141359236307,-0.35582464097624,4.31660057631701));
#41942=CARTESIAN_POINT('Ctrl Pts',(16.3583621315169,-0.481170314810987,
3.89811598262401));
#41943=CARTESIAN_POINT('Ctrl Pts',(16.4060779675797,-0.174540169679895,
3.54017290856226));
#41944=CARTESIAN_POINT('Ctrl Pts',(16.4537938036425,0.292372898913969,3.60449612791703));
#41945=CARTESIAN_POINT('Ctrl Pts',(16.5015096397054,0.490795435699827,4.0320166386149));
#41946=CARTESIAN_POINT('Ctrl Pts',(16.5413781531317,0.280003220364278,4.36466130212541));
#41947=CARTESIAN_POINT('Ctrl Pts',(16.5653413878703,0.0704421061260754,
4.4151638399628));
#41948=CARTESIAN_POINT('Ctrl Pts',(16.5733993439214,-1.52272386678906E-5,
4.41518677123726));
#41949=CARTESIAN_POINT('Origin',(3.42660065607856,0.,4.));
#41950=CARTESIAN_POINT('',(15.8766006560786,-0.00023258108979477,4.41639972388928));
#41951=CARTESIAN_POINT('',(15.9733993439214,-0.000169011902647176,4.4164782780785));
#41952=CARTESIAN_POINT('',(3.42660065607856,4.87367679877478E-13,4.415875));
#41953=CARTESIAN_POINT('Ctrl Pts',(15.8766006560786,-0.000232581089794846,
4.41639972388928));
#41954=CARTESIAN_POINT('Ctrl Pts',(15.8781481639346,-0.0136633580705269,
4.41648966084242));
#41955=CARTESIAN_POINT('Ctrl Pts',(15.8956009504782,-0.165044849757219,
4.40979870506104));
#41956=CARTESIAN_POINT('Ctrl Pts',(15.9289590157095,-0.437567097060412,
4.22458909239344));
#41957=CARTESIAN_POINT('Ctrl Pts',(15.9766748517724,-0.425562075928853,
3.75341909160864));
#41958=CARTESIAN_POINT('Ctrl Pts',(16.0243906878352,-0.0227568523576073,
3.50868813313462));
#41959=CARTESIAN_POINT('Ctrl Pts',(16.072106523898,0.400946338892803,3.71513642180785));
#41960=CARTESIAN_POINT('Ctrl Pts',(16.1198223599609,0.456454337785543,4.1831793175245));
#41961=CARTESIAN_POINT('Ctrl Pts',(16.1546537373544,0.190990792023167,4.40204523666471));
#41962=CARTESIAN_POINT('Ctrl Pts',(16.1735798360603,0.0266382990664043,
4.41629648110721));
#41963=CARTESIAN_POINT('Ctrl Pts',(16.1766006560786,0.000364146841390366,
4.41605523138122));
#41964=CARTESIAN_POINT('Ctrl Pts',(15.9733993439214,-0.000169011902647174,
4.4164782780785));
#41965=CARTESIAN_POINT('Ctrl Pts',(15.974478043619,-0.00952634975615679,
4.4165263696097));
#41966=CARTESIAN_POINT('Ctrl Pts',(15.9914620220042,-0.156808910032117,
4.4119928338179));
#41967=CARTESIAN_POINT('Ctrl Pts',(16.024351279077,-0.430762722000766,4.23737881579128));
#41968=CARTESIAN_POINT('Ctrl Pts',(16.0720671151398,-0.432639725453012,
3.76605963834362));
#41969=CARTESIAN_POINT('Ctrl Pts',(16.1197829512026,-0.0372170120039125,
3.50957149464017));
#41970=CARTESIAN_POINT('Ctrl Pts',(16.1674987872655,0.392382656225717,3.70345139362117));
#41971=CARTESIAN_POINT('Ctrl Pts',(16.2152146233283,0.461651293660056,4.16965644082667));
#41972=CARTESIAN_POINT('Ctrl Pts',(16.2505148088803,0.199264245432362,4.39929555075695));
#41973=CARTESIAN_POINT('Ctrl Pts',(16.2699097157447,0.0307553622657438,
4.41621302761729));
#41974=CARTESIAN_POINT('Ctrl Pts',(16.2733993439214,0.000380345806842052,
4.41593091837313));
#41975=CARTESIAN_POINT('Origin',(3.42660065607856,0.,4.));
#41976=CARTESIAN_POINT('',(15.5766006560786,-0.000245472137683418,4.41533389801214));
#41977=CARTESIAN_POINT('',(15.6733993439214,-0.00029394562308721,4.41541483535501));
#41978=CARTESIAN_POINT('',(3.42660065607856,4.87367679877478E-13,4.415875));
#41979=CARTESIAN_POINT('Ctrl Pts',(15.5766006560786,-0.000245472137683396,
4.41533389801214));
#41980=CARTESIAN_POINT('Ctrl Pts',(15.5827164918089,-0.0536739331835165,
4.41562024719655));
#41981=CARTESIAN_POINT('Ctrl Pts',(15.6047376062269,-0.245697356182912,
4.38119912149661));
#41982=CARTESIAN_POINT('Ctrl Pts',(15.6426639993325,-0.483248643997369,
4.09152034160055));
#41983=CARTESIAN_POINT('Ctrl Pts',(15.6903798353953,-0.338341267922855,
3.64302603558196));
#41984=CARTESIAN_POINT('Ctrl Pts',(15.7380956714582,0.117270100534806,3.52234641383892));
#41985=CARTESIAN_POINT('Ctrl Pts',(15.785811507521,0.465190531238913,3.84030342991275));
#41986=CARTESIAN_POINT('Ctrl Pts',(15.8319798357278,0.388490242362186,4.28984418805176));
#41987=CARTESIAN_POINT('Ctrl Pts',(15.862242885247,0.124378106492246,4.41556528924811));
#41988=CARTESIAN_POINT('Ctrl Pts',(15.8766006560786,-0.000232581089794846,
4.41639972388928));
#41989=CARTESIAN_POINT('Ctrl Pts',(15.6733993439214,-0.000293945623087231,
4.41541483535501));
#41990=CARTESIAN_POINT('Ctrl Pts',(15.6790463714933,-0.0496027558454661,
4.41573527017753));
#41991=CARTESIAN_POINT('Ctrl Pts',(15.7005986777528,-0.23740431922453,4.38477730872224));
#41992=CARTESIAN_POINT('Ctrl Pts',(15.7380562626999,-0.480343569999647,
4.1057131950703));
#41993=CARTESIAN_POINT('Ctrl Pts',(15.7857720987628,-0.348708030819167,
3.6531456586776));
#41994=CARTESIAN_POINT('Ctrl Pts',(15.8334879348256,0.103151458625294,3.5190998009613));
#41995=CARTESIAN_POINT('Ctrl Pts',(15.8812037708885,0.460285376424935,3.82667199562295));
#41996=CARTESIAN_POINT('Ctrl Pts',(15.9278409072537,0.396214095655672,4.28286244744368));
#41997=CARTESIAN_POINT('Ctrl Pts',(15.9585727649314,0.128446309981357,4.41581726659612));
#41998=CARTESIAN_POINT('Ctrl Pts',(15.9733993439214,-0.000169011902647174,
4.4164782780785));
#41999=CARTESIAN_POINT('Origin',(3.42660065607856,0.,4.));
#42000=CARTESIAN_POINT('',(15.2766006560786,0.000330084823988869,4.41550084660604));
#42001=CARTESIAN_POINT('',(15.3733993439214,0.000289868078815952,4.41540680128743));
#42002=CARTESIAN_POINT('',(3.42660065607856,4.87367679877478E-13,4.415875));
#42003=CARTESIAN_POINT('Ctrl Pts',(15.2766006560786,0.000330084823988861,
4.41550084660604));
#42004=CARTESIAN_POINT('Ctrl Pts',(15.2872848196833,-0.0929135079625664,
4.41481081573461));
#42005=CARTESIAN_POINT('Ctrl Pts',(15.3138742619755,-0.32600240339937,4.33760928826424));
#42006=CARTESIAN_POINT('Ctrl Pts',(15.3563689829555,-0.489387968817152,
3.95096286275689));
#42007=CARTESIAN_POINT('Ctrl Pts',(15.4040848190183,-0.223435404337718,
3.56184267101825));
#42008=CARTESIAN_POINT('Ctrl Pts',(15.4518006550811,0.24770132994065,3.57508909640066));
#42009=CARTESIAN_POINT('Ctrl Pts',(15.499516491144,0.491370121559653,3.97853774265298));
#42010=CARTESIAN_POINT('Ctrl Pts',(15.5411164914764,0.310410063586636,4.3474585185963));
#42011=CARTESIAN_POINT('Ctrl Pts',(15.5668112131213,0.0852759340546689,
4.41487554708019));
#42012=CARTESIAN_POINT('Ctrl Pts',(15.5766006560786,-0.000245472137683396,
4.41533389801214));
#42013=CARTESIAN_POINT('Ctrl Pts',(15.3733993439214,0.000289868078815973,
4.41540680128743));
#42014=CARTESIAN_POINT('Ctrl Pts',(15.3836146993676,-0.0889130762729256,
4.41483587894927));
#42015=CARTESIAN_POINT('Ctrl Pts',(15.4097353335015,-0.317845114095608,
4.34285359523591));
#42016=CARTESIAN_POINT('Ctrl Pts',(15.4517612463229,-0.490619905976795,
3.96539750426199));
#42017=CARTESIAN_POINT('Ctrl Pts',(15.4994770823858,-0.236243011612202,
3.56861332390027));
#42018=CARTESIAN_POINT('Ctrl Pts',(15.5471929184486,0.235079475381852,3.56797816593814));
#42019=CARTESIAN_POINT('Ctrl Pts',(15.5949087545115,0.490524862970081,3.9640753057054));
#42020=CARTESIAN_POINT('Ctrl Pts',(15.6369775630024,0.318592711010818,4.34238143198936));
#42021=CARTESIAN_POINT('Ctrl Pts',(15.6631410928057,0.0892792238074376,
4.41483274135358));
#42022=CARTESIAN_POINT('Ctrl Pts',(15.6733993439214,-0.000293945623087231,
4.41541483535501));
#42023=CARTESIAN_POINT('Origin',(3.42660065607856,0.,4.));
#42024=CARTESIAN_POINT('',(14.9766006560786,0.000104941934236194,4.41652945172571));
#42025=CARTESIAN_POINT('',(15.0733993439214,0.000175165248676303,4.41647198785975));
#42026=CARTESIAN_POINT('',(3.42660065607856,4.87367679877478E-13,4.415875));
#42027=CARTESIAN_POINT('Ctrl Pts',(14.9766006560786,0.000104941934236227,
4.41652945172572));
#42028=CARTESIAN_POINT('Ctrl Pts',(14.9918531475576,-0.132161740438444,
4.41608294134065));
#42029=CARTESIAN_POINT('Ctrl Pts',(15.0230109177242,-0.40316752945992,4.27633971254324));
#42030=CARTESIAN_POINT('Ctrl Pts',(15.0700739665785,-0.455482716161518,
3.8144178884426));
#42031=CARTESIAN_POINT('Ctrl Pts',(15.1177898026413,-0.0902467530057116,
3.51651189422706));
#42032=CARTESIAN_POINT('Ctrl Pts',(15.1655056387041,0.357864192060027,3.66260046696357));
#42033=CARTESIAN_POINT('Ctrl Pts',(15.2132214747669,0.47734294310866,4.11852822244656));
#42034=CARTESIAN_POINT('Ctrl Pts',(15.2502531472251,0.229869832763757,4.3878938710325));
#42035=CARTESIAN_POINT('Ctrl Pts',(15.2713795409956,0.0458961718568525,
4.41583804947224));
#42036=CARTESIAN_POINT('Ctrl Pts',(15.2766006560786,0.000330084823988861,
4.41550084660604));
#42037=CARTESIAN_POINT('Ctrl Pts',(15.0733993439214,0.000175165248676341,
4.41647198785975));
#42038=CARTESIAN_POINT('Ctrl Pts',(15.0881830272419,-0.128073190246274,
4.41579247653651));
#42039=CARTESIAN_POINT('Ctrl Pts',(15.1188719892501,-0.395510344386944,
4.28350986851547));
#42040=CARTESIAN_POINT('Ctrl Pts',(15.1654662299459,-0.46075086019608,3.82791319143947));
#42041=CARTESIAN_POINT('Ctrl Pts',(15.2131820660087,-0.104447211543591,
3.51937956259357));
#42042=CARTESIAN_POINT('Ctrl Pts',(15.2608979020716,0.347771918596306,3.652207076714));
#42043=CARTESIAN_POINT('Ctrl Pts',(15.3086137381344,0.480626744730421,4.10441818376995));
#42044=CARTESIAN_POINT('Ctrl Pts',(15.346114218751,0.238163166260598,4.38445638366753));
#42045=CARTESIAN_POINT('Ctrl Pts',(15.36770942068,0.0499756483669043,4.41572480336754));
#42046=CARTESIAN_POINT('Ctrl Pts',(15.3733993439214,0.000289868078815973,
4.41540680128743));
#42047=CARTESIAN_POINT('Origin',(3.42660065607856,0.,4.));
#42048=CARTESIAN_POINT('',(14.6766006560786,-0.000383732061438463,4.41581798673635));
#42049=CARTESIAN_POINT('',(14.7733993439214,-0.000379407362125217,4.41594234696178));
#42050=CARTESIAN_POINT('',(3.42660065607856,4.87367679877478E-13,4.415875));
#42051=CARTESIAN_POINT('Ctrl Pts',(14.6766006560786,-0.000383732061438387,
4.41581798673635));
#42052=CARTESIAN_POINT('Ctrl Pts',(14.6805161967443,-0.0344897130604965,
4.41612948839573));
#42053=CARTESIAN_POINT('Ctrl Pts',(14.7003370160976,-0.206786574235377,
4.39667515056147));
#42054=CARTESIAN_POINT('Ctrl Pts',(14.7360631141386,-0.466025611307368,
4.15724297904063));
#42055=CARTESIAN_POINT('Ctrl Pts',(14.7837789502014,-0.38430721152129,3.69305832471834));
#42056=CARTESIAN_POINT('Ctrl Pts',(14.8314947862642,0.0503264139313189,
3.51074293371195));
#42057=CARTESIAN_POINT('Ctrl Pts',(14.8792106223271,0.438744519099385,3.77771983486548));
#42058=CARTESIAN_POINT('Ctrl Pts',(14.9269264583899,0.42425678142631,4.24882003188202));
#42059=CARTESIAN_POINT('Ctrl Pts',(14.9593898029737,0.149335702075518,4.41387566524124));
#42060=CARTESIAN_POINT('Ctrl Pts',(14.97594786887,0.00576578747519492,4.41654856180149));
#42061=CARTESIAN_POINT('Ctrl Pts',(14.9766006560786,0.000104941934236227,
4.41652945172572));
#42062=CARTESIAN_POINT('Ctrl Pts',(14.7733993439214,-0.000379407362125234,
4.41594234696178));
#42063=CARTESIAN_POINT('Ctrl Pts',(14.7768460764287,-0.0303789312965351,
4.41622104989506));
#42064=CARTESIAN_POINT('Ctrl Pts',(14.7961980876235,-0.198506931257387,
4.39955296987463));
#42065=CARTESIAN_POINT('Ctrl Pts',(14.831455377506,-0.461192356972643,4.17090007232882));
#42066=CARTESIAN_POINT('Ctrl Pts',(14.8791712135689,-0.393180492164677,
3.7045100248179));
#42067=CARTESIAN_POINT('Ctrl Pts',(14.9268870496317,0.0358950684576197,
3.50947296821438));
#42068=CARTESIAN_POINT('Ctrl Pts',(14.9746028856945,0.432007635398663,3.76489443262817));
#42069=CARTESIAN_POINT('Ctrl Pts',(15.0223187217574,0.431400943461215,4.23621695712364));
#42070=CARTESIAN_POINT('Ctrl Pts',(15.0552508744997,0.157562060208247,4.41179740605063));
#42071=CARTESIAN_POINT('Ctrl Pts',(15.0722777485543,0.00990499767517082,
4.41652354042182));
#42072=CARTESIAN_POINT('Ctrl Pts',(15.0733993439214,0.000175165248676341,
4.41647198785975));
#42073=CARTESIAN_POINT('Origin',(3.42660065607856,0.,4.));
#42074=CARTESIAN_POINT('',(14.3766006560786,7.63317591858645E-5,4.41519896243726));
#42075=CARTESIAN_POINT('',(14.4733993439214,9.02664646690309E-6,4.41518644689786));
#42076=CARTESIAN_POINT('',(3.42660065607856,4.87367679877478E-13,4.415875));
#42077=CARTESIAN_POINT('Ctrl Pts',(14.3766006560786,7.63317591858798E-5,
4.41519896243726));
#42078=CARTESIAN_POINT('Ctrl Pts',(14.3850845246186,-0.0740996743586071,
4.41507773880187));
#42079=CARTESIAN_POINT('Ctrl Pts',(14.4094736718463,-0.287504468978829,
4.360651101065));
#42080=CARTESIAN_POINT('Ctrl Pts',(14.4497680977616,-0.491476396904638,
4.01887262932433));
#42081=CARTESIAN_POINT('Ctrl Pts',(14.4974839338244,-0.281685449746218,
3.59681451879656));
#42082=CARTESIAN_POINT('Ctrl Pts',(14.5451997698872,0.186781580201919,3.54500783946397));
#42083=CARTESIAN_POINT('Ctrl Pts',(14.59291560595,0.483724211046603,3.91102746210588));
#42084=CARTESIAN_POINT('Ctrl Pts',(14.6367159013472,0.348540265561382,4.32201186060262));
#42085=CARTESIAN_POINT('Ctrl Pts',(14.6646109180567,0.104051852208848,4.41486414061182));
#42086=CARTESIAN_POINT('Ctrl Pts',(14.6766006560786,-0.000383732061438387,
4.41581798673635));
#42087=CARTESIAN_POINT('Ctrl Pts',(14.4733993439214,9.0266464668684E-6,
4.41518644689786));
#42088=CARTESIAN_POINT('Ctrl Pts',(14.481414404303,-0.0700733710850898,
4.41517292627706));
#42089=CARTESIAN_POINT('Ctrl Pts',(14.5053347433722,-0.279247125311621,
4.3650573561381));
#42090=CARTESIAN_POINT('Ctrl Pts',(14.545160361129,-0.490707361486496,4.03333931965322));
#42091=CARTESIAN_POINT('Ctrl Pts',(14.5928761971918,-0.293437803431633,
3.60528557111603));
#42092=CARTESIAN_POINT('Ctrl Pts',(14.6405920332547,0.173300204635467,3.53970415608515));
#42093=CARTESIAN_POINT('Ctrl Pts',(14.6883078693175,0.480893968219416,3.89681949708321));
#42094=CARTESIAN_POINT('Ctrl Pts',(14.7325769728731,0.356556173733762,4.31604662460621));
#42095=CARTESIAN_POINT('Ctrl Pts',(14.760940797741,0.10805675748006,4.41493494840171));
#42096=CARTESIAN_POINT('Ctrl Pts',(14.7733993439214,-0.000379407362125234,
4.41594234696178));
#42097=CARTESIAN_POINT('Origin',(3.42660065607856,0.,4.));
#42098=CARTESIAN_POINT('',(14.0766006560786,0.000355193352615291,4.41609897421413));
#42099=CARTESIAN_POINT('',(14.1733993439214,0.000376051973931104,4.41597558743442));
#42100=CARTESIAN_POINT('',(3.42660065607856,4.87367679877478E-13,4.415875));
#42101=CARTESIAN_POINT('Ctrl Pts',(14.0766006560786,0.000355193352615277,
4.41609897421413));
#42102=CARTESIAN_POINT('Ctrl Pts',(14.0896528524929,-0.113137957382804,
4.41506966208575));
#42103=CARTESIAN_POINT('Ctrl Pts',(14.1186103275949,-0.366637448157006,
4.30821039815648));
#42104=CARTESIAN_POINT('Ctrl Pts',(14.1634730813845,-0.476711717661702,
3.87895801102093));
#42105=CARTESIAN_POINT('Ctrl Pts',(14.2111889174473,-0.156014541823709,
3.53356170012368));
#42106=CARTESIAN_POINT('Ctrl Pts',(14.2589047535102,0.307953188363286,3.61650285707861));
#42107=CARTESIAN_POINT('Ctrl Pts',(14.306620589573,0.4891227672074,4.05161534124029));
#42108=CARTESIAN_POINT('Ctrl Pts',(14.3458525570958,0.268773633406098,4.37039329245586));
#42109=CARTESIAN_POINT('Ctrl Pts',(14.369179245931,0.0649630708582953,4.4153050049005));
#42110=CARTESIAN_POINT('Ctrl Pts',(14.3766006560786,7.63317591858798E-5,
4.41519896243726));
#42111=CARTESIAN_POINT('Ctrl Pts',(14.1733993439214,0.000376051973931098,
4.41597558743442));
#42112=CARTESIAN_POINT('Ctrl Pts',(14.1859827321773,-0.109124255432428,
4.41495896305428));
#42113=CARTESIAN_POINT('Ctrl Pts',(14.2144713991208,-0.358682910161539,
4.31442504752535));
#42114=CARTESIAN_POINT('Ctrl Pts',(14.258865344752,-0.480069828122688,3.8930505494253));
#42115=CARTESIAN_POINT('Ctrl Pts',(14.3065811808148,-0.169684322438749,
3.53835895376334));
#42116=CARTESIAN_POINT('Ctrl Pts',(14.3542970168777,0.296524907469595,3.60759943412104));
#42117=CARTESIAN_POINT('Ctrl Pts',(14.4020128529405,0.49043075222644,4.0371873919842));
#42118=CARTESIAN_POINT('Ctrl Pts',(14.4417136286217,0.277046036654804,4.36620192284859));
#42119=CARTESIAN_POINT('Ctrl Pts',(14.4655091256154,0.0689998253659925,
4.41519975692232));
#42120=CARTESIAN_POINT('Ctrl Pts',(14.4733993439214,9.0266464668684E-6,
4.41518644689786));
#42121=CARTESIAN_POINT('Origin',(3.42660065607856,0.,4.));
#42122=CARTESIAN_POINT('',(13.7766006560786,-0.000253139125078747,4.41636688691614));
#42123=CARTESIAN_POINT('',(13.8733993439214,-0.000192710833643805,4.4164526008213));
#42124=CARTESIAN_POINT('',(3.42660065607856,4.87367679877478E-13,4.415875));
#42125=CARTESIAN_POINT('Ctrl Pts',(13.7766006560786,-0.000253139125078718,
4.41636688691614));
#42126=CARTESIAN_POINT('Ctrl Pts',(13.7783159016796,-0.0151427949580853,
4.41647347977994));
#42127=CARTESIAN_POINT('Ctrl Pts',(13.7959364259683,-0.167994124135391,
4.40898222403799));
#42128=CARTESIAN_POINT('Ctrl Pts',(13.8294622289446,-0.439909757638992,
4.21996506537626));
#42129=CARTESIAN_POINT('Ctrl Pts',(13.8771780650075,-0.422939705734467,
3.74894775411238));
#42130=CARTESIAN_POINT('Ctrl Pts',(13.9248939010703,-0.0175776142901187,
3.50847558318244));
#42131=CARTESIAN_POINT('Ctrl Pts',(13.9726097371332,0.403926270823208,3.71937784729135));
#42132=CARTESIAN_POINT('Ctrl Pts',(14.020325573196,0.454498446235019,4.18797975215946));
#42133=CARTESIAN_POINT('Ctrl Pts',(14.0549892128445,0.188032430710383,4.40299531219535));
#42134=CARTESIAN_POINT('Ctrl Pts',(14.0737475738053,0.0251636842930195,
4.41632397176197));
#42135=CARTESIAN_POINT('Ctrl Pts',(14.0766006560786,0.000355193352615277,
4.41609897421413));
#42136=CARTESIAN_POINT('Ctrl Pts',(13.8733993439214,-0.000192710833643682,
4.4164526008213));
#42137=CARTESIAN_POINT('Ctrl Pts',(13.874645781364,-0.0110068809386406,
4.41651469495978));
#42138=CARTESIAN_POINT('Ctrl Pts',(13.8917974974943,-0.15975450351916,4.41122255187585));
#42139=CARTESIAN_POINT('Ctrl Pts',(13.9248544923121,-0.433240552373761,
4.23282579030437));
#42140=CARTESIAN_POINT('Ctrl Pts',(13.9725703283749,-0.430150181893835,
3.76151300691929));
#42141=CARTESIAN_POINT('Ctrl Pts',(14.0202861644378,-0.032046280669499,
3.50920649887429));
#42142=CARTESIAN_POINT('Ctrl Pts',(14.0680020005006,0.39548621318905,3.70760321474174));
#42143=CARTESIAN_POINT('Ctrl Pts',(14.1157178365634,0.459837632138507,4.1745123976147));
#42144=CARTESIAN_POINT('Ctrl Pts',(14.1508502843704,0.196303200904851,4.40029544879449));
#42145=CARTESIAN_POINT('Ctrl Pts',(14.1700774534897,0.0292830534939708,
4.41624396624722));
#42146=CARTESIAN_POINT('Ctrl Pts',(14.1733993439214,0.000376051973931098,
4.41597558743442));
#42147=CARTESIAN_POINT('Origin',(3.42660065607856,0.,4.));
#42148=CARTESIAN_POINT('',(13.4766006560786,-0.000226204729293368,4.4153088088013));
#42149=CARTESIAN_POINT('',(13.5733993439214,-0.000277574767750837,4.41538411867388));
#42150=CARTESIAN_POINT('',(3.42660065607856,4.87367679877478E-13,4.415875));
#42151=CARTESIAN_POINT('Ctrl Pts',(13.4766006560786,-0.000226204729293314,
4.4153088088013));
#42152=CARTESIAN_POINT('Ctrl Pts',(13.482884229554,-0.0551283395969922,
4.41557894444213));
#42153=CARTESIAN_POINT('Ctrl Pts',(13.505073081717,-0.248664136397309,4.37988069596112));
#42154=CARTESIAN_POINT('Ctrl Pts',(13.5431672125676,-0.484186345555107,
4.08642226350871));
#42155=CARTESIAN_POINT('Ctrl Pts',(13.5908830486304,-0.334560300710407,
3.63948005597396));
#42156=CARTESIAN_POINT('Ctrl Pts',(13.6385988846933,0.122297616148583,3.52360886035071));
#42157=CARTESIAN_POINT('Ctrl Pts',(13.6863147207561,0.466847750307624,3.8452149784873));
#42158=CARTESIAN_POINT('Ctrl Pts',(13.7323153112179,0.38570983934117,4.29229218593957));
#42159=CARTESIAN_POINT('Ctrl Pts',(13.762410622992,0.122927301498021,4.41548505619568));
#42160=CARTESIAN_POINT('Ctrl Pts',(13.7766006560786,-0.000253139125078718,
4.41636688691614));
#42161=CARTESIAN_POINT('Ctrl Pts',(13.5733993439214,-0.000277574767750817,
4.41538411867388));
#42162=CARTESIAN_POINT('Ctrl Pts',(13.5792141092383,-0.0510604653080308,
4.41569425641003));
#42163=CARTESIAN_POINT('Ctrl Pts',(13.6009341532429,-0.240371663949131,
4.38351498152559));
#42164=CARTESIAN_POINT('Ctrl Pts',(13.6385594759351,-0.481431012491488,
4.10064494554323));
#42165=CARTESIAN_POINT('Ctrl Pts',(13.6862753119979,-0.345033139360895,
3.64948986092447));
#42166=CARTESIAN_POINT('Ctrl Pts',(13.7339911480608,0.108213974662067,3.52021363031051));
#42167=CARTESIAN_POINT('Ctrl Pts',(13.7817069841236,0.462086530666827,3.83153260544464));
#42168=CARTESIAN_POINT('Ctrl Pts',(13.8281763827438,0.393458703070077,4.28538422885222));
#42169=CARTESIAN_POINT('Ctrl Pts',(13.8587405026764,0.126988323162951,4.4157223370415));
#42170=CARTESIAN_POINT('Ctrl Pts',(13.8733993439214,-0.000192710833643682,
4.4164526008213));
#42171=CARTESIAN_POINT('Origin',(3.42660065607856,0.,4.));
#42172=CARTESIAN_POINT('',(13.1766006560786,0.000342007958933446,4.41553758638116));
#42173=CARTESIAN_POINT('',(13.2733993439214,0.000305371599794934,4.41543889539504));
#42174=CARTESIAN_POINT('',(3.42660065607856,4.87367679877478E-13,4.415875));
#42175=CARTESIAN_POINT('Ctrl Pts',(13.1766006560786,0.000342007958933428,
4.41553758638117));
#42176=CARTESIAN_POINT('Ctrl Pts',(13.1874525574283,-0.0943443719380771,
4.41480703635833));
#42177=CARTESIAN_POINT('Ctrl Pts',(13.2142097374657,-0.328913583769224,
4.33568767983454));
#42178=CARTESIAN_POINT('Ctrl Pts',(13.2568721961906,-0.488843983144383,
3.94580788806928));
#42179=CARTESIAN_POINT('Ctrl Pts',(13.3045880322534,-0.218805220893238,
3.55951220202843));
#42180=CARTESIAN_POINT('Ctrl Pts',(13.3523038683163,0.252165742455243,3.57772323864086));
#42181=CARTESIAN_POINT('Ctrl Pts',(13.4000197043791,0.491569024438394,3.98371752277252));
#42182=CARTESIAN_POINT('Ctrl Pts',(13.4414519669665,0.307476227900318,4.34923088347422));
#42183=CARTESIAN_POINT('Ctrl Pts',(13.4669789508664,0.0838425436168888,
4.41489516431802));
#42184=CARTESIAN_POINT('Ctrl Pts',(13.4766006560786,-0.000226204729293314,
4.4153088088013));
#42185=CARTESIAN_POINT('Ctrl Pts',(13.2733993439214,0.000305371599794949,
4.41543889539504));
#42186=CARTESIAN_POINT('Ctrl Pts',(13.2837824371127,-0.0903447040275099,
4.41482455235666));
#42187=CARTESIAN_POINT('Ctrl Pts',(13.3100708089916,-0.320767143545349,
4.3409984814332));
#42188=CARTESIAN_POINT('Ctrl Pts',(13.352264459558,-0.490227979701372,3.96022874442655));
#42189=CARTESIAN_POINT('Ctrl Pts',(13.3999802956209,-0.23168347330409,3.56614749850931));
#42190=CARTESIAN_POINT('Ctrl Pts',(13.4476961316837,0.239619531536799,3.57047968038978));
#42191=CARTESIAN_POINT('Ctrl Pts',(13.4954119677466,0.490876233547033,3.96924698078795));
#42192=CARTESIAN_POINT('Ctrl Pts',(13.5373130384925,0.315668023336251,4.34421900798688));
#42193=CARTESIAN_POINT('Ctrl Pts',(13.5633088305507,0.0878472949503496,
4.41484592860038));
#42194=CARTESIAN_POINT('Ctrl Pts',(13.5733993439214,-0.000277574767750817,
4.41538411867388));
#42195=CARTESIAN_POINT('Origin',(3.42660065607856,0.,4.));
#42196=CARTESIAN_POINT('',(12.8766006560786,7.85109994957766E-5,4.41654344863055));
#42197=CARTESIAN_POINT('',(12.9733993439214,0.000150764780949702,4.41649545414489));
#42198=CARTESIAN_POINT('',(3.42660065607856,4.87367679877478E-13,4.415875));
#42199=CARTESIAN_POINT('Ctrl Pts',(12.8766006560786,7.85109994958138E-5,
4.41654344863055));
#42200=CARTESIAN_POINT('Ctrl Pts',(12.8920208853026,-0.133630732206743,
4.41619751255639));
#42201=CARTESIAN_POINT('Ctrl Pts',(12.9233463932143,-0.405888408666218,
4.27372356364211));
#42202=CARTESIAN_POINT('Ctrl Pts',(12.9705771798136,-0.453501555338242,
3.80962782724943));
#42203=CARTESIAN_POINT('Ctrl Pts',(13.0182930158764,-0.0851462219395619,
3.51558762841831));
#42204=CARTESIAN_POINT('Ctrl Pts',(13.0660088519392,0.361400197209248,3.66639076405307));
#42205=CARTESIAN_POINT('Ctrl Pts',(13.1137246880021,0.476067254403989,4.1235523942958));
#42206=CARTESIAN_POINT('Ctrl Pts',(13.1505886227152,0.226902767145371,4.38908671404106));
#42207=CARTESIAN_POINT('Ctrl Pts',(13.1715472787407,0.0444343739838573,
4.41587777975472));
#42208=CARTESIAN_POINT('Ctrl Pts',(13.1766006560786,0.000342007958933428,
4.41553758638117));
#42209=CARTESIAN_POINT('Ctrl Pts',(12.9733993439214,0.000150764780949724,
4.4164954541449));
#42210=CARTESIAN_POINT('Ctrl Pts',(12.988350764987,-0.12953330947047,4.41589144324702));
#42211=CARTESIAN_POINT('Ctrl Pts',(13.0192074647402,-0.39825874617628,4.28096832590395));
#42212=CARTESIAN_POINT('Ctrl Pts',(13.065969443181,-0.458911634846768,3.82306685936703));
#42213=CARTESIAN_POINT('Ctrl Pts',(13.1136852792439,-0.0993761143989603,
3.51830547777773));
#42214=CARTESIAN_POINT('Ctrl Pts',(13.1614011153067,0.351418020999476,3.65589158776806));
#42215=CARTESIAN_POINT('Ctrl Pts',(13.2091169513695,0.479499580452807,4.10947774749948));
#42216=CARTESIAN_POINT('Ctrl Pts',(13.2464496942411,0.235195791588524,4.38570395495548));
#42217=CARTESIAN_POINT('Ctrl Pts',(13.2678771584251,0.0485170676377186,
4.41576563003508));
#42218=CARTESIAN_POINT('Ctrl Pts',(13.2733993439214,0.000305371599794949,
4.41543889539504));
#42219=CARTESIAN_POINT('Origin',(3.42660065607856,0.,4.));
#42220=CARTESIAN_POINT('',(12.5766006560786,-0.000382134531266273,4.41577416496379));
#42221=CARTESIAN_POINT('',(12.6733993439214,-0.000382453243898073,4.41589767499446));
#42222=CARTESIAN_POINT('',(3.42660065607856,4.87367679877478E-13,4.415875));
#42223=CARTESIAN_POINT('Ctrl Pts',(12.5766006560786,-0.000382134531266193,
4.41577416496379));
#42224=CARTESIAN_POINT('Ctrl Pts',(12.5806839344893,-0.0359587315295452,
4.41609477791077));
#42225=CARTESIAN_POINT('Ctrl Pts',(12.6006724915877,-0.209750441210566,
4.39561070447123));
#42226=CARTESIAN_POINT('Ctrl Pts',(12.6365663273737,-0.4676569254097,4.15232276575852));
#42227=CARTESIAN_POINT('Ctrl Pts',(12.6842821634365,-0.381050985679211,
3.68902512775968));
#42228=CARTESIAN_POINT('Ctrl Pts',(12.7319979994994,0.0554799374235607,
3.5113004999026));
#42229=CARTESIAN_POINT('Ctrl Pts',(12.7797138355622,0.441062780321708,3.78235614259331));
#42230=CARTESIAN_POINT('Ctrl Pts',(12.8274296716251,0.421610885427219,4.2532774884218));
#42231=CARTESIAN_POINT('Ctrl Pts',(12.8597252784638,0.146394963767536,4.4145887178469));
#42232=CARTESIAN_POINT('Ctrl Pts',(12.876115606615,0.00428438860018927,
4.4165543301878));
#42233=CARTESIAN_POINT('Ctrl Pts',(12.8766006560786,7.85109994958138E-5,
4.41654344863055));
#42234=CARTESIAN_POINT('Ctrl Pts',(12.6733993439214,-0.000382453243898042,
4.41589767499447));
#42235=CARTESIAN_POINT('Ctrl Pts',(12.6770138141737,-0.0318505807336982,
4.4161892599907));
#42236=CARTESIAN_POINT('Ctrl Pts',(12.6965335631136,-0.201468625965512,
4.39853963407534));
#42237=CARTESIAN_POINT('Ctrl Pts',(12.7319585907412,-0.462967872677167,
4.16603003860975));
#42238=CARTESIAN_POINT('Ctrl Pts',(12.779674426804,-0.390044463885,3.70038267566003));
#42239=CARTESIAN_POINT('Ctrl Pts',(12.8273902628668,0.0410627776982723,
3.50987851185683));
#42240=CARTESIAN_POINT('Ctrl Pts',(12.8751060989297,0.434461438689172,3.76946045210395));
#42241=CARTESIAN_POINT('Ctrl Pts',(12.9228219349925,0.42888747548329,4.24075040649094));
#42242=CARTESIAN_POINT('Ctrl Pts',(12.9555863499897,0.154617472482897,4.41255553662561));
#42243=CARTESIAN_POINT('Ctrl Pts',(12.9724454862994,0.00842423538524961,
4.41653398830136));
#42244=CARTESIAN_POINT('Ctrl Pts',(12.9733993439214,0.000150764780949724,
4.4164954541449));
#42245=CARTESIAN_POINT('Origin',(3.42660065607856,0.,4.));
#42246=CARTESIAN_POINT('',(12.2766006560786,9.99581421417901E-5,4.41520820259509));
#42247=CARTESIAN_POINT('',(12.3733993439214,3.32456539758885E-5,4.41518865831861));
#42248=CARTESIAN_POINT('',(3.42660065607856,4.87367679877478E-13,4.415875));
#42249=CARTESIAN_POINT('Ctrl Pts',(12.2766006560786,9.99581421418094E-5,
4.41520820259509));
#42250=CARTESIAN_POINT('Ctrl Pts',(12.2852522623637,-0.0755384113923865,
4.41504611816934));
#42251=CARTESIAN_POINT('Ctrl Pts',(12.3098091473364,-0.290455378639464,
4.35903266527152));
#42252=CARTESIAN_POINT('Ctrl Pts',(12.3502713109967,-0.49164800158875,4.0136918729824));
#42253=CARTESIAN_POINT('Ctrl Pts',(12.3979871470595,-0.277420602272412,
3.59386820576715));
#42254=CARTESIAN_POINT('Ctrl Pts',(12.4457029831224,0.191566404775332,3.54700161433684));
#42255=CARTESIAN_POINT('Ctrl Pts',(12.4934188191852,0.484635034689867,3.91613041073711));
#42256=CARTESIAN_POINT('Ctrl Pts',(12.5370513768373,0.345661459897227,4.32409890635003));
#42257=CARTESIAN_POINT('Ctrl Pts',(12.5647786558017,0.102620036091023,4.41484591908716));
#42258=CARTESIAN_POINT('Ctrl Pts',(12.5766006560786,-0.000382134531266193,
4.41577416496379));
#42259=CARTESIAN_POINT('Ctrl Pts',(12.3733993439214,3.32456539758746E-5,
4.41518865831861));
#42260=CARTESIAN_POINT('Ctrl Pts',(12.381582142048,-0.071514873974996,4.41513780400291));
#42261=CARTESIAN_POINT('Ctrl Pts',(12.4056702188623,-0.282203129244181,
4.36350051499509));
#42262=CARTESIAN_POINT('Ctrl Pts',(12.4456635743641,-0.491031474462283,
4.0281658647901));
#42263=CARTESIAN_POINT('Ctrl Pts',(12.493379410427,-0.289261580343189,3.60221492864948));
#42264=CARTESIAN_POINT('Ctrl Pts',(12.5410952464898,0.178141673866572,3.54155614424011));
#42265=CARTESIAN_POINT('Ctrl Pts',(12.5888110825527,0.481954687902679,3.90189340664049));
#42266=CARTESIAN_POINT('Ctrl Pts',(12.6329124483632,0.353693368040787,4.31820342736526));
#42267=CARTESIAN_POINT('Ctrl Pts',(12.6611085354861,0.106623193447456,4.41490615616012));
#42268=CARTESIAN_POINT('Ctrl Pts',(12.6733993439214,-0.000382453243898042,
4.41589767499447));
#42269=CARTESIAN_POINT('Origin',(3.42660065607856,0.,4.));
#42270=CARTESIAN_POINT('',(11.9766006560786,0.000344603143201134,4.41614202049347));
#42271=CARTESIAN_POINT('',(12.0733993439214,0.00037008249145147,4.41602009379307));
#42272=CARTESIAN_POINT('',(3.42660065607856,4.87367679877478E-13,4.415875));
#42273=CARTESIAN_POINT('Ctrl Pts',(11.9766006560786,0.000344603143201134,
4.41614202049347));
#42274=CARTESIAN_POINT('Ctrl Pts',(11.989820590238,-0.114576335025177,4.41511745277426));
#42275=CARTESIAN_POINT('Ctrl Pts',(12.018945803085,-0.369470719226983,4.30593844396252));
#42276=CARTESIAN_POINT('Ctrl Pts',(12.0639762946196,-0.475409571231627,
3.87394063131468));
#42277=CARTESIAN_POINT('Ctrl Pts',(12.1116921306825,-0.151090047408964,
3.53194335553704));
#42278=CARTESIAN_POINT('Ctrl Pts',(12.1594079667453,0.311977791768556,3.61976969834691));
#42279=CARTESIAN_POINT('Ctrl Pts',(12.2071238028081,0.488551624369653,4.05676737776005));
#42280=CARTESIAN_POINT('Ctrl Pts',(12.2461880325859,0.265811525316043,4.37185240566124));
#42281=CARTESIAN_POINT('Ctrl Pts',(12.269346983676,0.0635166157645696,4.41534409728183));
#42282=CARTESIAN_POINT('Ctrl Pts',(12.2766006560786,9.99581421418094E-5,
4.41520820259509));
#42283=CARTESIAN_POINT('Ctrl Pts',(12.0733993439214,0.000370082491451453,
4.41602009379308));
#42284=CARTESIAN_POINT('Ctrl Pts',(12.0861504699224,-0.110559366248508,
4.41499479059613));
#42285=CARTESIAN_POINT('Ctrl Pts',(12.1148068746109,-0.361534897467509,
4.3122242613332));
#42286=CARTESIAN_POINT('Ctrl Pts',(12.1593685579871,-0.478916017555994,
3.88799699566402));
#42287=CARTESIAN_POINT('Ctrl Pts',(12.2070843940499,-0.164809627468288,
3.53659627586117));
#42288=CARTESIAN_POINT('Ctrl Pts',(12.2548002301128,0.300643979445627,3.61074632631782));
#42289=CARTESIAN_POINT('Ctrl Pts',(12.3025160661756,0.490011594032383,4.04235401475446));
#42290=CARTESIAN_POINT('Ctrl Pts',(12.3420491041118,0.274087380788525,4.36772087084377));
#42291=CARTESIAN_POINT('Ctrl Pts',(12.3656768633604,0.0675564760281007,
4.41523665186048));
#42292=CARTESIAN_POINT('Ctrl Pts',(12.3733993439214,3.32456539758746E-5,
4.41518865831861));
#42293=CARTESIAN_POINT('Origin',(3.42660065607856,0.,4.));
#42294=CARTESIAN_POINT('',(11.6766006560786,-0.000272404999166542,4.41633191892761));
#42295=CARTESIAN_POINT('',(11.7733993439214,-0.000215373091504267,4.41642415578018));
#42296=CARTESIAN_POINT('',(3.42660065607856,4.87367679877478E-13,4.415875));
#42297=CARTESIAN_POINT('Ctrl Pts',(11.6766006560786,-0.000272404999166455,
4.41633191892761));
#42298=CARTESIAN_POINT('Ctrl Pts',(11.6784836394247,-0.0166217551361539,
4.41645573239506));
#42299=CARTESIAN_POINT('Ctrl Pts',(11.6962719014584,-0.170944672110958,
4.40814899119985));
#42300=CARTESIAN_POINT('Ctrl Pts',(11.7299654421798,-0.44220355512924,4.21531660568344));
#42301=CARTESIAN_POINT('Ctrl Pts',(11.7776812782426,-0.420270357404582,
3.74450430230823));
#42302=CARTESIAN_POINT('Ctrl Pts',(11.8253971143054,-0.0123964237846327,
3.50831762943));
#42303=CARTESIAN_POINT('Ctrl Pts',(11.8731129503683,0.406861336540243,3.72365044295193));
#42304=CARTESIAN_POINT('Ctrl Pts',(11.9208287864311,0.452492071153857,4.1927593068956));
#42305=CARTESIAN_POINT('Ctrl Pts',(11.9553246883346,0.185075114683736,4.40392780377));
#42306=CARTESIAN_POINT('Ctrl Pts',(11.9739153115504,0.0236883133891,4.41635013933017));
#42307=CARTESIAN_POINT('Ctrl Pts',(11.9766006560786,0.000344603143201134,
4.41614202049347));
#42308=CARTESIAN_POINT('Ctrl Pts',(11.7733993439214,-0.000215373091504231,
4.41642415578018));
#42309=CARTESIAN_POINT('Ctrl Pts',(11.7748135191091,-0.0124870613922979,
4.41650138834433));
#42310=CARTESIAN_POINT('Ctrl Pts',(11.7921329729843,-0.162701432614141,
4.41043584391465));
#42311=CARTESIAN_POINT('Ctrl Pts',(11.8253577055472,-0.435670260442099,
4.22824690363353));
#42312=CARTESIAN_POINT('Ctrl Pts',(11.8730735416101,-0.427612859293677,
3.75699286549843));
#42313=CARTESIAN_POINT('Ctrl Pts',(11.9207893776729,-0.0268719897862959,
3.50889601812151));
#42314=CARTESIAN_POINT('Ctrl Pts',(11.9685052137357,0.398545841420554,3.71178751390968));
#42315=CARTESIAN_POINT('Ctrl Pts',(12.0162210497986,0.457972894034889,4.17934897039372));
#42316=CARTESIAN_POINT('Ctrl Pts',(12.0511857598605,0.193343073938706,4.40127740506484));
#42317=CARTESIAN_POINT('Ctrl Pts',(12.0702451912347,0.0278098881012828,
4.41627371553856));
#42318=CARTESIAN_POINT('Ctrl Pts',(12.0733993439214,0.000370082491451453,
4.41602009379308));
#42319=CARTESIAN_POINT('Origin',(3.42660065607856,0.,4.));
#42320=CARTESIAN_POINT('',(11.3766006560786,-0.000206048103233091,4.41528588740701));
#42321=CARTESIAN_POINT('',(11.4733993439214,-0.000260100423148973,4.41535533657191));
#42322=CARTESIAN_POINT('',(3.42660065607856,4.87367679877478E-13,4.415875));
#42323=CARTESIAN_POINT('Ctrl Pts',(11.3766006560786,-0.000206048103232999,
4.41528588740701));
#42324=CARTESIAN_POINT('Ctrl Pts',(11.383051967299,-0.0565815589273492,
4.41553770218085));
#42325=CARTESIAN_POINT('Ctrl Pts',(11.4054085572071,-0.251630532720247,
4.37854193442951));
#42326=CARTESIAN_POINT('Ctrl Pts',(11.4436704258028,-0.485070265991237,
4.08131458604192));
#42327=CARTESIAN_POINT('Ctrl Pts',(11.4913862618656,-0.330742172127369,
3.63597412121053));
#42328=CARTESIAN_POINT('Ctrl Pts',(11.5391020979284,0.127311547523522,3.52492422212962));
#42329=CARTESIAN_POINT('Ctrl Pts',(11.5868179339912,0.468453114143607,3.85014371984754));
#42330=CARTESIAN_POINT('Ctrl Pts',(11.632650786708,0.382920955827079,4.29471395365306));
#42331=CARTESIAN_POINT('Ctrl Pts',(11.6625783607371,0.121478760105588,4.41540989855421));
#42332=CARTESIAN_POINT('Ctrl Pts',(11.6766006560786,-0.000272404999166455,
4.41633191892761));
#42333=CARTESIAN_POINT('Ctrl Pts',(11.4733993439214,-0.000260100423148869,
4.41535533657191));
#42334=CARTESIAN_POINT('Ctrl Pts',(11.4793818469834,-0.0525169974224216,
4.41565306322741));
#42335=CARTESIAN_POINT('Ctrl Pts',(11.501269628733,-0.243338890257842,4.3822327073369));
#42336=CARTESIAN_POINT('Ctrl Pts',(11.5390626891702,-0.482464979911041,
4.09556551685319));
#42337=CARTESIAN_POINT('Ctrl Pts',(11.586778525233,-0.341319923258817,3.64587299617429));
#42338=CARTESIAN_POINT('Ctrl Pts',(11.6344943612959,0.113264470804062,3.5213807520529));
#42339=CARTESIAN_POINT('Ctrl Pts',(11.6822101973587,0.463836358529674,3.83641192782507));
#42340=CARTESIAN_POINT('Ctrl Pts',(11.7285118582339,0.390694138047139,4.28787953265104));
#42341=CARTESIAN_POINT('Ctrl Pts',(11.7589082404215,0.125533053862222,4.41563275094549));
#42342=CARTESIAN_POINT('Ctrl Pts',(11.7733993439214,-0.000215373091504231,
4.41642415578018));
#42343=CARTESIAN_POINT('Origin',(3.42660065607856,0.,4.));
#42344=CARTESIAN_POINT('',(11.0766006560786,0.000352537510456688,4.41557576695298));
#42345=CARTESIAN_POINT('',(11.1733993439214,0.000319650745578964,4.41547275084625));
#42346=CARTESIAN_POINT('',(3.42660065607856,4.87367679877478E-13,4.415875));
#42347=CARTESIAN_POINT('Ctrl Pts',(11.0766006560786,0.000352537510456667,
4.41557576695298));
#42348=CARTESIAN_POINT('Ctrl Pts',(11.0876202951733,-0.0957751134661499,
4.41480617263661));
#42349=CARTESIAN_POINT('Ctrl Pts',(11.1145452129557,-0.331820540820521,
4.33374203885914));
#42350=CARTESIAN_POINT('Ctrl Pts',(11.1573754094257,-0.488245699001722,
3.94065893278431));
#42351=CARTESIAN_POINT('Ctrl Pts',(11.2050912454886,-0.214150733603143,
3.55723066033293));
#42352=CARTESIAN_POINT('Ctrl Pts',(11.2528070815514,0.256602145595791,3.58040428537983));
#42353=CARTESIAN_POINT('Ctrl Pts',(11.3005229176142,0.491713326162588,3.98889911147238));
#42354=CARTESIAN_POINT('Ctrl Pts',(11.3417874424566,0.304539430122629,4.35098016691413));
#42355=CARTESIAN_POINT('Ctrl Pts',(11.3671466886114,0.0824085130402235,
4.41491686960609));
#42356=CARTESIAN_POINT('Ctrl Pts',(11.3766006560786,-0.000206048103232999,
4.41528588740701));
#42357=CARTESIAN_POINT('Ctrl Pts',(11.1733993439214,0.000319650745578978,
4.41547275084625));
#42358=CARTESIAN_POINT('Ctrl Pts',(11.1839501748577,-0.0917759901056567,
4.4148158243975));
#42359=CARTESIAN_POINT('Ctrl Pts',(11.2104062844816,-0.32368545017211,4.33911969104981));
#42360=CARTESIAN_POINT('Ctrl Pts',(11.2527676727932,-0.489781601228288,
3.95506440219344));
#42361=CARTESIAN_POINT('Ctrl Pts',(11.300483508856,-0.227098200695192,3.56372986339542));
#42362=CARTESIAN_POINT('Ctrl Pts',(11.3481993449188,0.244132971891272,3.57302890392028));
#42363=CARTESIAN_POINT('Ctrl Pts',(11.3959151809817,0.491173079921361,3.97442207176994));
#42364=CARTESIAN_POINT('Ctrl Pts',(11.4376485139825,0.312739912806573,4.34603313379779));
#42365=CARTESIAN_POINT('Ctrl Pts',(11.4634765682958,0.0864149014017155,
4.41486151738456));
#42366=CARTESIAN_POINT('Ctrl Pts',(11.4733993439214,-0.000260100423148869,
4.41535533657191));
#42367=CARTESIAN_POINT('Origin',(3.42660065607856,0.,4.));
#42368=CARTESIAN_POINT('',(10.7766006560786,5.16128798610187E-5,4.41655360457584));
#42369=CARTESIAN_POINT('',(10.8733993439214,0.000125523266313186,4.41651574507477));
#42370=CARTESIAN_POINT('',(3.42660065607856,4.87367679877478E-13,4.415875));
#42371=CARTESIAN_POINT('Ctrl Pts',(10.7766006560786,5.16128798610299E-5,
4.41655360457584));
#42372=CARTESIAN_POINT('Ctrl Pts',(10.7921886230477,-0.135103241057852,
4.41631783152902));
#42373=CARTESIAN_POINT('Ctrl Pts',(10.8236818687044,-0.408598944994929,
4.27108057505162));
#42374=CARTESIAN_POINT('Ctrl Pts',(10.8710803930487,-0.451470021714238,
3.80485891169382));
#42375=CARTESIAN_POINT('Ctrl Pts',(10.9187962291115,-0.080036233235122,
3.51471716883706));
#42376=CARTESIAN_POINT('Ctrl Pts',(10.9665120651743,0.364896059739551,3.6702181168734));
#42377=CARTESIAN_POINT('Ctrl Pts',(11.0142279012372,0.47473868640782,4.1285628425314));
#42378=CARTESIAN_POINT('Ctrl Pts',(11.0509240982053,0.223935965514619,4.3902602363912));
#42379=CARTESIAN_POINT('Ctrl Pts',(11.0717150164857,0.0429714521173939,
4.4159169723618));
#42380=CARTESIAN_POINT('Ctrl Pts',(11.0766006560786,0.000352537510456667,
4.41557576695298));
#42381=CARTESIAN_POINT('Ctrl Pts',(10.8733993439214,0.000125523266313226,
4.41651574507477));
#42382=CARTESIAN_POINT('Ctrl Pts',(10.888518502732,-0.130996444363694,4.41599591363288));
#42383=CARTESIAN_POINT('Ctrl Pts',(10.9195429402303,-0.400997532511054,
4.27840016053723));
#42384=CARTESIAN_POINT('Ctrl Pts',(10.9664726564161,-0.45702143577077,3.81824018018824));
#42385=CARTESIAN_POINT('Ctrl Pts',(11.014188492479,-0.0942939790271268,
3.51728489730359));
#42386=CARTESIAN_POINT('Ctrl Pts',(11.0619043285418,0.355025089556487,3.65961432075161));
#42387=CARTESIAN_POINT('Ctrl Pts',(11.1096201646047,0.478319155637209,4.11452515096033));
#42388=CARTESIAN_POINT('Ctrl Pts',(11.1467851697312,0.23222845252417,4.38693182090163));
#42389=CARTESIAN_POINT('Ctrl Pts',(11.1680448961701,0.0470573247768451,
4.41580613485813));
#42390=CARTESIAN_POINT('Ctrl Pts',(11.1733993439214,0.000319650745578978,
4.41547275084625));
#42391=CARTESIAN_POINT('Origin',(3.42660065607856,0.,4.));
#42392=CARTESIAN_POINT('',(10.4766006560786,-0.000378910032885682,4.4157309619862));
#42393=CARTESIAN_POINT('',(10.5733993439214,-0.000383826598418624,4.41585315377736));
#42394=CARTESIAN_POINT('',(3.42660065607856,4.87367679877478E-13,4.415875));
#42395=CARTESIAN_POINT('Ctrl Pts',(10.4766006560786,-0.000378910032885704,
4.4157309619862));
#42396=CARTESIAN_POINT('Ctrl Pts',(10.4808516722344,-0.0374267536145521,
4.41605913507464));
#42397=CARTESIAN_POINT('Ctrl Pts',(10.5010079670778,-0.212714974368116,
4.3945277200383));
#42398=CARTESIAN_POINT('Ctrl Pts',(10.5370695406088,-0.469236294399976,
4.14738563318641));
#42399=CARTESIAN_POINT('Ctrl Pts',(10.5847853766716,-0.377752434501872,
3.68502647241413));
#42400=CARTESIAN_POINT('Ctrl Pts',(10.6325012127345,0.0606272984676223,
3.51191234851464));
#42401=CARTESIAN_POINT('Ctrl Pts',(10.6802170487973,0.443332050383407,3.78701662516801));
#42402=CARTESIAN_POINT('Ctrl Pts',(10.7279328848602,0.418918158891686,4.25770681210006));
#42403=CARTESIAN_POINT('Ctrl Pts',(10.7600607539539,0.143455624352724,4.41528584951654));
#42404=CARTESIAN_POINT('Ctrl Pts',(10.7762833443601,0.00280285164340033,
4.41655840401831));
#42405=CARTESIAN_POINT('Ctrl Pts',(10.7766006560786,5.16128798610299E-5,
4.41655360457584));
#42406=CARTESIAN_POINT('Ctrl Pts',(10.5733993439214,-0.000383826598418617,
4.41585315377736));
#42407=CARTESIAN_POINT('Ctrl Pts',(10.5771815519187,-0.0333213161677604,
4.41615637378185));
#42408=CARTESIAN_POINT('Ctrl Pts',(10.5968690386037,-0.20443114816448,4.39750812937281));
#42409=CARTESIAN_POINT('Ctrl Pts',(10.6324618039763,-0.464691964107356,
4.16114156306187));
#42410=CARTESIAN_POINT('Ctrl Pts',(10.6801776400391,-0.386865111317189,
3.69628860657276));
#42411=CARTESIAN_POINT('Ctrl Pts',(10.7278934761019,0.0462259258804368,
3.51033849586834));
#42412=CARTESIAN_POINT('Ctrl Pts',(10.7756093121648,0.436866984064762,3.77405207881873));
#42413=CARTESIAN_POINT('Ctrl Pts',(10.8233251482276,0.426326368719826,4.24525711444552));
#42414=CARTESIAN_POINT('Ctrl Pts',(10.8559218254798,0.151674250044741,4.4132974389186));
#42415=CARTESIAN_POINT('Ctrl Pts',(10.8726132240444,0.00694320316194716,
4.41654277368359));
#42416=CARTESIAN_POINT('Ctrl Pts',(10.8733993439214,0.000125523266313226,
4.41651574507477));
#42417=CARTESIAN_POINT('Origin',(3.42660065607856,0.,4.));
#42418=CARTESIAN_POINT('',(10.1766006560786,0.000123197149224082,4.41521991402453));
#42419=CARTESIAN_POINT('',(10.2733993439214,5.7336166378985E-5,4.41519339896199));
#42420=CARTESIAN_POINT('',(3.42660065607856,4.87367679877478E-13,4.415875));
#42421=CARTESIAN_POINT('Ctrl Pts',(10.1766006560786,0.000123197149224097,
4.41521991402453));
#42422=CARTESIAN_POINT('Ctrl Pts',(10.1854200001087,-0.0769762270984491,
4.41501595190525));
#42423=CARTESIAN_POINT('Ctrl Pts',(10.2101446228264,-0.293404201931947,
4.35739193013711));
#42424=CARTESIAN_POINT('Ctrl Pts',(10.2507745242318,-0.491764996345908,
4.00850959581219));
#42425=CARTESIAN_POINT('Ctrl Pts',(10.2984903602946,-0.273124940234581,
3.59096700393021));
#42426=CARTESIAN_POINT('Ctrl Pts',(10.3462061963575,0.196329951061554,3.54904570612073));
#42427=CARTESIAN_POINT('Ctrl Pts',(10.3939220324203,0.485492027373267,3.92124267520431));
#42428=CARTESIAN_POINT('Ctrl Pts',(10.4373868523273,0.34277731801193,4.32616121393696));
#42429=CARTESIAN_POINT('Ctrl Pts',(10.4649463935468,0.101188639822117,4.41483126760997));
#42430=CARTESIAN_POINT('Ctrl Pts',(10.4766006560786,-0.000378910032885704,
4.4157309619862));
#42431=CARTESIAN_POINT('Ctrl Pts',(10.2733993439214,5.73361663789851E-5,
4.41519339896199));
#42432=CARTESIAN_POINT('Ctrl Pts',(10.2817498797931,-0.0729553575157724,
4.41510384014646));
#42433=CARTESIAN_POINT('Ctrl Pts',(10.3060056943524,-0.285157432566911,
4.36192175935665));
#42434=CARTESIAN_POINT('Ctrl Pts',(10.3461667875993,-0.491301045992024,
4.02298928139638));
#42435=CARTESIAN_POINT('Ctrl Pts',(10.3938826236621,-0.285053227451061,
3.599188470261));
#42436=CARTESIAN_POINT('Ctrl Pts',(10.4415984597249,0.182963355965895,3.54345905416307));
#42437=CARTESIAN_POINT('Ctrl Pts',(10.4893142957878,0.482961874346273,3.9069782134126));
#42438=CARTESIAN_POINT('Ctrl Pts',(10.5332479238533,0.35082465130295,4.32033516829581));
#42439=CARTESIAN_POINT('Ctrl Pts',(10.5612762732311,0.105190355120073,4.41488124595214));
#42440=CARTESIAN_POINT('Ctrl Pts',(10.5733993439214,-0.000383826598418617,
4.41585315377736));
#42441=CARTESIAN_POINT('Origin',(3.42660065607856,0.,4.));
#42442=CARTESIAN_POINT('',(9.87660065607859,0.000332404019580576,4.41618417038907));
#42443=CARTESIAN_POINT('',(9.9733993439214,0.000362444897862246,4.41606425076498));
#42444=CARTESIAN_POINT('',(3.42660065607856,4.87367679877478E-13,4.415875));
#42445=CARTESIAN_POINT('Ctrl Pts',(9.87660065607859,0.000332404019580564,
4.41618417038907));
#42446=CARTESIAN_POINT('Ctrl Pts',(9.88998832798303,-0.116016130490024,
4.41516972706101));
#42447=CARTESIAN_POINT('Ctrl Pts',(9.91928127857509,-0.372296869871387,
4.30364082544554));
#42448=CARTESIAN_POINT('Ctrl Pts',(9.96447950785476,-0.474054618562381,
3.8689372536849));
#42449=CARTESIAN_POINT('Ctrl Pts',(10.0121953439176,-0.146148770628728,
3.53037700046135));
#42450=CARTESIAN_POINT('Ctrl Pts',(10.0599111799804,0.315967742161179,3.62307877379278));
#42451=CARTESIAN_POINT('Ctrl Pts',(10.1076270160433,0.487926215535836,4.06191310882887));
#42452=CARTESIAN_POINT('Ctrl Pts',(10.146523508076,0.262848409674369,4.37329037489646));
#42453=CARTESIAN_POINT('Ctrl Pts',(10.1695147214211,0.062069015396409,4.41538378814543));
#42454=CARTESIAN_POINT('Ctrl Pts',(10.1766006560786,0.000123197149224097,
4.41521991402453));
#42455=CARTESIAN_POINT('Ctrl Pts',(9.9733993439214,0.000362444897862267,
4.41606425076498));
#42456=CARTESIAN_POINT('Ctrl Pts',(9.9863182076674,-0.111995531308361,4.41503480155798));
#42457=CARTESIAN_POINT('Ctrl Pts',(10.015142350101,-0.364380386131072,4.30999810797653));
#42458=CARTESIAN_POINT('Ctrl Pts',(10.0598717712222,-0.477709011270712,
3.88295588266498));
#42459=CARTESIAN_POINT('Ctrl Pts',(10.1075876072851,-0.159916626226494,
3.53488507064564));
#42460=CARTESIAN_POINT('Ctrl Pts',(10.1553034433479,0.304729657315094,3.61393645496551));
#42461=CARTESIAN_POINT('Ctrl Pts',(10.2030192794107,0.489538007675758,4.04751593304174));
#42462=CARTESIAN_POINT('Ctrl Pts',(10.2423845796019,0.271127379494919,4.3692182851415));
#42463=CARTESIAN_POINT('Ctrl Pts',(10.2658446011055,0.0661120339180705,
4.41527442296197));
#42464=CARTESIAN_POINT('Ctrl Pts',(10.2733993439214,5.73361663789851E-5,
4.41519339896199));
#42465=CARTESIAN_POINT('Origin',(3.42660065607856,0.,4.));
#42466=CARTESIAN_POINT('',(9.57660065607859,-0.000290304052950346,4.41629504206998));
#42467=CARTESIAN_POINT('',(9.6733993439214,-0.000236899196693507,4.41639317328699));
#42468=CARTESIAN_POINT('',(3.42660065607856,4.87367679877478E-13,4.415875));
#42469=CARTESIAN_POINT('Ctrl Pts',(9.57660065607859,-0.000290304052950335,
4.41629504206998));
#42470=CARTESIAN_POINT('Ctrl Pts',(9.57865137716975,-0.0181001948149981,
4.41643644713422));
#42471=CARTESIAN_POINT('Ctrl Pts',(9.59660737694851,-0.173896467062472,
4.40729888742394));
#42472=CARTESIAN_POINT('Ctrl Pts',(9.63046865541489,-0.444448234747017,
4.21064422964382));
#42473=CARTESIAN_POINT('Ctrl Pts',(9.67818449147773,-0.41755432743774,3.74008922975375));
#42474=CARTESIAN_POINT('Ctrl Pts',(9.72590032754057,-0.00721385634321597,
3.50821428942208));
#42475=CARTESIAN_POINT('Ctrl Pts',(9.77361616360341,0.40975121003073,3.72795373420991));
#42476=CARTESIAN_POINT('Ctrl Pts',(9.82133199966624,0.450435435400681,4.19751745084266));
#42477=CARTESIAN_POINT('Ctrl Pts',(9.85566016382464,0.182118884769847,4.40484283743537));
#42478=CARTESIAN_POINT('Ctrl Pts',(9.87408304929542,0.0222122246324328,
4.41637494063069));
#42479=CARTESIAN_POINT('Ctrl Pts',(9.87660065607859,0.000332404019580564,
4.41618417038907));
#42480=CARTESIAN_POINT('Ctrl Pts',(9.6733993439214,-0.00023689919669354,
4.41639317328699));
#42481=CARTESIAN_POINT('Ctrl Pts',(9.67498125685411,-0.0139668454918635,
4.4164864708936));
#42482=CARTESIAN_POINT('Ctrl Pts',(9.69246844847443,-0.165649677201134,
4.40963259460397));
#42483=CARTESIAN_POINT('Ctrl Pts',(9.72586091878235,-0.438051576325333,
4.22364266437974));
#42484=CARTESIAN_POINT('Ctrl Pts',(9.77357675484519,-0.425028039486299,
3.75249971615691));
#42485=CARTESIAN_POINT('Ctrl Pts',(9.82129259090803,-0.0216947140899849,
3.50864008686857));
#42486=CARTESIAN_POINT('Ctrl Pts',(9.86900842697087,0.401561201071248,3.7160038263529));
#42487=CARTESIAN_POINT('Ctrl Pts',(9.91672426303371,0.456057286475463,4.18416562194019));
#42488=CARTESIAN_POINT('Ctrl Pts',(9.95152123535055,0.190383912560376,4.40224154849284));
#42489=CARTESIAN_POINT('Ctrl Pts',(9.97041292897978,0.0263359008882403,
4.4163022254471));
#42490=CARTESIAN_POINT('Ctrl Pts',(9.9733993439214,0.000362444897862267,
4.41606425076498));
#42491=CARTESIAN_POINT('Origin',(3.42660065607856,0.,4.));
#42492=CARTESIAN_POINT('',(9.27660065607858,-0.000185084181660103,4.41526520375254));
#42493=CARTESIAN_POINT('',(9.37339934392141,-0.000241596553487405,4.41532857883968));
#42494=CARTESIAN_POINT('',(3.42660065607856,4.87367679877478E-13,4.415875));
#42495=CARTESIAN_POINT('Ctrl Pts',(9.27660065607858,-0.000185084181660189,
4.41526520375254));
#42496=CARTESIAN_POINT('Ctrl Pts',(9.28321970504406,-0.0580335922681754,
4.4154966095816));
#42497=CARTESIAN_POINT('Ctrl Pts',(9.30574403269715,-0.254596444523232,
4.37718269734299));
#42498=CARTESIAN_POINT('Ctrl Pts',(9.34417363903789,-0.485900307124067,
4.07619787653679));
#42499=CARTESIAN_POINT('Ctrl Pts',(9.39188947510068,-0.326887306273347,
3.63250862071426));
#42500=CARTESIAN_POINT('Ctrl Pts',(9.43960531116356,0.13231133773591,3.52629235307153));
#42501=CARTESIAN_POINT('Ctrl Pts',(9.48732114722637,0.470006444430667,3.85508910653225));
#42502=CARTESIAN_POINT('Ctrl Pts',(9.53298626219807,0.380123833963086,4.29710958399465));
#42503=CARTESIAN_POINT('Ctrl Pts',(9.56274609848214,0.120032327051623,4.41533971732329));
#42504=CARTESIAN_POINT('Ctrl Pts',(9.57660065607859,-0.000290304052950335,
4.41629504206998));
#42505=CARTESIAN_POINT('Ctrl Pts',(9.3733993439214,-0.000241596553487357,
4.41532857883968));
#42506=CARTESIAN_POINT('Ctrl Pts',(9.37954958472843,-0.0539723465869793,
4.41561177485228));
#42507=CARTESIAN_POINT('Ctrl Pts',(9.40160510422307,-0.246305905820531,
4.3809303471886));
#42508=CARTESIAN_POINT('Ctrl Pts',(9.43956590240532,-0.483445357410111,
4.09047547319903));
#42509=CARTESIAN_POINT('Ctrl Pts',(9.48728173846818,-0.337568794959357,
3.64229546617122));
#42510=CARTESIAN_POINT('Ctrl Pts',(9.53499757453099,0.118302386066128,3.5226010365501));
#42511=CARTESIAN_POINT('Ctrl Pts',(9.58271341059386,0.465534665650901,3.84130942079228));
#42512=CARTESIAN_POINT('Ctrl Pts',(9.62884733372396,0.387920650713885,4.29034844530944));
#42513=CARTESIAN_POINT('Ctrl Pts',(9.65907597816649,0.124080336294106,4.41554841393524));
#42514=CARTESIAN_POINT('Ctrl Pts',(9.6733993439214,-0.00023689919669354,
4.41639317328699));
#42515=CARTESIAN_POINT('Origin',(3.42660065607856,0.,4.));
#42516=CARTESIAN_POINT('',(8.97660065607858,0.000361621133123973,4.41561526113518));
#42517=CARTESIAN_POINT('',(9.0733993439214,0.00033264130393823,4.41550825894961));
#42518=CARTESIAN_POINT('',(3.42660065607856,4.87367679877478E-13,4.415875));
#42519=CARTESIAN_POINT('Ctrl Pts',(8.97660065607858,0.000361621133123963,
4.41561526113518));
#42520=CARTESIAN_POINT('Ctrl Pts',(8.98778803291839,-0.097205817696177,
4.41480833810253));
#42521=CARTESIAN_POINT('Ctrl Pts',(9.01488068844582,-0.334723089553266,
4.33177224018802));
#42522=CARTESIAN_POINT('Ctrl Pts',(9.05787862266083,-0.487593182843731,
3.93551656882348));
#42523=CARTESIAN_POINT('Ctrl Pts',(9.10559445872368,-0.209472459465777,
3.55499829935456));
#42524=CARTESIAN_POINT('Ctrl Pts',(9.15331029478651,0.261010046587687,3.58313193881964));
#42525=CARTESIAN_POINT('Ctrl Pts',(9.20102613084934,0.491803010703882,3.99408193320625));
#42526=CARTESIAN_POINT('Ctrl Pts',(9.24212291794672,0.301599829163518,4.35270650246492));
#42527=CARTESIAN_POINT('Ctrl Pts',(9.26731442635645,0.0809737859182142,
4.41494055172187));
#42528=CARTESIAN_POINT('Ctrl Pts',(9.27660065607858,-0.000185084181660189,
4.41526520375254));
#42529=CARTESIAN_POINT('Ctrl Pts',(9.0733993439214,0.000332641303938268,
4.41550825894961));
#42530=CARTESIAN_POINT('Ctrl Pts',(9.08411791260276,-0.093207009794584,
4.4148098083896));
#42531=CARTESIAN_POINT('Ctrl Pts',(9.11074175997173,-0.326599857706223,
4.33721709571948));
#42532=CARTESIAN_POINT('Ctrl Pts',(9.1532708860283,-0.489280820139143,3.94990505119329));
#42533=CARTESIAN_POINT('Ctrl Pts',(9.20098672209113,-0.222487703095825,
3.56136068709803));
#42534=CARTESIAN_POINT('Ctrl Pts',(9.24870255815399,0.248619295113741,3.57562555337399));
#42535=CARTESIAN_POINT('Ctrl Pts',(9.29641839421681,0.49141536912078,3.97960000382683));
#42536=CARTESIAN_POINT('Ctrl Pts',(9.33798398947263,0.309808547095179,4.34782394055348));
#42537=CARTESIAN_POINT('Ctrl Pts',(9.36364430604082,0.0849819773478622,
4.41487939515448));
#42538=CARTESIAN_POINT('Ctrl Pts',(9.3733993439214,-0.000241596553487357,
4.41532857883968));
#42539=CARTESIAN_POINT('Origin',(3.42660065607856,0.,4.));
#42540=CARTESIAN_POINT('',(8.67660065607859,2.43999233753954E-5,4.41655967853978));
#42541=CARTESIAN_POINT('',(8.77339934392141,9.9565801791445E-5,4.41653262406943));
#42542=CARTESIAN_POINT('',(3.42660065607856,4.87367679877478E-13,4.415875));
#42543=CARTESIAN_POINT('Ctrl Pts',(8.67660065607859,2.43999233753836E-5,
4.41655967853978));
#42544=CARTESIAN_POINT('Ctrl Pts',(8.69235636079272,-0.136579453435425,
4.41644398151286));
#42545=CARTESIAN_POINT('Ctrl Pts',(8.72401734419445,-0.411298873006737,
4.26841067400337));
#42546=CARTESIAN_POINT('Ctrl Pts',(8.7715836062838,-0.449388340942622,3.80011167148426));
#42547=CARTESIAN_POINT('Ctrl Pts',(8.81929944234665,-0.0749173544856965,
3.51390061216986));
#42548=CARTESIAN_POINT('Ctrl Pts',(8.86701527840948,0.368351391347115,3.67408210030036));
#42549=CARTESIAN_POINT('Ctrl Pts',(8.91473111447233,0.473357386691186,4.13355901061654));
#42550=CARTESIAN_POINT('Ctrl Pts',(8.95125957369535,0.220969504140389,4.39141457480799));
#42551=CARTESIAN_POINT('Ctrl Pts',(8.97188275423077,0.0415074238114615,
4.41595555392421));
#42552=CARTESIAN_POINT('Ctrl Pts',(8.97660065607858,0.000361621133123963,
4.41561526113518));
#42553=CARTESIAN_POINT('Ctrl Pts',(8.77339934392141,9.95658017914599E-5,
4.41653262406943));
#42554=CARTESIAN_POINT('Ctrl Pts',(8.78868624047708,-0.132462770989084,
4.416105976883));
#42555=CARTESIAN_POINT('Ctrl Pts',(8.81987841572037,-0.403726445587972,
4.27580529254432));
#42556=CARTESIAN_POINT('Ctrl Pts',(8.86697586965126,-0.455080472922433,
3.81343369002772));
#42557=CARTESIAN_POINT('Ctrl Pts',(8.91469170571412,-0.0892013699275644,
3.51631793453238));
#42558=CARTESIAN_POINT('Ctrl Pts',(8.96240754177693,0.358592723611288,3.66337486216116));
#42559=CARTESIAN_POINT('Ctrl Pts',(9.0101233778398,0.477085601399612,4.11955983351088));
#42560=CARTESIAN_POINT('Ctrl Pts',(9.04712064522126,0.229261233371815,4.38814011953822));
#42561=CARTESIAN_POINT('Ctrl Pts',(9.06821263391514,0.0455964315317218,
4.41584623882512));
#42562=CARTESIAN_POINT('Ctrl Pts',(9.0733993439214,0.000332641303938268,
4.41550825894961));
#42563=CARTESIAN_POINT('Origin',(3.42660065607856,0.,4.));
#42564=CARTESIAN_POINT('',(8.37660065607859,-0.000374086211409503,4.41568853448753));
#42565=CARTESIAN_POINT('',(8.47339934392141,-0.000383538171196851,4.41580895574666));
#42566=CARTESIAN_POINT('',(3.42660065607856,4.87367679877478E-13,4.415875));
#42567=CARTESIAN_POINT('Ctrl Pts',(8.37660065607859,-0.000374086211409545,
4.41568853448753));
#42568=CARTESIAN_POINT('Ctrl Pts',(8.38101940997943,-0.0388937529272332,
4.41602262289185));
#42569=CARTESIAN_POINT('Ctrl Pts',(8.40134344256788,-0.215680110827853,
4.3934260635833));
#42570=CARTESIAN_POINT('Ctrl Pts',(8.43757275384394,-0.470763542849379,
4.14243212971755));
#42571=CARTESIAN_POINT('Ctrl Pts',(8.48528858990678,-0.37441192437669,3.68106280283335));
#42572=CARTESIAN_POINT('Ctrl Pts',(8.53300442596962,0.0657679253190804,
3.51257841158684));
#42573=CARTESIAN_POINT('Ctrl Pts',(8.58072026203246,0.445552077224736,3.79170076492532));
#42574=CARTESIAN_POINT('Ctrl Pts',(8.62843609809529,0.41617890091499,4.26210751092856));
#42575=CARTESIAN_POINT('Ctrl Pts',(8.66039622944401,0.140517691799823,4.41596716726027));
#42576=CARTESIAN_POINT('Ctrl Pts',(8.6764510821051,0.00132122424898086,
4.41656077688887));
#42577=CARTESIAN_POINT('Ctrl Pts',(8.67660065607859,2.43999233753836E-5,
4.41655967853978));
#42578=CARTESIAN_POINT('Ctrl Pts',(8.47339934392141,-0.000383538171196768,
4.41580895574666));
#42579=CARTESIAN_POINT('Ctrl Pts',(8.47734928966379,-0.0347911067166248,
4.41612244784963));
#42580=CARTESIAN_POINT('Ctrl Pts',(8.4972045140938,-0.207394442561863,4.39645832432586));
#42581=CARTESIAN_POINT('Ctrl Pts',(8.5329650172114,-0.466364439759318,4.15623518867385));
#42582=CARTESIAN_POINT('Ctrl Pts',(8.58068085327425,-0.383642787608637,
3.69222827230584));
#42583=CARTESIAN_POINT('Ctrl Pts',(8.62839668933707,0.0513839395061145,
3.51085286915611));
#42584=CARTESIAN_POINT('Ctrl Pts',(8.67611252539993,0.439224004328866,3.77866880275638));
#42585=CARTESIAN_POINT('Ctrl Pts',(8.72382836146275,0.42371790764641,4.24973658040369));
#42586=CARTESIAN_POINT('Ctrl Pts',(8.75625730096992,0.148732406864234,4.41402322426773));
#42587=CARTESIAN_POINT('Ctrl Pts',(8.77278096178947,0.00546194790078228,
4.41654988270631));
#42588=CARTESIAN_POINT('Ctrl Pts',(8.77339934392141,9.95658017914599E-5,
4.41653262406943));
#42589=CARTESIAN_POINT('Origin',(3.42660065607856,0.,4.));
#42590=CARTESIAN_POINT('',(8.07660065607859,0.000145957947245773,4.41523406184916));
#42591=CARTESIAN_POINT('',(8.1733993439214,8.12049300508987E-5,4.41520065480005));
#42592=CARTESIAN_POINT('',(3.42660065607856,4.87367679877478E-13,4.415875));
#42593=CARTESIAN_POINT('Ctrl Pts',(8.07660065607858,0.00014595794724577,
4.41523406184916));
#42594=CARTESIAN_POINT('Ctrl Pts',(8.08558773785375,-0.0784131624224431,
4.41498734772332));
#42595=CARTESIAN_POINT('Ctrl Pts',(8.11048009831652,-0.296350794919178,
4.35572875890285));
#42596=CARTESIAN_POINT('Ctrl Pts',(8.15127773746691,-0.491827368180951,
4.00332637343646));
#42597=CARTESIAN_POINT('Ctrl Pts',(8.19899357352975,-0.268798940774433,
3.58811123553743));
#42598=CARTESIAN_POINT('Ctrl Pts',(8.24670940959259,0.201071689948468,3.55113988776764));
#42599=CARTESIAN_POINT('Ctrl Pts',(8.29442524565542,0.486295093906121,3.92636368766143));
#42600=CARTESIAN_POINT('Ctrl Pts',(8.33772232781743,0.339888039743562,4.32819890206972));
#42601=CARTESIAN_POINT('Ctrl Pts',(8.36511413129181,0.0997575609540166,
4.41482007364463));
#42602=CARTESIAN_POINT('Ctrl Pts',(8.37660065607859,-0.000374086211409545,
4.41568853448753));
#42603=CARTESIAN_POINT('Ctrl Pts',(8.1733993439214,8.12049300509751E-5,
4.41520065480005));
#42604=CARTESIAN_POINT('Ctrl Pts',(8.18191761753811,-0.0743948540356096,
4.41507113968239));
#42605=CARTESIAN_POINT('Ctrl Pts',(8.20634116984244,-0.288109900049694,
4.36032095112539));
#42606=CARTESIAN_POINT('Ctrl Pts',(8.24667000083438,-0.491516046133,4.01781014446235));
#42607=CARTESIAN_POINT('Ctrl Pts',(8.29438583689722,-0.280813212199106,
3.59620653211525));
#42608=CARTESIAN_POINT('Ctrl Pts',(8.34210167296004,0.187764715363875,3.54541267448783));
#42609=CARTESIAN_POINT('Ctrl Pts',(8.38981750902289,0.483915415676709,3.91207335260334));
#42610=CARTESIAN_POINT('Ctrl Pts',(8.43358339934334,0.347950231939931,4.32244196179047));
#42611=CARTESIAN_POINT('Ctrl Pts',(8.46144401097618,0.1037581297464,4.41486010664565));
#42612=CARTESIAN_POINT('Ctrl Pts',(8.47339934392141,-0.000383538171196768,
4.41580895574666));
#42613=CARTESIAN_POINT('Origin',(3.42660065607856,0.,4.));
#42614=CARTESIAN_POINT('',(7.77660065607858,0.000318631424802313,4.41622521972442));
#42615=CARTESIAN_POINT('',(7.8733993439214,0.000353153796088606,4.4161078667978));
#42616=CARTESIAN_POINT('',(3.42660065607856,4.87367679877478E-13,4.415875));
#42617=CARTESIAN_POINT('Ctrl Pts',(7.77660065607859,0.000318631424802297,
4.41622521972442));
#42618=CARTESIAN_POINT('Ctrl Pts',(7.79015606572807,-0.117457481003694,
4.41522659035305));
#42619=CARTESIAN_POINT('Ctrl Pts',(7.81961675406517,-0.375115671948731,
4.30131743988157));
#42620=CARTESIAN_POINT('Ctrl Pts',(7.86498272108989,-0.472647010158531,
3.86394843388276));
#42621=CARTESIAN_POINT('Ctrl Pts',(7.91269855715272,-0.141191260335066,
3.52886280888004));
#42622=CARTESIAN_POINT('Ctrl Pts',(7.96041439321556,0.31992259635559,3.62642971585976));
#42623=CARTESIAN_POINT('Ctrl Pts',(8.0081302292784,0.48724661017382,4.0670519628834));
#42624=CARTESIAN_POINT('Ctrl Pts',(8.04685898356608,0.259884401562094,4.37470733986759));
#42625=CARTESIAN_POINT('Ctrl Pts',(8.06968245916614,0.0606202562326388,
4.41542398077349));
#42626=CARTESIAN_POINT('Ctrl Pts',(8.07660065607858,0.00014595794724577,
4.41523406184916));
#42627=CARTESIAN_POINT('Ctrl Pts',(7.8733993439214,0.000353153796088627,
4.4161078667978));
#42628=CARTESIAN_POINT('Ctrl Pts',(7.88648594541244,-0.113432877329791,
4.41507910421771));
#42629=CARTESIAN_POINT('Ctrl Pts',(7.9154778255911,-0.367219156371593,4.30774647947464));
#42630=CARTESIAN_POINT('Ctrl Pts',(7.96037498445733,-0.476448943335793,
3.87792777037096));
#42631=CARTESIAN_POINT('Ctrl Pts',(8.0080908205202,-0.1550058622045,3.53322552818936));
#42632=CARTESIAN_POINT('Ctrl Pts',(8.05580665658301,0.308781487260178,3.61716946571973));
#42633=CARTESIAN_POINT('Ctrl Pts',(8.10352249264587,0.489010045760349,4.0526725734847));
#42634=CARTESIAN_POINT('Ctrl Pts',(8.14272005509199,0.26816615642074,4.37069430501912));
#42635=CARTESIAN_POINT('Ctrl Pts',(8.1660123388505,0.064666477720629,4.4153129696744));
#42636=CARTESIAN_POINT('Ctrl Pts',(8.1733993439214,8.12049300509751E-5,
4.41520065480005));
#42637=CARTESIAN_POINT('Origin',(3.42660065607856,0.,4.));
#42638=CARTESIAN_POINT('',(7.47660065607859,-0.000306770237538029,4.41625647512786));
#42639=CARTESIAN_POINT('',(7.5733993439214,-0.000257198714157858,4.41635988094829));
#42640=CARTESIAN_POINT('',(3.42660065607856,4.87367679877478E-13,4.415875));
#42641=CARTESIAN_POINT('Ctrl Pts',(7.47660065607859,-0.00030677023753798,
4.41625647512786));
#42642=CARTESIAN_POINT('Ctrl Pts',(7.47881911491479,-0.0195780710793754,
4.41641565502598));
#42643=CARTESIAN_POINT('Ctrl Pts',(7.4969428524386,-0.176849480241104,4.4064317922735));
#42644=CARTESIAN_POINT('Ctrl Pts',(7.53097186865002,-0.44664354691983,4.20594845626764));
#42645=CARTESIAN_POINT('Ctrl Pts',(7.57868770471286,-0.414791917646955,
3.73570302684109));
#42646=CARTESIAN_POINT('Ctrl Pts',(7.62640354077569,-0.00203048755240202,
3.50816557464413));
#42647=CARTESIAN_POINT('Ctrl Pts',(7.67411937683853,0.412595570264971,3.73228724307244));
#42648=CARTESIAN_POINT('Ctrl Pts',(7.72183521290137,0.448328767436039,4.20225365549051));
#42649=CARTESIAN_POINT('Ctrl Pts',(7.75599563931472,0.179163779268806,4.40574053813273));
#42650=CARTESIAN_POINT('Ctrl Pts',(7.77425078704046,0.0207354574140521,
4.41639833498254));
#42651=CARTESIAN_POINT('Ctrl Pts',(7.77660065607859,0.000318631424802297,
4.41622521972442));
#42652=CARTESIAN_POINT('Ctrl Pts',(7.5733993439214,-0.000257198714157839,
4.41635988094829));
#42653=CARTESIAN_POINT('Ctrl Pts',(7.57514899459915,-0.0154461882200338,
4.41646996636401));
#42654=CARTESIAN_POINT('Ctrl Pts',(7.59280392396451,-0.168599214901356,
4.40881268721627));
#42655=CARTESIAN_POINT('Ctrl Pts',(7.62636413201748,-0.440384235482588,
4.21901358396786));
#42656=CARTESIAN_POINT('Ctrl Pts',(7.67407996808031,-0.422396009600076,
3.7480340579683));
#42657=CARTESIAN_POINT('Ctrl Pts',(7.72179580414317,-0.0165150286377962,
3.50843873354525));
#42658=CARTESIAN_POINT('Ctrl Pts',(7.76951164020598,0.404531957204003,3.72025168374225));
#42659=CARTESIAN_POINT('Ctrl Pts',(7.81722747626884,0.454091022239626,4.18896181724392));
#42660=CARTESIAN_POINT('Ctrl Pts',(7.85185671084063,0.187425762196077,4.40318800700955));
#42661=CARTESIAN_POINT('Ctrl Pts',(7.87058066672482,0.02486112795907,4.41632944836175));
#42662=CARTESIAN_POINT('Ctrl Pts',(7.8733993439214,0.000353153796088627,
4.4161078667978));
#42663=CARTESIAN_POINT('Origin',(3.42660065607856,0.,4.));
#42664=CARTESIAN_POINT('',(7.17660065607858,-0.000163391746992416,4.4152468210878));
#42665=CARTESIAN_POINT('',(7.2733993439214,-0.000222139526412562,4.4153039283715));
#42666=CARTESIAN_POINT('',(3.42660065607856,4.87367679877478E-13,4.415875));
#42667=CARTESIAN_POINT('Ctrl Pts',(7.17660065607859,-0.000163391746992363,
4.4152468210878));
#42668=CARTESIAN_POINT('Ctrl Pts',(7.18338744278911,-0.0594844418834033,
4.41545575762517));
#42669=CARTESIAN_POINT('Ctrl Pts',(7.20607950818724,-0.257561782965025,
4.37580284351512));
#42670=CARTESIAN_POINT('Ctrl Pts',(7.24467685227299,-0.486676365692783,
4.07107270446015));
#42671=CARTESIAN_POINT('Ctrl Pts',(7.29239268833582,-0.322996137187983,
3.62908393881966));
#42672=CARTESIAN_POINT('Ctrl Pts',(7.34010852439867,0.137296434535941,3.52771310152703));
#42673=CARTESIAN_POINT('Ctrl Pts',(7.3878243604615,0.471507566988788,3.86005058906394));
#42674=CARTESIAN_POINT('Ctrl Pts',(7.43332173768814,0.377318713751663,4.29947917201381));
#42675=CARTESIAN_POINT('Ctrl Pts',(7.46291383622717,0.118587850938607,4.41527441201542));
#42676=CARTESIAN_POINT('Ctrl Pts',(7.47660065607859,-0.00030677023753798,
4.41625647512786));
#42677=CARTESIAN_POINT('Ctrl Pts',(7.2733993439214,-0.000222139526412493,
4.4153039283715));
#42678=CARTESIAN_POINT('Ctrl Pts',(7.27971732247348,-0.0554265094472961,
4.41557047734173));
#42679=CARTESIAN_POINT('Ctrl Pts',(7.30194057971316,-0.249272617462211,
4.37960776139715));
#42680=CARTESIAN_POINT('Ctrl Pts',(7.34006911564044,-0.484372034479295,
4.08537538031203));
#42681=CARTESIAN_POINT('Ctrl Pts',(7.3877849517033,-0.333780171974684,3.63875766810317));
#42682=CARTESIAN_POINT('Ctrl Pts',(7.43550078776612,0.123327161313159,3.52387434835784));
#42683=CARTESIAN_POINT('Ctrl Pts',(7.48321662382897,0.467181263150904,3.84622454030349));
#42684=CARTESIAN_POINT('Ctrl Pts',(7.52918280921405,0.385138488472668,4.29279105563264));
#42685=CARTESIAN_POINT('Ctrl Pts',(7.55924371591154,0.122630008444172,4.41546922990911));
#42686=CARTESIAN_POINT('Ctrl Pts',(7.5733993439214,-0.000257198714157839,
4.41635988094829));
#42687=CARTESIAN_POINT('Origin',(3.42660065607856,0.,4.));
#42688=CARTESIAN_POINT('',(6.87660065607859,0.000369753976522709,4.4156559906262));
#42689=CARTESIAN_POINT('',(6.9733993439214,0.000344359613660638,4.41554532105972));
#42690=CARTESIAN_POINT('',(3.42660065607856,4.87367679877478E-13,4.415875));
#42691=CARTESIAN_POINT('Ctrl Pts',(6.87660065607859,0.000369753976522759,
4.4156559906262));
#42692=CARTESIAN_POINT('Ctrl Pts',(6.88795577066343,-0.0986361616094132,
4.41481368816743));
#42693=CARTESIAN_POINT('Ctrl Pts',(6.91521616393589,-0.337621850525623,
4.32977807754403));
#42694=CARTESIAN_POINT('Ctrl Pts',(6.95838183589596,-0.486886005735063,
3.93038141845316));
#42695=CARTESIAN_POINT('Ctrl Pts',(7.0060976719588,-0.204771183672361,3.55281534000283));
#42696=CARTESIAN_POINT('Ctrl Pts',(7.05381350802163,0.265389096458903,3.58590591031157));
#42697=CARTESIAN_POINT('Ctrl Pts',(7.10152934408448,0.491837993618785,3.99926540470374));
#42698=CARTESIAN_POINT('Ctrl Pts',(7.14245839343679,0.298657604039877,4.35441002681052));
#42699=CARTESIAN_POINT('Ctrl Pts',(7.16748216410149,0.0795383202432945,
4.41496610118));
#42700=CARTESIAN_POINT('Ctrl Pts',(7.17660065607859,-0.000163391746992363,
4.4152468210878));
#42701=CARTESIAN_POINT('Ctrl Pts',(6.9733993439214,0.00034435961366068,
4.41554532105972));
#42702=CARTESIAN_POINT('Ctrl Pts',(6.9842856503478,-0.0946377878655052,
4.41480662962373));
#42703=CARTESIAN_POINT('Ctrl Pts',(7.0110772354618,-0.329510302625179,4.33529054280597));
#42704=CARTESIAN_POINT('Ctrl Pts',(7.05377409926342,-0.488725618924084,
3.94475128051735));
#42705=CARTESIAN_POINT('Ctrl Pts',(7.10148993532626,-0.21785253135038,3.55904022429238));
#42706=CARTESIAN_POINT('Ctrl Pts',(7.14920577138909,0.253078023397415,3.57826934481931));
#42707=CARTESIAN_POINT('Ctrl Pts',(7.19692160745195,0.491603063369337,3.98478019943955));
#42708=CARTESIAN_POINT('Ctrl Pts',(7.2383194649627,0.306874094293292,4.34959156107453));
#42709=CARTESIAN_POINT('Ctrl Pts',(7.26381204378586,0.0835484619188193,
4.41489945011039));
#42710=CARTESIAN_POINT('Ctrl Pts',(7.2733993439214,-0.000222139526412493,
4.4153039283715));
#42711=CARTESIAN_POINT('Origin',(3.42660065607856,0.,4.));
#42712=CARTESIAN_POINT('',(6.57660065607858,1.8302248101926E-5,4.41656360501758));
#42713=CARTESIAN_POINT('',(6.6733993439214,7.63499956435865E-5,4.4165465803965));
#42714=CARTESIAN_POINT('',(3.42660065607856,4.87367679877478E-13,4.415875));
#42715=CARTESIAN_POINT('Ctrl Pts',(6.57660065607858,1.83022481018748E-5,
4.41656360501758));
#42716=CARTESIAN_POINT('Ctrl Pts',(6.57661881985014,-0.000139156870309867,
4.41656362372179));
#42717=CARTESIAN_POINT('Ctrl Pts',(6.59254226230931,-0.138177237712184,
4.41649399470799));
#42718=CARTESIAN_POINT('Ctrl Pts',(6.62437098345609,-0.41404349770976,4.26553045144514));
#42719=CARTESIAN_POINT('Ctrl Pts',(6.67208681951894,-0.447234019333667,
3.79538894860702));
#42720=CARTESIAN_POINT('Ctrl Pts',(6.71980265558177,-0.0698021891909718,
3.51313682319347));
#42721=CARTESIAN_POINT('Ctrl Pts',(6.76751849164461,0.371772181936036,3.67798293440124));
#42722=CARTESIAN_POINT('Ctrl Pts',(6.81523432770745,0.471920133146607,4.13853999974893));
#42723=CARTESIAN_POINT('Ctrl Pts',(6.85159504918544,0.21800401543618,4.39254992240466));
#42724=CARTESIAN_POINT('Ctrl Pts',(6.87205049197582,0.0400429038769189,
4.41599351380864));
#42725=CARTESIAN_POINT('Ctrl Pts',(6.87660065607859,0.000369753976522759,
4.4156559906262));
#42726=CARTESIAN_POINT('Ctrl Pts',(6.6733993439214,7.63499956435956E-5,
4.4165465803965));
#42727=CARTESIAN_POINT('Ctrl Pts',(6.68885397822212,-0.133927014866661,
4.41622291450327));
#42728=CARTESIAN_POINT('Ctrl Pts',(6.72021389121046,-0.406451392834186,
4.27318229388465));
#42729=CARTESIAN_POINT('Ctrl Pts',(6.76747908288639,-0.453085647428837,
3.80864864857145));
#42730=CARTESIAN_POINT('Ctrl Pts',(6.81519491894923,-0.0841006081168706,
3.51540431248109));
#42731=CARTESIAN_POINT('Ctrl Pts',(6.86291075501207,0.362121456530253,3.66717299786736));
#42732=CARTESIAN_POINT('Ctrl Pts',(6.91062659107491,0.475798562415156,4.124581128109));
#42733=CARTESIAN_POINT('Ctrl Pts',(6.94745612071136,0.226294304474162,4.38932900794447));
#42734=CARTESIAN_POINT('Ctrl Pts',(6.96838037166019,0.0441344886838037,
4.41588588393584));
#42735=CARTESIAN_POINT('Ctrl Pts',(6.9733993439214,0.00034435961366068,
4.41554532105972));
#42736=CARTESIAN_POINT('Origin',(3.42660065607856,0.,4.));
#42737=CARTESIAN_POINT('',(6.27660065607859,-8.94903747701068E-6,4.41582842213685));
#42738=CARTESIAN_POINT('',(6.3733993439214,-0.000441664590319634,4.4157663968931));
#42739=CARTESIAN_POINT('',(3.42660065607856,4.87367679877478E-13,4.415875));
#42740=CARTESIAN_POINT('Ctrl Pts',(6.27660065607859,-8.94903747701223E-6,
4.41582842213685));
#42741=CARTESIAN_POINT('Ctrl Pts',(6.28118714772447,-0.0399801639742102,
4.41579747358059));
#42742=CARTESIAN_POINT('Ctrl Pts',(6.29372627871415,-0.149263049162913,
4.40013952362907));
#42743=CARTESIAN_POINT('Ctrl Pts',(6.31421804904765,-0.307151379675736,
4.3060270879454));
#42744=CARTESIAN_POINT('Ctrl Pts',(6.33807596707907,-0.416657206472865,
4.12081787696614));
#42745=CARTESIAN_POINT('Ctrl Pts',(6.36193388511048,-0.422829889105799,
3.9075587958503));
#42746=CARTESIAN_POINT('Ctrl Pts',(6.39374444248571,-0.296437506874183,
3.64987069373525));
#42747=CARTESIAN_POINT('Ctrl Pts',(6.43350763920474,0.0703302468340302,
3.51324810367198));
#42748=CARTESIAN_POINT('Ctrl Pts',(6.48122347526758,0.448014600657906,3.7964368525222));
#42749=CARTESIAN_POINT('Ctrl Pts',(6.52892114755886,0.413253290380966,4.26628466471864));
#42750=CARTESIAN_POINT('Ctrl Pts',(6.56071354116253,0.137741412285014,4.41654724519979));
#42751=CARTESIAN_POINT('Ctrl Pts',(6.57660065607858,1.83022481018748E-5,
4.41656360501758));
#42752=CARTESIAN_POINT('Ctrl Pts',(6.3733993439214,-0.000441664590319611,
4.4157663968931));
#42753=CARTESIAN_POINT('Ctrl Pts',(6.37751702740883,-0.0362476131304844,
4.41610293027605));
#42754=CARTESIAN_POINT('Ctrl Pts',(6.39753998958387,-0.210006484715375,
4.39546152579387));
#42755=CARTESIAN_POINT('Ctrl Pts',(6.43346823044653,-0.468271923807345,
4.15124960425567));
#42756=CARTESIAN_POINT('Ctrl Pts',(6.48118406650937,-0.380227249479543,
3.6882349865083));
#42757=CARTESIAN_POINT('Ctrl Pts',(6.52889990257221,0.0564566449812287,
3.51140415777354));
#42758=CARTESIAN_POINT('Ctrl Pts',(6.57661573863504,0.441574375138847,3.78331933667001));
#42759=CARTESIAN_POINT('Ctrl Pts',(6.62433157469789,0.421040068198854,4.25418342072721));
#42760=CARTESIAN_POINT('Ctrl Pts',(6.65659277646,0.145792717270209,4.41473316952435));
#42761=CARTESIAN_POINT('Ctrl Pts',(6.6729486995345,0.00398377756883227,
4.41655601822694));
#42762=CARTESIAN_POINT('Ctrl Pts',(6.6733993439214,7.63499956435956E-5,
4.4165465803965));
#42763=CARTESIAN_POINT('Origin',(3.42660065607856,0.,4.));
#42764=CARTESIAN_POINT('',(5.97660065607859,-9.19412645702589E-6,4.41589218083175));
#42765=CARTESIAN_POINT('',(6.0733993439214,-6.65563173402051E-6,4.41590255337155));
#42766=CARTESIAN_POINT('',(3.42660065607856,4.87367679877478E-13,4.415875));
#42767=CARTESIAN_POINT('Ctrl Pts',(5.97660065607858,-9.19412645705893E-6,
4.41589218083175));
#42768=CARTESIAN_POINT('Ctrl Pts',(5.97780283625498,-0.0104787976275591,
4.4159022685469));
#42769=CARTESIAN_POINT('Ctrl Pts',(5.98695765577519,-0.0902010538040918,
4.41295272969856));
#42770=CARTESIAN_POINT('Ctrl Pts',(6.0040651146392,-0.23587461323539,4.36380751861078));
#42771=CARTESIAN_POINT('Ctrl Pts',(6.02792303267061,-0.381351759249696,
4.20630938167977));
#42772=CARTESIAN_POINT('Ctrl Pts',(6.05178095070204,-0.433578399193506,
3.9983625870902));
#42773=CARTESIAN_POINT('Ctrl Pts',(6.07563886873346,-0.379782579589031,
3.79081692866841));
#42774=CARTESIAN_POINT('Ctrl Pts',(6.09949678676487,-0.233120953551068,
3.63442082419035));
#42775=CARTESIAN_POINT('Ctrl Pts',(6.12335470479629,-0.0294522997972467,
3.5674214393556));
#42776=CARTESIAN_POINT('Ctrl Pts',(6.14721262282771,0.181413325723775,3.60619428643423));
#42777=CARTESIAN_POINT('Ctrl Pts',(6.17107054085913,0.347927737305898,3.74127281623538));
#42778=CARTESIAN_POINT('Ctrl Pts',(6.19492845889055,0.429346806292137,3.93959933010928));
#42779=CARTESIAN_POINT('Ctrl Pts',(6.21878637692197,0.405811992579865,4.15272917617017));
#42780=CARTESIAN_POINT('Ctrl Pts',(6.24264429495339,0.282982581651336,4.32844890303245));
#42781=CARTESIAN_POINT('Ctrl Pts',(6.26191572133893,0.127967070080381,4.40561019629887));
#42782=CARTESIAN_POINT('Ctrl Pts',(6.27323450838066,0.029326984292613,4.415851136102));
#42783=CARTESIAN_POINT('Ctrl Pts',(6.27660065607859,-8.94903747701223E-6,
4.41582842213685));
#42784=CARTESIAN_POINT('Ctrl Pts',(6.0733993439214,-6.65563173397714E-6,
4.41590255337156));
#42785=CARTESIAN_POINT('Ctrl Pts',(6.07413271593935,-0.00639299139291402,
4.41590724351385));
#42786=CARTESIAN_POINT('Ctrl Pts',(6.0828187273011,-0.0820297780542147,
4.41420140028919));
#42787=CARTESIAN_POINT('Ctrl Pts',(6.09945737800665,-0.2250554921608,4.3705991908187));
#42788=CARTESIAN_POINT('Ctrl Pts',(6.12331529603809,-0.375113923638194,
4.21744656883549));
#42789=CARTESIAN_POINT('Ctrl Pts',(6.1471732140695,-0.433431396087355,4.01114207710762));
#42790=CARTESIAN_POINT('Ctrl Pts',(6.17103113210093,-0.385792139046387,
3.80207577201042));
#42791=CARTESIAN_POINT('Ctrl Pts',(6.19488905013233,-0.243761337718234,
3.64147770828707));
#42792=CARTESIAN_POINT('Ctrl Pts',(6.21874696816376,-0.042227823444436,
3.56841523311022));
#42793=CARTESIAN_POINT('Ctrl Pts',(6.24260488619517,0.16982704650124,3.60113783246665));
#42794=CARTESIAN_POINT('Ctrl Pts',(6.2664628042266,0.339985970990829,3.73091992247201));
#42795=CARTESIAN_POINT('Ctrl Pts',(6.29032072225801,0.427700638223926,3.92738904240251));
#42796=CARTESIAN_POINT('Ctrl Pts',(6.31417864028943,0.409561128158778,4.13996490148311));
#42797=CARTESIAN_POINT('Ctrl Pts',(6.34187151417723,0.27471212230801,4.35031587281991));
#42798=CARTESIAN_POINT('Ctrl Pts',(6.36161174872122,0.102059178040878,4.41480301073152));
#42799=CARTESIAN_POINT('Ctrl Pts',(6.3733993439214,-0.000441664590319611,
4.4157663968931));
#42800=CARTESIAN_POINT('Origin',(3.42660065607856,0.,4.));
#42801=CARTESIAN_POINT('',(5.67660065607858,1.06631253201556E-5,4.41586554077139));
#42802=CARTESIAN_POINT('',(5.7733993439214,9.17748676071416E-6,4.4158542849441));
#42803=CARTESIAN_POINT('',(3.42660065607856,4.87367679877478E-13,4.415875));
#42804=CARTESIAN_POINT('Ctrl Pts',(5.67660065607858,1.06631253201268E-5,
4.41586554077139));
#42805=CARTESIAN_POINT('Ctrl Pts',(5.68237116412931,-0.050253077703417,
4.41581669384736));
#42806=CARTESIAN_POINT('Ctrl Pts',(5.69609431152383,-0.169828933264711,
4.3941204493343));
#42807=CARTESIAN_POINT('Ctrl Pts',(5.71777009826218,-0.329222253834466,
4.28214440376531));
#42808=CARTESIAN_POINT('Ctrl Pts',(5.74162801629359,-0.424158110434281,
4.08990358344764));
#42809=CARTESIAN_POINT('Ctrl Pts',(5.76548593432501,-0.415375755386326,
3.8756788878607));
#42810=CARTESIAN_POINT('Ctrl Pts',(5.78934385235642,-0.305022713182347,
3.69185409099321));
#42811=CARTESIAN_POINT('Ctrl Pts',(5.81320177038785,-0.120083309624962,
3.58337936191985));
#42812=CARTESIAN_POINT('Ctrl Pts',(5.83705968841926,0.0942197354074567,
3.57677972866706));
#42813=CARTESIAN_POINT('Ctrl Pts',(5.86091760645069,0.285483486244351,3.673668977605));
#42814=CARTESIAN_POINT('Ctrl Pts',(5.8847755244821,0.406938752801468,3.85035505520226));
#42815=CARTESIAN_POINT('Ctrl Pts',(5.90863344251353,0.428886400972996,4.06363338935351));
#42816=CARTESIAN_POINT('Ctrl Pts',(5.93249136054494,0.345959657594393,4.261351642888));
#42817=CARTESIAN_POINT('Ctrl Pts',(5.95514709839996,0.186877681905787,4.38841966610496));
#42818=CARTESIAN_POINT('Ctrl Pts',(5.96985019691118,0.0587795235055939,
4.41583553648629));
#42819=CARTESIAN_POINT('Ctrl Pts',(5.97660065607858,-9.19412645705893E-6,
4.41589218083175));
#42820=CARTESIAN_POINT('Ctrl Pts',(5.7733993439214,9.17748676073846E-6,
4.4158542849441));
#42821=CARTESIAN_POINT('Ctrl Pts',(5.77870104381367,-0.0461746181927863,
4.41581721944429));
#42822=CARTESIAN_POINT('Ctrl Pts',(5.79195538304975,-0.161664917198308,
4.3966319946429));
#42823=CARTESIAN_POINT('Ctrl Pts',(5.81316236162963,-0.320769768688322,
4.29171820750724));
#42824=CARTESIAN_POINT('Ctrl Pts',(5.83702027966105,-0.421326288178809,
4.10235681181338));
#42825=CARTESIAN_POINT('Ctrl Pts',(5.86087819769247,-0.418857046020503,
3.88796639709818));
#42826=CARTESIAN_POINT('Ctrl Pts',(5.88473611572389,-0.313965860818636,
3.70097123187977));
#42827=CARTESIAN_POINT('Ctrl Pts',(5.90859403375531,-0.132301443679057,
3.58709678011166));
#42828=CARTESIAN_POINT('Ctrl Pts',(5.93245195178673,0.0817142298265842,
3.57418834816524));
#42829=CARTESIAN_POINT('Ctrl Pts',(5.95630986981814,0.275748643515392,3.66540258613358));
#42830=CARTESIAN_POINT('Ctrl Pts',(5.98016778784957,0.402354822815078,3.83843477537114));
#42831=CARTESIAN_POINT('Ctrl Pts',(6.00402570588098,0.430574627524036,4.05097449853386));
#42832=CARTESIAN_POINT('Ctrl Pts',(6.02788362391241,0.353506566116634,4.25104874587108));
#42833=CARTESIAN_POINT('Ctrl Pts',(6.05100816992587,0.195023852357142,4.38547315270063));
#42834=CARTESIAN_POINT('Ctrl Pts',(6.06618007659554,0.06286002589468,4.4158563839102));
#42835=CARTESIAN_POINT('Ctrl Pts',(6.0733993439214,-6.65563173397714E-6,
4.41590255337156));
#42836=CARTESIAN_POINT('Origin',(3.42660065607856,0.,4.));
#42837=CARTESIAN_POINT('',(5.37660065607858,-1.01751121954902E-5,4.41586038335289));
#42838=CARTESIAN_POINT('',(5.4733993439214,-1.09014992595302E-5,4.41587264340464));
#42839=CARTESIAN_POINT('',(3.42660065607856,4.87367679877478E-13,4.415875));
#42840=CARTESIAN_POINT('Ctrl Pts',(5.37660065607859,-1.01751121954468E-5,
4.41586038335289));
#42841=CARTESIAN_POINT('Ctrl Pts',(5.37898685265982,-0.0207957689391596,
4.41587928195339));
#42842=CARTESIAN_POINT('Ctrl Pts',(5.38932568858487,-0.110842971866809,
4.40924760552439));
#42843=CARTESIAN_POINT('Ctrl Pts',(5.40761716385372,-0.26226226804932,4.34526983614494));
#42844=CARTESIAN_POINT('Ctrl Pts',(5.43147508188515,-0.395631058815178,
4.17739453851434));
#42845=CARTESIAN_POINT('Ctrl Pts',(5.45533299991656,-0.432257278927009,
3.96614144408682));
#42846=CARTESIAN_POINT('Ctrl Pts',(5.47919091794798,-0.363184819889405,
3.76316768886851));
#42847=CARTESIAN_POINT('Ctrl Pts',(5.5030488359794,-0.205303779432806,3.61810588490468));
#42848=CARTESIAN_POINT('Ctrl Pts',(5.52690675401082,0.00277962745745752,
3.56642759466814));
#42849=CARTESIAN_POINT('Ctrl Pts',(5.55076467204224,0.210183339719457,3.62076956781107));
#42850=CARTESIAN_POINT('Ctrl Pts',(5.57462259007365,0.36619150013966,3.76784371165257));
#42851=CARTESIAN_POINT('Ctrl Pts',(5.59848050810508,0.432655863921731,3.97168639180759));
#42852=CARTESIAN_POINT('Ctrl Pts',(5.62233842613649,0.393324083661671,4.18245252040861));
#42853=CARTESIAN_POINT('Ctrl Pts',(5.64619634416792,0.257813851021257,4.34860403787086));
#42854=CARTESIAN_POINT('Ctrl Pts',(5.66428375414861,0.107285005985459,4.40994309575933));
#42855=CARTESIAN_POINT('Ctrl Pts',(5.6744185247855,0.0190180158238588,4.41588401235146));
#42856=CARTESIAN_POINT('Ctrl Pts',(5.67660065607858,1.06631253201268E-5,
4.41586554077139));
#42857=CARTESIAN_POINT('Ctrl Pts',(5.4733993439214,-1.0901499259525E-5,
4.41587264340464));
#42858=CARTESIAN_POINT('Ctrl Pts',(5.47531673234419,-0.0167114040746605,
4.41588973972128));
#42859=CARTESIAN_POINT('Ctrl Pts',(5.48518676011079,-0.102669266038577,
4.41080986982701));
#42860=CARTESIAN_POINT('Ctrl Pts',(5.50300942722118,-0.251979671819092,
4.35284416104532));
#42861=CARTESIAN_POINT('Ctrl Pts',(5.52686734525261,-0.390234841353927,
4.18896964197264));
#42862=CARTESIAN_POINT('Ctrl Pts',(5.55072526328402,-0.433066962396004,
3.97888689800548));
#42863=CARTESIAN_POINT('Ctrl Pts',(5.57458318131544,-0.370002414621403,
3.77396688259));
#42864=CARTESIAN_POINT('Ctrl Pts',(5.59844109934686,-0.21646219781534,3.62431812139094));
#42865=CARTESIAN_POINT('Ctrl Pts',(5.62229901737828,-0.00999107731853999,
3.56653381289738));
#42866=CARTESIAN_POINT('Ctrl Pts',(5.64615693540971,0.198923133709572,3.61474379450078));
#42867=CARTESIAN_POINT('Ctrl Pts',(5.67001485344111,0.359195220034686,3.75715941257656));
#42868=CARTESIAN_POINT('Ctrl Pts',(5.69387277147254,0.431634290692432,3.95895616900985));
#42869=CARTESIAN_POINT('Ctrl Pts',(5.71773068950395,0.398527019959163,4.1707892603438));
#42870=CARTESIAN_POINT('Ctrl Pts',(5.74158860753538,0.267969036875697,4.34085972491723));
#42871=CARTESIAN_POINT('Ctrl Pts',(5.76014482567452,0.115458993192439,4.40830959117706));
#42872=CARTESIAN_POINT('Ctrl Pts',(5.77074840446986,0.0231018550196917,
4.41587281831976));
#42873=CARTESIAN_POINT('Ctrl Pts',(5.7733993439214,9.17748676073846E-6,
4.4158542849441));
#42874=CARTESIAN_POINT('Origin',(3.42660065607856,0.,4.));
#42875=CARTESIAN_POINT('',(5.07660065607859,8.10857529294212E-6,4.41589722116852));
#42876=CARTESIAN_POINT('',(5.1733993439214,1.02299162792543E-5,4.4158851107878));
#42877=CARTESIAN_POINT('',(3.42660065607856,4.87367679877478E-13,4.415875));
#42878=CARTESIAN_POINT('Ctrl Pts',(5.07660065607858,8.10857529294148E-6,
4.41589722116852));
#42879=CARTESIAN_POINT('Ctrl Pts',(5.08355518053415,-0.060555656273516,
4.41584370653314));
#42880=CARTESIAN_POINT('Ctrl Pts',(5.09846234433351,-0.190424342306974,
4.38715451669839));
#42881=CARTESIAN_POINT('Ctrl Pts',(5.1213221474767,-0.349282119693095,4.256894448863));
#42882=CARTESIAN_POINT('Ctrl Pts',(5.1451800655081,-0.4296670234643,4.05812921762123));
#42883=CARTESIAN_POINT('Ctrl Pts',(5.16903798353954,-0.404986636103755,
3.84514980926298));
#42884=CARTESIAN_POINT('Ctrl Pts',(5.19289590157095,-0.281275984601366,
3.67003549057442));
#42885=CARTESIAN_POINT('Ctrl Pts',(5.21675381960238,-0.0887856930599551,
3.5756064824932));
#42886=CARTESIAN_POINT('Ctrl Pts',(5.24061173763379,0.125415118908336,3.58495324968971));
#42887=CARTESIAN_POINT('Ctrl Pts',(5.26446965566521,0.308948518064291,3.69579025298356));
#42888=CARTESIAN_POINT('Ctrl Pts',(5.28832757369662,0.416935588964862,3.88101482593007));
#42889=CARTESIAN_POINT('Ctrl Pts',(5.31218549172805,0.422970551266107,4.09533451502773));
#42890=CARTESIAN_POINT('Ctrl Pts',(5.33604340975946,0.325577692296299,4.28634231834109));
#42891=CARTESIAN_POINT('Ctrl Pts',(5.35751513120965,0.166275769440666,4.39523064161658));
#42892=CARTESIAN_POINT('Ctrl Pts',(5.37103421331602,0.0484777907299229,
4.41581629730449));
#42893=CARTESIAN_POINT('Ctrl Pts',(5.37660065607859,-1.01751121954468E-5,
4.41586038335289));
#42894=CARTESIAN_POINT('Ctrl Pts',(5.1733993439214,1.02299162792474E-5,
4.4158851107878));
#42895=CARTESIAN_POINT('Ctrl Pts',(5.17988506021851,-0.0564756498766958,
4.41582730150705));
#42896=CARTESIAN_POINT('Ctrl Pts',(5.19432341585943,-0.182274442988225,
4.39002065289559));
#42897=CARTESIAN_POINT('Ctrl Pts',(5.21671441084416,-0.341564590845109,
4.26707000444592));
#42898=CARTESIAN_POINT('Ctrl Pts',(5.24057232887557,-0.427768622694993,
4.07075847957352));
#42899=CARTESIAN_POINT('Ctrl Pts',(5.264430246907,-0.409371574112622,3.85714457902312));
#42900=CARTESIAN_POINT('Ctrl Pts',(5.2882881649384,-0.290872024601924,3.6784627202051));
#42901=CARTESIAN_POINT('Ctrl Pts',(5.31214608296984,-0.101246341881189,
3.57840548479658));
#42902=CARTESIAN_POINT('Ctrl Pts',(5.33600400100125,0.113136829324483,3.58143959235932));
#42903=CARTESIAN_POINT('Ctrl Pts',(5.35986191903268,0.299854963974951,3.68682312094679));
#42904=CARTESIAN_POINT('Ctrl Pts',(5.38371983706408,0.413250392048343,3.8687869272297));
#42905=CARTESIAN_POINT('Ctrl Pts',(5.40757775509551,0.425594842551202,4.08283590397723));
#42906=CARTESIAN_POINT('Ctrl Pts',(5.43143567312693,0.333869761079625,4.27662924579771));
#42907=CARTESIAN_POINT('Ctrl Pts',(5.45337620273556,0.174437273907163,4.39264091290779));
#42908=CARTESIAN_POINT('Ctrl Pts',(5.46736409300038,0.0525562895569378,
4.41581883033293));
#42909=CARTESIAN_POINT('Ctrl Pts',(5.4733993439214,-1.0901499259525E-5,
4.41587264340464));
#42910=CARTESIAN_POINT('Origin',(3.42660065607856,0.,4.));
#42911=CARTESIAN_POINT('',(4.77660065607858,-3.27394476109793E-6,4.41584059078716));
#42912=CARTESIAN_POINT('',(4.8733993439214,-6.67049670156904E-6,4.4158459349409));
#42913=CARTESIAN_POINT('',(3.42660065607856,4.87367679877478E-13,4.415875));
#42914=CARTESIAN_POINT('Ctrl Pts',(4.77660065607858,-3.27394476113199E-6,
4.41584059078717));
#42915=CARTESIAN_POINT('Ctrl Pts',(4.78017086906467,-0.0311067951354469,
4.4158491206715));
#42916=CARTESIAN_POINT('Ctrl Pts',(4.79169372139456,-0.131487321212171,
4.40473555835468));
#42917=CARTESIAN_POINT('Ctrl Pts',(4.81116921306824,-0.287199161490599,
4.32482210305491));
#42918=CARTESIAN_POINT('Ctrl Pts',(4.83502713109967,-0.407721671464292,
4.14749845969467));
#42919=CARTESIAN_POINT('Ctrl Pts',(4.85888504913109,-0.42854512664958,3.93410742516172));
#42920=CARTESIAN_POINT('Ctrl Pts',(4.8827429671625,-0.344577625034195,3.73682892005441));
#42921=CARTESIAN_POINT('Ctrl Pts',(4.90660088519393,-0.176351507991885,
3.60390291263011));
#42922=CARTESIAN_POINT('Ctrl Pts',(4.93045880322534,0.0349973564730633,
3.56783343253575));
#42923=CARTESIAN_POINT('Ctrl Pts',(4.95431672125677,0.237788413971502,3.63744045016736));
#42924=CARTESIAN_POINT('Ctrl Pts',(4.97817463928818,0.382433727027559,3.79570315365689));
#42925=CARTESIAN_POINT('Ctrl Pts',(5.0020325573196,0.433563576539811,4.00392200101168));
#42926=CARTESIAN_POINT('Ctrl Pts',(5.02589047535102,0.378675321553375,4.21118181228595));
#42927=CARTESIAN_POINT('Ctrl Pts',(5.04974839338244,0.231190635538481,4.36680191797922));
#42928=CARTESIAN_POINT('Ctrl Pts',(5.0666517869583,0.086644022961884,4.4135113916189));
#42929=CARTESIAN_POINT('Ctrl Pts',(5.07560254119034,0.00870023350343714,
4.41590490160082));
#42930=CARTESIAN_POINT('Ctrl Pts',(5.07660065607858,8.10857529294148E-6,
4.41589722116852));
#42931=CARTESIAN_POINT('Ctrl Pts',(4.8733993439214,-6.67049670157252E-6,
4.41584593494091));
#42932=CARTESIAN_POINT('Ctrl Pts',(4.87650074874903,-0.0270249643080214,
4.41586127519519));
#42933=CARTESIAN_POINT('Ctrl Pts',(4.88755479292047,-0.123313358466266,
4.40662010077424));
#42934=CARTESIAN_POINT('Ctrl Pts',(4.90656147643571,-0.277507970732168,
4.33313973520738));
#42935=CARTESIAN_POINT('Ctrl Pts',(4.93041939446713,-0.403200703213916,
4.15944262266324));
#42936=CARTESIAN_POINT('Ctrl Pts',(4.95427731249855,-0.430299880793222,
3.94675744574809));
#42937=CARTESIAN_POINT('Ctrl Pts',(4.97813523052996,-0.352179016385168,
3.7470915236456));
#42938=CARTESIAN_POINT('Ctrl Pts',(5.00199314856139,-0.187940789307144,
3.60926861310034));
#42939=CARTESIAN_POINT('Ctrl Pts',(5.0258510665928,0.0222540801607904,3.56699016996131));
#42940=CARTESIAN_POINT('Ctrl Pts',(5.04970898462423,0.227007220840439,3.63059442521772));
#42941=CARTESIAN_POINT('Ctrl Pts',(5.07356690265564,0.376250912472057,3.7845284059142));
#42942=CARTESIAN_POINT('Ctrl Pts',(5.09742482068706,0.433491007135177,3.99115106069306));
#42943=CARTESIAN_POINT('Ctrl Pts',(5.12128273871848,0.384730742495793,4.19993752217271));
#42944=CARTESIAN_POINT('Ctrl Pts',(5.1451406567499,0.241893331461176,4.35983381329239));
#42945=CARTESIAN_POINT('Ctrl Pts',(5.16251285848421,0.0948160588051851,
4.41219316122439));
#42946=CARTESIAN_POINT('Ctrl Pts',(5.17193242087471,0.0127860645481494,
4.41589818594594));
#42947=CARTESIAN_POINT('Ctrl Pts',(5.1733993439214,1.02299162792474E-5,
4.4158851107878));
#42948=CARTESIAN_POINT('Origin',(3.42660065607856,0.,4.));
#42949=CARTESIAN_POINT('',(4.47660065607858,-1.72413508574122E-6,4.41591032029986));
#42950=CARTESIAN_POINT('',(4.5733993439214,2.6062779713001E-6,4.4159095790646));
#42951=CARTESIAN_POINT('',(3.42660065607856,4.87367679877478E-13,4.415875));
#42952=CARTESIAN_POINT('Ctrl Pts',(4.47660065607858,-1.72413508575881E-6,
4.41591032029986));
#42953=CARTESIAN_POINT('Ctrl Pts',(4.47678655759518,-0.00162050728124812,
4.41591069657345));
#42954=CARTESIAN_POINT('Ctrl Pts',(4.48492509845559,-0.0724886630755744,
4.4155056303295));
#42955=CARTESIAN_POINT('Ctrl Pts',(4.5010162786598,-0.212178818846594,4.37811758201071));
#42956=CARTESIAN_POINT('Ctrl Pts',(4.52487419669122,-0.367409789343613,
4.23022337776645));
#42957=CARTESIAN_POINT('Ctrl Pts',(4.54873211472264,-0.432799058467291,
4.02603328640456));
#42958=CARTESIAN_POINT('Ctrl Pts',(4.57259003275406,-0.392357168499796,
3.8154773474345));
#42959=CARTESIAN_POINT('Ctrl Pts',(4.59644795078547,-0.255973263285106,
3.65004222328625));
#42960=CARTESIAN_POINT('Ctrl Pts',(4.6203058688169,-0.0569969226013119,
3.57018130821703));
#42961=CARTESIAN_POINT('Ctrl Pts',(4.64416378684831,0.155916718210686,3.59542277130738));
#42962=CARTESIAN_POINT('Ctrl Pts',(4.66802170487973,0.330704474340828,3.71959438727947));
#42963=CARTESIAN_POINT('Ctrl Pts',(4.69187962291115,0.424625978282027,3.91233281365517));
#42964=CARTESIAN_POINT('Ctrl Pts',(4.71573754094257,0.41471486395576,4.1265082550995));
#42965=CARTESIAN_POINT('Ctrl Pts',(4.73959545897399,0.303394668785218,4.30974898215573));
#42966=CARTESIAN_POINT('Ctrl Pts',(4.75988316401932,0.145646585585232,4.40116103141851));
#42967=CARTESIAN_POINT('Ctrl Pts',(4.77221822972086,0.0381762104768988,
4.41583012037823));
#42968=CARTESIAN_POINT('Ctrl Pts',(4.77660065607858,-3.27394476113199E-6,
4.41584059078717));
#42969=CARTESIAN_POINT('Ctrl Pts',(4.5733993439214,2.60627797130011E-6,
4.4159095790646));
#42970=CARTESIAN_POINT('Ctrl Pts',(4.58106907662335,-0.0667838229435618,
4.4158868274511));
#42971=CARTESIAN_POINT('Ctrl Pts',(4.59669144866912,-0.202842099803805,
4.38250385602613));
#42972=CARTESIAN_POINT('Ctrl Pts',(4.62026646005868,-0.360469908510665,
4.24094439618412));
#42973=CARTESIAN_POINT('Ctrl Pts',(4.6441243780901,-0.431844582779732,4.03876871570463));
#42974=CARTESIAN_POINT('Ctrl Pts',(4.66798229612152,-0.397621493350665,
3.82711302819544));
#42975=CARTESIAN_POINT('Ctrl Pts',(4.69184021415294,-0.266169117804412,
3.65773291463971));
#42976=CARTESIAN_POINT('Ctrl Pts',(4.71569813218436,-0.0696311426542753,
3.57204642662242));
#42977=CARTESIAN_POINT('Ctrl Pts',(4.73955605021577,0.143933543589337,3.59100624451743));
#42978=CARTESIAN_POINT('Ctrl Pts',(4.76341396824719,0.322302557754209,3.70997617639404));
#42979=CARTESIAN_POINT('Ctrl Pts',(4.78727188627862,0.421859817202848,3.8998648332327));
#42980=CARTESIAN_POINT('Ctrl Pts',(4.81112980431003,0.41826086011465,4.11423926597311));
#42981=CARTESIAN_POINT('Ctrl Pts',(4.83498772234146,0.312385729531365,4.30067908636799));
#42982=CARTESIAN_POINT('Ctrl Pts',(4.85574423554524,0.15381688120809,4.39891624198015));
#42983=CARTESIAN_POINT('Ctrl Pts',(4.86854810940522,0.04225549351942,4.41582193963064));
#42984=CARTESIAN_POINT('Ctrl Pts',(4.8733993439214,-6.67049670157252E-6,
4.41584593494091));
#42985=CARTESIAN_POINT('Origin',(3.42660065607856,0.,4.));
#42986=CARTESIAN_POINT('',(4.17660065607858,5.88453344125852E-6,4.41584444980552));
#42987=CARTESIAN_POINT('',(4.2733993439214,2.51014653358805E-6,4.41583996132385));
#42988=CARTESIAN_POINT('',(3.42660065607856,4.87367679877478E-13,4.415875));
#42989=CARTESIAN_POINT('Ctrl Pts',(4.17660065607858,5.88453344126799E-6,
4.41584444980552));
#42990=CARTESIAN_POINT('Ctrl Pts',(4.18135488546951,-0.0414115481342504,
4.41582334930757));
#42991=CARTESIAN_POINT('Ctrl Pts',(4.19406175420423,-0.152126265423154,
4.3993918905015));
#42992=CARTESIAN_POINT('Ctrl Pts',(4.21472126228278,-0.310547447266788,
4.30257739619942));
#42993=CARTESIAN_POINT('Ctrl Pts',(4.23857918031418,-0.417556725585918,
4.11678647978038));
#42994=CARTESIAN_POINT('Ctrl Pts',(4.26243709834561,-0.422462345057068,
3.90243789311793));
#42995=CARTESIAN_POINT('Ctrl Pts',(4.28629501637703,-0.324064236326554,
3.71194600226016));
#42996=CARTESIAN_POINT('Ctrl Pts',(4.31015293440845,-0.146423688323203,
3.59189110566319));
#42997=CARTESIAN_POINT('Ctrl Pts',(4.33401085243986,0.0670214896752265,
3.5716299793216));
#42998=CARTESIAN_POINT('Ctrl Pts',(4.35786877047129,0.264078061498623,3.65611697628114));
#42999=CARTESIAN_POINT('Ctrl Pts',(4.38172668850271,0.396560367883193,3.82469274783887));
#43000=CARTESIAN_POINT('Ctrl Pts',(4.40558460653412,0.432072854850341,4.03613591352675));
#43001=CARTESIAN_POINT('Ctrl Pts',(4.42944252456555,0.361931763288092,4.23874286631049));
#43002=CARTESIAN_POINT('Ctrl Pts',(4.45311454108036,0.204524647174786,4.38184685695289));
#43003=CARTESIAN_POINT('Ctrl Pts',(4.46883391825138,0.0676290543833733,
4.4158946000499));
#43004=CARTESIAN_POINT('Ctrl Pts',(4.47660065607858,-1.72413508575881E-6,
4.41591032029986));
#43005=CARTESIAN_POINT('Ctrl Pts',(4.2733993439214,2.51014653359152E-6,
4.41583996132385));
#43006=CARTESIAN_POINT('Ctrl Pts',(4.27768476515387,-0.0373320337329404,
4.41583213221101));
#43007=CARTESIAN_POINT('Ctrl Pts',(4.28992282573015,-0.143955736965383,
4.40160880992953));
#43008=CARTESIAN_POINT('Ctrl Pts',(4.31011352565024,-0.301501118270308,
4.3115924136571));
#43009=CARTESIAN_POINT('Ctrl Pts',(4.33397144368164,-0.413936097932681,
4.12903358037428));
#43010=CARTESIAN_POINT('Ctrl Pts',(4.35782936171308,-0.425152419412173,
3.91492252699502));
#43011=CARTESIAN_POINT('Ctrl Pts',(4.38168727974448,-0.332407397051365,
3.72161523052345));
#43012=CARTESIAN_POINT('Ctrl Pts',(4.40554519777592,-0.158379709595794,
3.5963805946708));
#43013=CARTESIAN_POINT('Ctrl Pts',(4.42940311580732,0.0543761300157755,
3.56984189703405));
#43014=CARTESIAN_POINT('Ctrl Pts',(4.45326103383876,0.25383552520097,3.64848857324589));
#43015=CARTESIAN_POINT('Ctrl Pts',(4.47711895187016,0.39122521984844,3.81308936806525));
#43016=CARTESIAN_POINT('Ctrl Pts',(4.50097686990159,0.432949691632991,4.02339490384879));
#43017=CARTESIAN_POINT('Ctrl Pts',(4.524834787933,0.368806170420464,4.22797974831721));
#43018=CARTESIAN_POINT('Ctrl Pts',(4.54869270596443,0.214479494504121,4.37681733431002));
#43019=CARTESIAN_POINT('Ctrl Pts',(4.56488089129389,0.0741790848482271,
4.4152866170047));
#43020=CARTESIAN_POINT('Ctrl Pts',(4.57311643727954,0.0024660981813593,
4.41591041828323));
#43021=CARTESIAN_POINT('Ctrl Pts',(4.5733993439214,2.60627797130011E-6,
4.4159095790646));
#43022=CARTESIAN_POINT('Origin',(4.,0.,4.));
#43023=CARTESIAN_POINT('',(4.,-7.34788079488412E-17,4.6));
#43024=CARTESIAN_POINT('Origin',(4.,0.,4.));
#43025=CARTESIAN_POINT('',(4.,-0.219892372742957,4.3529863453938));
#43026=CARTESIAN_POINT('Ctrl Pts',(4.,-0.219914231356238,4.35301468169996));
#43027=CARTESIAN_POINT('Ctrl Pts',(4.,-0.219843051329574,4.3531167999744));
#43028=CARTESIAN_POINT('Ctrl Pts',(4.,-0.219771822781512,4.35321888245988));
#43029=CARTESIAN_POINT('Ctrl Pts',(4.,-0.21970054575756,4.3533209291203));
#43030=CARTESIAN_POINT('Ctrl Pts',(4.,-0.207925336055227,4.3701793886806));
#43031=CARTESIAN_POINT('Ctrl Pts',(4.,-0.194831304039315,4.38605734350833));
#43032=CARTESIAN_POINT('Ctrl Pts',(4.,-0.18064579384139,4.40088380688851));
#43033=CARTESIAN_POINT('Ctrl Pts',(4.,-0.168975273508986,4.41308164397169));
#43034=CARTESIAN_POINT('Ctrl Pts',(4.,-0.156565051628872,4.42456888924957));
#43035=CARTESIAN_POINT('Ctrl Pts',(4.,-0.143515931303371,4.43531683418355));
#43036=CARTESIAN_POINT('Ctrl Pts',(4.,-0.133182439541062,4.44382804395605));
#43037=CARTESIAN_POINT('Ctrl Pts',(4.,-0.122447811630206,4.45187590303098));
#43038=CARTESIAN_POINT('Ctrl Pts',(4.,-0.111352162047151,4.45944712768208));
#43039=CARTESIAN_POINT('Ctrl Pts',(4.,-0.105068105051177,4.46373511522897));
#43040=CARTESIAN_POINT('Ctrl Pts',(4.,-0.0986661212125077,4.46787107983396));
#43041=CARTESIAN_POINT('Ctrl Pts',(4.,-0.0921733602714696,4.47184061613108));
#43042=CARTESIAN_POINT('Ctrl Pts',(4.,-0.0718171345235072,4.48428598070136));
#43043=CARTESIAN_POINT('Ctrl Pts',(4.,-0.0505350523745213,4.49512244469223));
#43044=CARTESIAN_POINT('Ctrl Pts',(4.,-0.0285775088988711,4.50429938857761));
#43045=CARTESIAN_POINT('Ctrl Pts',(4.,-0.00645956782426854,4.51354336909515));
#43046=CARTESIAN_POINT('Ctrl Pts',(4.,0.0163444141029789,4.52110543571878));
#43047=CARTESIAN_POINT('Ctrl Pts',(4.,0.0396343143342583,4.52702898180467));
#43048=CARTESIAN_POINT('Ctrl Pts',(4.,0.0479455316904685,4.52914285427945));
#43049=CARTESIAN_POINT('Ctrl Pts',(4.,0.0563191235587283,4.53104786585874));
#43050=CARTESIAN_POINT('Ctrl Pts',(4.,0.0647475081636451,4.53274519105122));
#43051=CARTESIAN_POINT('Ctrl Pts',(4.,0.0709442475001029,4.53399310299165));
#43052=CARTESIAN_POINT('Ctrl Pts',(4.,0.0771669940275102,4.53512789739638));
#43053=CARTESIAN_POINT('Ctrl Pts',(4.,0.0834037601527001,4.53614909266968));
#43054=CARTESIAN_POINT('Ctrl Pts',(4.,0.108500755516298,4.54025842313435));
#43055=CARTESIAN_POINT('Ctrl Pts',(4.,0.133859781029961,4.54253781872753));
#43056=CARTESIAN_POINT('Ctrl Pts',(3.99999999999999,0.159256593756596,4.54305292380224));
#43057=CARTESIAN_POINT('Ctrl Pts',(3.99999999999999,0.185497795908202,4.5435851550133));
#43058=CARTESIAN_POINT('Ctrl Pts',(3.99999999999998,0.211780221987087,4.54223483664603));
#43059=CARTESIAN_POINT('Ctrl Pts',(3.99999999999998,0.237902321580844,4.5390442708621));
#43060=CARTESIAN_POINT('Ctrl Pts',(3.99999999999998,0.243507595489062,4.53835964001621));
#43061=CARTESIAN_POINT('Ctrl Pts',(3.99999999999998,0.249105619801251,4.53759013757336));
#43062=CARTESIAN_POINT('Ctrl Pts',(3.99999999999998,0.254694598474614,4.53673594206822));
#43063=CARTESIAN_POINT('',(4.,-0.219892372743086,3.64701365460628));
#43064=CARTESIAN_POINT('Ctrl Pts',(4.,0.254721014554616,3.46322028700966));
#43065=CARTESIAN_POINT('Ctrl Pts',(4.,0.254552373521139,3.46319452321125));
#43066=CARTESIAN_POINT('Ctrl Pts',(4.,0.254383724765285,3.46316883668624));
#43067=CARTESIAN_POINT('Ctrl Pts',(4.,0.254215068323085,3.46314322746093));
#43068=CARTESIAN_POINT('Ctrl Pts',(4.,0.228435861761457,3.4592288468388));
#43069=CARTESIAN_POINT('Ctrl Pts',(4.,0.202474691352968,3.45711700011808));
#43070=CARTESIAN_POINT('Ctrl Pts',(4.,0.176517231963435,3.45683380906617));
#43071=CARTESIAN_POINT('Ctrl Pts',(4.,0.151199179447316,3.45655759382427));
#43072=CARTESIAN_POINT('Ctrl Pts',(4.,0.125883695414598,3.45802192769867));
#43073=CARTESIAN_POINT('Ctrl Pts',(4.,0.1007794950383,3.46128259448669));
#43074=CARTESIAN_POINT('Ctrl Pts',(4.,0.0854593772715275,3.46327245269535));
#43075=CARTESIAN_POINT('Ctrl Pts',(4.,0.0702187270328167,3.46593187194604));
#43076=CARTESIAN_POINT('Ctrl Pts',(4.,0.0551140352340102,3.4692772918897));
#43077=CARTESIAN_POINT('Ctrl Pts',(4.,0.0468842919617017,3.47110003330284));
#43078=CARTESIAN_POINT('Ctrl Pts',(4.,0.0386923719445779,3.47312744960567));
#43079=CARTESIAN_POINT('Ctrl Pts',(4.,0.0305707631998946,3.47535548770785));
#43080=CARTESIAN_POINT('Ctrl Pts',(4.,0.0102648423897012,3.48092610391051));
#43081=CARTESIAN_POINT('Ctrl Pts',(4.,-0.00963556638195036,3.48775588581666));
#43082=CARTESIAN_POINT('Ctrl Pts',(4.,-0.0289965775380143,3.49587186612014));
#43083=CARTESIAN_POINT('Ctrl Pts',(4.,-0.047965755796229,3.50382359322137));
#43084=CARTESIAN_POINT('Ctrl Pts',(4.,-0.0664174073931304,3.51301096346156));
#43085=CARTESIAN_POINT('Ctrl Pts',(4.,-0.0841982143338667,3.52340033683134));
#43086=CARTESIAN_POINT('Ctrl Pts',(4.,-0.0930898199841631,3.5285957259532));
#43087=CARTESIAN_POINT('Ctrl Pts',(4.,-0.101813128894432,3.53409169793663));
#43088=CARTESIAN_POINT('Ctrl Pts',(4.,-0.110345561972859,3.53988353361915));
#43089=CARTESIAN_POINT('Ctrl Pts',(4.,-0.11586100642067,3.5436274303089));
#43090=CARTESIAN_POINT('Ctrl Pts',(4.,-0.121288652521606,3.54748953413154));
#43091=CARTESIAN_POINT('Ctrl Pts',(4.,-0.126621987542688,3.55146681430013));
#43092=CARTESIAN_POINT('Ctrl Pts',(4.,-0.143297831161627,3.56390265451229));
#43093=CARTESIAN_POINT('Ctrl Pts',(4.,-0.159061930875806,3.57746928852925));
#43094=CARTESIAN_POINT('Ctrl Pts',(4.,-0.173743808224101,3.59211536896244));
#43095=CARTESIAN_POINT('Ctrl Pts',(4.,-0.187864697165731,3.60620182877415));
#43096=CARTESIAN_POINT('Ctrl Pts',(4.,-0.200984288190684,3.62128798311348));
#43097=CARTESIAN_POINT('Ctrl Pts',(4.,-0.212904831975564,3.63731335989365));
#43098=CARTESIAN_POINT('Ctrl Pts',(4.,-0.21528245268753,3.64050971304978));
#43099=CARTESIAN_POINT('Ctrl Pts',(4.,-0.217612227418936,3.64374335030505));
#43100=CARTESIAN_POINT('Ctrl Pts',(4.,-0.219892372743211,3.64701365460636));
#43101=CARTESIAN_POINT('Origin',(4.,0.,4.));
#43102=CARTESIAN_POINT('Origin',(2.,0.,4.));
#43103=CARTESIAN_POINT('',(2.,-7.34788079488412E-17,4.6));
#43104=CARTESIAN_POINT('',(2.,-7.34788079488412E-17,4.6));
#43105=CARTESIAN_POINT('Origin',(2.,0.,4.));
#43106=CARTESIAN_POINT('Origin',(2.,0.,4.));
#43107=CARTESIAN_POINT('Ctrl Pts',(3.95224475517895,0.178288362465424,4.37571967666652));
#43108=CARTESIAN_POINT('Ctrl Pts',(3.96019739452275,0.115708609995841,4.40541533085819));
#43109=CARTESIAN_POINT('Ctrl Pts',(3.97610267321037,-0.0245105356436035,
4.43290545314371));
#43110=CARTESIAN_POINT('Ctrl Pts',(3.99996059124178,-0.228962993402626,
4.36819499612132));
#43111=CARTESIAN_POINT('Ctrl Pts',(4.0238185092732,-0.377374743411151,4.21349068386271));
#43112=CARTESIAN_POINT('Ctrl Pts',(4.04767642730463,-0.433534992178268,
4.00656196868444));
#43113=CARTESIAN_POINT('Ctrl Pts',(4.07153434533603,-0.383670022685343,
3.79803920418254));
#43114=CARTESIAN_POINT('Ctrl Pts',(4.09539226336747,-0.239994733226421,
3.63889579340969));
#43115=CARTESIAN_POINT('Ctrl Pts',(4.11925018139887,-0.0376302499649443,
3.56805514133307));
#43116=CARTESIAN_POINT('Ctrl Pts',(4.1431080994303,0.173933765839147,3.60283521426327));
#43117=CARTESIAN_POINT('Ctrl Pts',(4.16696601746172,0.342967344134064,3.73473372141871));
#43118=CARTESIAN_POINT('Ctrl Pts',(4.19082393549313,0.428135478754777,3.93149662217858));
#43119=CARTESIAN_POINT('Ctrl Pts',(4.21468185352456,0.40861313688017,4.1450106963618));
#43120=CARTESIAN_POINT('Ctrl Pts',(4.23853977155597,0.289173588337559,4.32306558264197));
#43121=CARTESIAN_POINT('Ctrl Pts',(4.2623976895874,0.0990233075312312,4.42212219878201));
#43122=CARTESIAN_POINT('Ctrl Pts',(4.28625560761881,-0.115340915390822,
4.41795840454656));
#43123=CARTESIAN_POINT('Ctrl Pts',(4.31011352565024,-0.301501118270308,
4.3115924136571));
#43124=CARTESIAN_POINT('Ctrl Pts',(4.33397144368164,-0.413936097932681,
4.12903358037428));
#43125=CARTESIAN_POINT('Ctrl Pts',(4.35782936171308,-0.425152419412173,
3.91492252699502));
#43126=CARTESIAN_POINT('Ctrl Pts',(4.38168727974448,-0.332407397051365,
3.72161523052345));
#43127=CARTESIAN_POINT('Ctrl Pts',(4.40554519777592,-0.158379709595794,
3.5963805946708));
#43128=CARTESIAN_POINT('Ctrl Pts',(4.42940311580732,0.0543761300157755,
3.56984189703405));
#43129=CARTESIAN_POINT('Ctrl Pts',(4.45326103383876,0.25383552520097,3.64848857324589));
#43130=CARTESIAN_POINT('Ctrl Pts',(4.47711895187016,0.39122521984844,3.81308936806525));
#43131=CARTESIAN_POINT('Ctrl Pts',(4.50097686990159,0.432949691632991,4.02339490384879));
#43132=CARTESIAN_POINT('Ctrl Pts',(4.524834787933,0.368806170420464,4.22797974831721));
#43133=CARTESIAN_POINT('Ctrl Pts',(4.54869270596443,0.214479494504121,4.37681733431002));
#43134=CARTESIAN_POINT('Ctrl Pts',(4.57255062399584,0.00770673985495463,
4.4335128177492));
#43135=CARTESIAN_POINT('Ctrl Pts',(4.59640854202726,-0.200950522604244,
4.38420260860549));
#43136=CARTESIAN_POINT('Ctrl Pts',(4.62026646005868,-0.360469908510665,
4.24094439618412));
#43137=CARTESIAN_POINT('Ctrl Pts',(4.6441243780901,-0.431844582779732,4.03876871570463));
#43138=CARTESIAN_POINT('Ctrl Pts',(4.66798229612152,-0.397621493350665,
3.82711302819544));
#43139=CARTESIAN_POINT('Ctrl Pts',(4.69184021415294,-0.266169117804412,
3.65773291463971));
#43140=CARTESIAN_POINT('Ctrl Pts',(4.71569813218436,-0.0696311426542753,
3.57204642662242));
#43141=CARTESIAN_POINT('Ctrl Pts',(4.73955605021577,0.143933543589337,3.59100624451743));
#43142=CARTESIAN_POINT('Ctrl Pts',(4.76341396824719,0.322302557754209,3.70997617639404));
#43143=CARTESIAN_POINT('Ctrl Pts',(4.78727188627862,0.421859817202848,3.8998648332327));
#43144=CARTESIAN_POINT('Ctrl Pts',(4.81112980431003,0.41826086011465,4.11423926597311));
#43145=CARTESIAN_POINT('Ctrl Pts',(4.83498772234146,0.312385729531365,4.30067908636799));
#43146=CARTESIAN_POINT('Ctrl Pts',(4.85884564037287,0.130123778861223,4.41359467981201));
#43147=CARTESIAN_POINT('Ctrl Pts',(4.88270355840429,-0.0839569802410516,
4.42537510794913));
#43148=CARTESIAN_POINT('Ctrl Pts',(4.90656147643571,-0.277507970732168,
4.33313973520738));
#43149=CARTESIAN_POINT('Ctrl Pts',(4.93041939446713,-0.403200703213916,
4.15944262266324));
#43150=CARTESIAN_POINT('Ctrl Pts',(4.95427731249855,-0.430299880793222,
3.94675744574809));
#43151=CARTESIAN_POINT('Ctrl Pts',(4.97813523052996,-0.352179016385168,
3.7470915236456));
#43152=CARTESIAN_POINT('Ctrl Pts',(5.00199314856139,-0.187940789307144,
3.60926861310034));
#43153=CARTESIAN_POINT('Ctrl Pts',(5.0258510665928,0.0222540801607904,3.56699016996131));
#43154=CARTESIAN_POINT('Ctrl Pts',(5.04970898462423,0.227007220840439,3.63059442521772));
#43155=CARTESIAN_POINT('Ctrl Pts',(5.07356690265564,0.376250912472057,3.7845284059142));
#43156=CARTESIAN_POINT('Ctrl Pts',(5.09742482068706,0.433491007135177,3.99115106069306));
#43157=CARTESIAN_POINT('Ctrl Pts',(5.12128273871848,0.384730742495793,4.19993752217271));
#43158=CARTESIAN_POINT('Ctrl Pts',(5.1451406567499,0.241893331461176,4.35983381329239));
#43159=CARTESIAN_POINT('Ctrl Pts',(5.16899857478132,0.0399064118422473,
4.43174093538579));
#43160=CARTESIAN_POINT('Ctrl Pts',(5.19285649281273,-0.171838712500945,
4.39807563839043));
#43161=CARTESIAN_POINT('Ctrl Pts',(5.21671441084416,-0.341564590845109,
4.26707000444592));
#43162=CARTESIAN_POINT('Ctrl Pts',(5.24057232887557,-0.427768622694993,
4.07075847957352));
#43163=CARTESIAN_POINT('Ctrl Pts',(5.264430246907,-0.409371574112622,3.85714457902312));
#43164=CARTESIAN_POINT('Ctrl Pts',(5.2882881649384,-0.290872024601924,3.6784627202051));
#43165=CARTESIAN_POINT('Ctrl Pts',(5.31214608296984,-0.101246341881189,
3.57840548479658));
#43166=CARTESIAN_POINT('Ctrl Pts',(5.33600400100125,0.113136829324483,3.58143959235932));
#43167=CARTESIAN_POINT('Ctrl Pts',(5.35986191903268,0.299854963974951,3.68682312094679));
#43168=CARTESIAN_POINT('Ctrl Pts',(5.38371983706408,0.413250392048343,3.8687869272297));
#43169=CARTESIAN_POINT('Ctrl Pts',(5.40757775509551,0.425594842551202,4.08283590397723));
#43170=CARTESIAN_POINT('Ctrl Pts',(5.43143567312693,0.333869761079625,4.27662924579771));
#43171=CARTESIAN_POINT('Ctrl Pts',(5.45529359115834,0.160504428594232,4.4027792017911));
#43172=CARTESIAN_POINT('Ctrl Pts',(5.47915150918977,-0.0521086087350157,
4.43043867146175));
#43173=CARTESIAN_POINT('Ctrl Pts',(5.50300942722118,-0.251979671819092,
4.35284416104532));
#43174=CARTESIAN_POINT('Ctrl Pts',(5.52686734525261,-0.390234841353927,
4.18896964197264));
#43175=CARTESIAN_POINT('Ctrl Pts',(5.55072526328402,-0.433066962396004,
3.97888689800548));
#43176=CARTESIAN_POINT('Ctrl Pts',(5.57458318131544,-0.370002414621403,
3.77396688259));
#43177=CARTESIAN_POINT('Ctrl Pts',(5.59844109934686,-0.21646219781534,3.62431812139094));
#43178=CARTESIAN_POINT('Ctrl Pts',(5.62229901737828,-0.00999107731853999,
3.56653381289738));
#43179=CARTESIAN_POINT('Ctrl Pts',(5.64615693540971,0.198923133709572,3.61474379450078));
#43180=CARTESIAN_POINT('Ctrl Pts',(5.67001485344111,0.359195220034686,3.75715941257656));
#43181=CARTESIAN_POINT('Ctrl Pts',(5.69387277147254,0.431634290692432,3.95895616900985));
#43182=CARTESIAN_POINT('Ctrl Pts',(5.71773068950395,0.398527019959163,4.1707892603438));
#43183=CARTESIAN_POINT('Ctrl Pts',(5.74158860753538,0.267969036875697,4.34085972491723));
#43184=CARTESIAN_POINT('Ctrl Pts',(5.76544652556679,0.0718853255354575,
4.42758070267197));
#43185=CARTESIAN_POINT('Ctrl Pts',(5.78930444359821,-0.141776307127955,
4.40974655013133));
#43186=CARTESIAN_POINT('Ctrl Pts',(5.81316236162963,-0.320769768688322,
4.29171820750724));
#43187=CARTESIAN_POINT('Ctrl Pts',(5.83702027966105,-0.421326288178809,
4.10235681181338));
#43188=CARTESIAN_POINT('Ctrl Pts',(5.86087819769247,-0.418857046020503,
3.88796639709818));
#43189=CARTESIAN_POINT('Ctrl Pts',(5.88473611572389,-0.313965860818636,
3.70097123187977));
#43190=CARTESIAN_POINT('Ctrl Pts',(5.90859403375531,-0.132301443679057,
3.58709678011166));
#43191=CARTESIAN_POINT('Ctrl Pts',(5.93245195178673,0.0817142298265842,
3.57418834816524));
#43192=CARTESIAN_POINT('Ctrl Pts',(5.95630986981814,0.275748643515392,3.66540258613358));
#43193=CARTESIAN_POINT('Ctrl Pts',(5.98016778784957,0.402354822815078,3.83843477537114));
#43194=CARTESIAN_POINT('Ctrl Pts',(6.00402570588098,0.430574627524036,4.05097449853386));
#43195=CARTESIAN_POINT('Ctrl Pts',(6.02788362391241,0.353506566116634,4.25104874587108));
#43196=CARTESIAN_POINT('Ctrl Pts',(6.05174154194382,0.189997730437525,4.38973628930191));
#43197=CARTESIAN_POINT('Ctrl Pts',(6.07559945997525,-0.0199730113800777,
4.43311976162365));
#43198=CARTESIAN_POINT('Ctrl Pts',(6.09945737800665,-0.2250554921608,4.3705991908187));
#43199=CARTESIAN_POINT('Ctrl Pts',(6.12331529603809,-0.375113923638194,
4.21744656883549));
#43200=CARTESIAN_POINT('Ctrl Pts',(6.1471732140695,-0.433431396087355,4.01114207710762));
#43201=CARTESIAN_POINT('Ctrl Pts',(6.17103113210093,-0.385792139046387,
3.80207577201042));
#43202=CARTESIAN_POINT('Ctrl Pts',(6.19488905013233,-0.243761337718234,
3.64147770828707));
#43203=CARTESIAN_POINT('Ctrl Pts',(6.21874696816376,-0.042227823444436,
3.56841523311022));
#43204=CARTESIAN_POINT('Ctrl Pts',(6.24260488619517,0.16982704650124,3.60113783246665));
#43205=CARTESIAN_POINT('Ctrl Pts',(6.2664628042266,0.339985970990829,3.73091992247201));
#43206=CARTESIAN_POINT('Ctrl Pts',(6.29032072225801,0.427700638223926,3.92738904240251));
#43207=CARTESIAN_POINT('Ctrl Pts',(6.31417864028943,0.409561128158778,4.13996490148311));
#43208=CARTESIAN_POINT('Ctrl Pts',(6.34598919766466,0.254661277208374,4.38159318714805));
#43209=CARTESIAN_POINT('Ctrl Pts',(6.38575239438369,-0.125272905304917,
4.47558432627151));
#43210=CARTESIAN_POINT('Ctrl Pts',(6.43346823044653,-0.468271923807345,
4.15124960425567));
#43211=CARTESIAN_POINT('Ctrl Pts',(6.48118406650937,-0.380227249479543,
3.6882349865083));
#43212=CARTESIAN_POINT('Ctrl Pts',(6.52889990257221,0.0564566449812287,
3.51140415777354));
#43213=CARTESIAN_POINT('Ctrl Pts',(6.57661573863504,0.441574375138847,3.78331933667001));
#43214=CARTESIAN_POINT('Ctrl Pts',(6.62433157469789,0.421040068198854,4.25418342072721));
#43215=CARTESIAN_POINT('Ctrl Pts',(6.67204741076071,0.0139362792425842,
4.49164405688148));
#43216=CARTESIAN_POINT('Ctrl Pts',(6.71976324682356,-0.406006764042365,
4.27761133505345));
#43217=CARTESIAN_POINT('Ctrl Pts',(6.76747908288639,-0.453085647428837,
3.80864864857145));
#43218=CARTESIAN_POINT('Ctrl Pts',(6.81519491894923,-0.0841006081168706,
3.51540431248109));
#43219=CARTESIAN_POINT('Ctrl Pts',(6.86291075501207,0.362121456530253,3.66717299786736));
#43220=CARTESIAN_POINT('Ctrl Pts',(6.91062659107491,0.475798562415156,4.124581128109));
#43221=CARTESIAN_POINT('Ctrl Pts',(6.95834242713775,0.152544250279933,4.46758486877347));
#43222=CARTESIAN_POINT('Ctrl Pts',(7.00605826320058,-0.310794706562241,
4.38119802990972));
#43223=CARTESIAN_POINT('Ctrl Pts',(7.05377409926342,-0.488725618924084,
3.94475128051735));
#43224=CARTESIAN_POINT('Ctrl Pts',(7.10148993532626,-0.21785253135038,3.55904022429238));
#43225=CARTESIAN_POINT('Ctrl Pts',(7.14920577138909,0.253078023397415,3.57826934481931));
#43226=CARTESIAN_POINT('Ctrl Pts',(7.19692160745195,0.491603063369337,3.98478019943955));
#43227=CARTESIAN_POINT('Ctrl Pts',(7.24463744351477,0.278681483980911,4.40526763942622));
#43228=CARTESIAN_POINT('Ctrl Pts',(7.29235327957762,-0.190157610347023,
4.45359156587464));
#43229=CARTESIAN_POINT('Ctrl Pts',(7.34006911564044,-0.484372034479295,
4.08537538031203));
#43230=CARTESIAN_POINT('Ctrl Pts',(7.3877849517033,-0.333780171974684,3.63875766810317));
#43231=CARTESIAN_POINT('Ctrl Pts',(7.43550078776612,0.123327161313159,3.52387434835784));
#43232=CARTESIAN_POINT('Ctrl Pts',(7.48321662382897,0.467181263150904,3.84622454030349));
#43233=CARTESIAN_POINT('Ctrl Pts',(7.5309324598918,0.382015623368301,4.30978910321172));
#43234=CARTESIAN_POINT('Ctrl Pts',(7.57864829595465,-0.0539608418635878,
4.4888695658253));
#43235=CARTESIAN_POINT('Ctrl Pts',(7.62636413201748,-0.440384235482588,
4.21901358396786));
#43236=CARTESIAN_POINT('Ctrl Pts',(7.67407996808031,-0.422396009600076,
3.7480340579683));
#43237=CARTESIAN_POINT('Ctrl Pts',(7.72179580414317,-0.0165150286377962,
3.50843873354525));
#43238=CARTESIAN_POINT('Ctrl Pts',(7.76951164020598,0.404531957204003,3.72025168374225));
#43239=CARTESIAN_POINT('Ctrl Pts',(7.81722747626884,0.454091022239626,4.18896181724392));
#43240=CARTESIAN_POINT('Ctrl Pts',(7.86494331233166,0.0866513144543145,
4.48414540641706));
#43241=CARTESIAN_POINT('Ctrl Pts',(7.91265914839452,-0.360361628691054,
4.33473081934393));
#43242=CARTESIAN_POINT('Ctrl Pts',(7.96037498445733,-0.476448943335793,
3.87792777037096));
#43243=CARTESIAN_POINT('Ctrl Pts',(8.0080908205202,-0.1550058622045,3.53322552818936));
#43244=CARTESIAN_POINT('Ctrl Pts',(8.05580665658301,0.308781487260178,3.61716946571973));
#43245=CARTESIAN_POINT('Ctrl Pts',(8.10352249264587,0.489010045760349,4.0526725734847));
#43246=CARTESIAN_POINT('Ctrl Pts',(8.1512383287087,0.220173154851853,4.43980564654689));
#43247=CARTESIAN_POINT('Ctrl Pts',(8.19895416477154,-0.250852131956433,
4.4230584271054));
#43248=CARTESIAN_POINT('Ctrl Pts',(8.24667000083438,-0.491516046133,4.01781014446235));
#43249=CARTESIAN_POINT('Ctrl Pts',(8.29438583689722,-0.280813212199106,
3.59620653211525));
#43250=CARTESIAN_POINT('Ctrl Pts',(8.34210167296004,0.187764715363875,3.54541267448783));
#43251=CARTESIAN_POINT('Ctrl Pts',(8.38981750902289,0.483915415676709,3.91207335260334));
#43252=CARTESIAN_POINT('Ctrl Pts',(8.43753334508573,0.335679143777854,4.35947842394856));
#43253=CARTESIAN_POINT('Ctrl Pts',(8.48524918114857,-0.120816450939738,
4.4767689272953));
#43254=CARTESIAN_POINT('Ctrl Pts',(8.5329650172114,-0.466364439759318,4.15623518867385));
#43255=CARTESIAN_POINT('Ctrl Pts',(8.58068085327425,-0.383642787608637,
3.69222827230584));
#43256=CARTESIAN_POINT('Ctrl Pts',(8.62839668933707,0.0513839395061145,
3.51085286915611));
#43257=CARTESIAN_POINT('Ctrl Pts',(8.67611252539993,0.439224004328866,3.77866880275638));
#43258=CARTESIAN_POINT('Ctrl Pts',(8.72382836146275,0.42371790764641,4.24973658040369));
#43259=CARTESIAN_POINT('Ctrl Pts',(8.7715441975256,0.0191051366342138,4.49146741357506));
#43260=CARTESIAN_POINT('Ctrl Pts',(8.81926003358843,-0.403052175319494,
4.28187615866228));
#43261=CARTESIAN_POINT('Ctrl Pts',(8.86697586965126,-0.455080472922433,
3.81343369002772));
#43262=CARTESIAN_POINT('Ctrl Pts',(8.91469170571412,-0.0892013699275644,
3.51631793453238));
#43263=CARTESIAN_POINT('Ctrl Pts',(8.96240754177693,0.358592723611288,3.66337486216116));
#43264=CARTESIAN_POINT('Ctrl Pts',(9.0101233778398,0.477085601399612,4.11955983351088));
#43265=CARTESIAN_POINT('Ctrl Pts',(9.05783921390261,0.157463430517111,4.46595117008304));
#43266=CARTESIAN_POINT('Ctrl Pts',(9.10555504996547,-0.306759831495564,
4.38445237758765));
#43267=CARTESIAN_POINT('Ctrl Pts',(9.1532708860283,-0.489280820139143,3.94990505119329));
#43268=CARTESIAN_POINT('Ctrl Pts',(9.20098672209113,-0.222487703095825,
3.56136068709803));
#43269=CARTESIAN_POINT('Ctrl Pts',(9.24870255815399,0.248619295113741,3.57562555337399));
#43270=CARTESIAN_POINT('Ctrl Pts',(9.29641839421681,0.49141536912078,3.97960000382683));
#43271=CARTESIAN_POINT('Ctrl Pts',(9.34413423027966,0.282937148266828,4.40230808465976));
#43272=CARTESIAN_POINT('Ctrl Pts',(9.39185006634249,-0.185366609388173,
4.45557046104408));
#43273=CARTESIAN_POINT('Ctrl Pts',(9.43956590240532,-0.483445357410111,
4.09047547319903));
#43274=CARTESIAN_POINT('Ctrl Pts',(9.48728173846818,-0.337568794959357,
3.64229546617122));
#43275=CARTESIAN_POINT('Ctrl Pts',(9.53499757453099,0.118302386066128,3.5226010365501));
#43276=CARTESIAN_POINT('Ctrl Pts',(9.58271341059386,0.465534665650901,3.84130942079228));
#43277=CARTESIAN_POINT('Ctrl Pts',(9.63042924665667,0.385259298596883,4.30574580568933));
#43278=CARTESIAN_POINT('Ctrl Pts',(9.67814508271952,-0.0488056103349303,
4.48941111271794));
#43279=CARTESIAN_POINT('Ctrl Pts',(9.72586091878235,-0.438051576325333,
4.22364266437974));
#43280=CARTESIAN_POINT('Ctrl Pts',(9.77357675484519,-0.425028039486299,
3.75249971615691));
#43281=CARTESIAN_POINT('Ctrl Pts',(9.82129259090803,-0.0216947140899849,
3.50864008686857));
#43282=CARTESIAN_POINT('Ctrl Pts',(9.86900842697087,0.401561201071248,3.7160038263529));
#43283=CARTESIAN_POINT('Ctrl Pts',(9.91672426303371,0.456057286475463,4.18416562194019));
#43284=CARTESIAN_POINT('Ctrl Pts',(9.96444009909655,0.0917489483659128,
4.48320529314746));
#43285=CARTESIAN_POINT('Ctrl Pts',(10.0121559351594,-0.356813860767086,
4.3385101085883));
#43286=CARTESIAN_POINT('Ctrl Pts',(10.0598717712222,-0.477709011270712,
3.88295588266498));
#43287=CARTESIAN_POINT('Ctrl Pts',(10.1075876072851,-0.159916626226494,
3.53488507064564));
#43288=CARTESIAN_POINT('Ctrl Pts',(10.1553034433479,0.304729657315094,3.61393645496551));
#43289=CARTESIAN_POINT('Ctrl Pts',(10.2030192794107,0.489538007675758,4.04751593304174));
#43290=CARTESIAN_POINT('Ctrl Pts',(10.2507351154736,0.224796073077312,4.43746079867915));
#43291=CARTESIAN_POINT('Ctrl Pts',(10.2984509515364,-0.246379554360218,
4.42567868168988));
#43292=CARTESIAN_POINT('Ctrl Pts',(10.3461667875993,-0.491301045992024,
4.02298928139638));
#43293=CARTESIAN_POINT('Ctrl Pts',(10.3938826236621,-0.285053227451061,
3.599188470261));
#43294=CARTESIAN_POINT('Ctrl Pts',(10.4415984597249,0.182963355965895,3.54345905416307));
#43295=CARTESIAN_POINT('Ctrl Pts',(10.4893142957878,0.482961874346273,3.9069782134126));
#43296=CARTESIAN_POINT('Ctrl Pts',(10.5370301318506,0.339449072190825,4.35592071060949));
#43297=CARTESIAN_POINT('Ctrl Pts',(10.5847459679134,-0.115785036052801,
4.47801574270962));
#43298=CARTESIAN_POINT('Ctrl Pts',(10.6324618039763,-0.464691964107356,
4.16114156306187));
#43299=CARTESIAN_POINT('Ctrl Pts',(10.6801776400391,-0.386865111317189,
3.69628860657276));
#43300=CARTESIAN_POINT('Ctrl Pts',(10.7278934761019,0.0462259258804368,
3.51033849586834));
#43301=CARTESIAN_POINT('Ctrl Pts',(10.7756093121648,0.436866984064762,3.77405207881873));
#43302=CARTESIAN_POINT('Ctrl Pts',(10.8233251482276,0.426326368719826,4.24525711444552));
#43303=CARTESIAN_POINT('Ctrl Pts',(10.8710409842905,0.0242836891050981,
4.49123876811122));
#43304=CARTESIAN_POINT('Ctrl Pts',(10.9187568203533,-0.400059075867425,
4.28610830234036));
#43305=CARTESIAN_POINT('Ctrl Pts',(10.9664726564161,-0.45702143577077,3.81824018018824));
#43306=CARTESIAN_POINT('Ctrl Pts',(11.014188492479,-0.0942939790271268,
3.51728489730359));
#43307=CARTESIAN_POINT('Ctrl Pts',(11.0619043285418,0.355025089556487,3.65961432075161));
#43308=CARTESIAN_POINT('Ctrl Pts',(11.1096201646047,0.478319155637209,4.11452515096033));
#43309=CARTESIAN_POINT('Ctrl Pts',(11.1573360006675,0.16236538121005,4.46426577284621));
#43310=CARTESIAN_POINT('Ctrl Pts',(11.2050518367304,-0.302691021094817,
4.38766399188028));
#43311=CARTESIAN_POINT('Ctrl Pts',(11.2527676727932,-0.489781601228288,
3.95506440219344));
#43312=CARTESIAN_POINT('Ctrl Pts',(11.300483508856,-0.227098200695192,3.56372986339542));
#43313=CARTESIAN_POINT('Ctrl Pts',(11.3481993449188,0.244132971891272,3.57302890392028));
#43314=CARTESIAN_POINT('Ctrl Pts',(11.3959151809817,0.491173079921361,3.97442207176994));
#43315=CARTESIAN_POINT('Ctrl Pts',(11.4436310170445,0.287161390990383,4.39930384468027));
#43316=CARTESIAN_POINT('Ctrl Pts',(11.4913468531074,-0.180555021833016,
4.45749875294131));
#43317=CARTESIAN_POINT('Ctrl Pts',(11.5390626891702,-0.482464979911041,
4.09556551685319));
#43318=CARTESIAN_POINT('Ctrl Pts',(11.586778525233,-0.341319923258817,3.64587299617429));
#43319=CARTESIAN_POINT('Ctrl Pts',(11.6344943612959,0.113264470804062,3.5213807520529));
#43320=CARTESIAN_POINT('Ctrl Pts',(11.6822101973587,0.463836358529674,3.83641192782507));
#43321=CARTESIAN_POINT('Ctrl Pts',(11.7299260334216,0.38846018117773,4.30166854740152));
#43322=CARTESIAN_POINT('Ctrl Pts',(11.7776418694844,-0.0436449577779122,
4.48989829813191));
#43323=CARTESIAN_POINT('Ctrl Pts',(11.8253577055472,-0.435670260442099,
4.22824690363353));
#43324=CARTESIAN_POINT('Ctrl Pts',(11.8730735416101,-0.427612859293677,
3.75699286549843));
#43325=CARTESIAN_POINT('Ctrl Pts',(11.9207893776729,-0.0268719897862959,
3.50889601812151));
#43326=CARTESIAN_POINT('Ctrl Pts',(11.9685052137357,0.398545841420554,3.71178751390968));
#43327=CARTESIAN_POINT('Ctrl Pts',(12.0162210497986,0.457972894034889,4.17934897039372));
#43328=CARTESIAN_POINT('Ctrl Pts',(12.0639368858614,0.0968363912382316,
4.48221150772657));
#43329=CARTESIAN_POINT('Ctrl Pts',(12.1116527219243,-0.353226459651896,
4.34225179773635));
#43330=CARTESIAN_POINT('Ctrl Pts',(12.1593685579871,-0.478916017555994,
3.88799699566402));
#43331=CARTESIAN_POINT('Ctrl Pts',(12.2070843940499,-0.164809627468288,
3.53659627586117));
#43332=CARTESIAN_POINT('Ctrl Pts',(12.2548002301128,0.300643979445627,3.61074632631782));
#43333=CARTESIAN_POINT('Ctrl Pts',(12.3025160661756,0.490011594032383,4.04235401475446));
#43334=CARTESIAN_POINT('Ctrl Pts',(12.3502319022385,0.229394022021679,4.43506735974179));
#43335=CARTESIAN_POINT('Ctrl Pts',(12.3979477383013,-0.241879610092261,
4.42825165390643));
#43336=CARTESIAN_POINT('Ctrl Pts',(12.4456635743641,-0.491031474462283,
4.0281658647901));
#43337=CARTESIAN_POINT('Ctrl Pts',(12.493379410427,-0.289261580343189,3.60221492864948));
#43338=CARTESIAN_POINT('Ctrl Pts',(12.5410952464898,0.178141673866572,3.54155614424011));
#43339=CARTESIAN_POINT('Ctrl Pts',(12.5888110825527,0.481954687902679,3.90189340664049));
#43340=CARTESIAN_POINT('Ctrl Pts',(12.6365269186155,0.343181296211668,4.35232346328687));
#43341=CARTESIAN_POINT('Ctrl Pts',(12.6842427546783,-0.110740760313508,
4.47920946240362));
#43342=CARTESIAN_POINT('Ctrl Pts',(12.7319585907412,-0.462967872677167,
4.16603003860975));
#43343=CARTESIAN_POINT('Ctrl Pts',(12.779674426804,-0.390044463885,3.70038267566003));
#43344=CARTESIAN_POINT('Ctrl Pts',(12.8273902628668,0.0410627776982723,
3.50987851185683));
#43345=CARTESIAN_POINT('Ctrl Pts',(12.8751060989297,0.434461438689172,3.76946045210395));
#43346=CARTESIAN_POINT('Ctrl Pts',(12.9228219349925,0.42888747548329,4.24075040649094));
#43347=CARTESIAN_POINT('Ctrl Pts',(12.9705377710553,0.0294595442590321,
4.49095555817611));
#43348=CARTESIAN_POINT('Ctrl Pts',(13.0182536071182,-0.397021539751646,
4.29030866646591));
#43349=CARTESIAN_POINT('Ctrl Pts',(13.065969443181,-0.458911634846768,3.82306685936703));
#43350=CARTESIAN_POINT('Ctrl Pts',(13.1136852792439,-0.0993761143989603,
3.51830547777773));
#43351=CARTESIAN_POINT('Ctrl Pts',(13.1614011153067,0.351418020999476,3.65589158776806));
#43352=CARTESIAN_POINT('Ctrl Pts',(13.2091169513695,0.479499580452807,4.10947774749948));
#43353=CARTESIAN_POINT('Ctrl Pts',(13.2568327874324,0.167249297126924,4.46252880717046));
#43354=CARTESIAN_POINT('Ctrl Pts',(13.3045486234952,-0.298588589211839,
4.39083254629632));
#43355=CARTESIAN_POINT('Ctrl Pts',(13.352264459558,-0.490227979701372,3.96022874442655));
#43356=CARTESIAN_POINT('Ctrl Pts',(13.3999802956209,-0.23168347330409,3.56614749850931));
#43357=CARTESIAN_POINT('Ctrl Pts',(13.4476961316837,0.239619531536799,3.57047968038978));
#43358=CARTESIAN_POINT('Ctrl Pts',(13.4954119677466,0.490876233547033,3.96924698078795));
#43359=CARTESIAN_POINT('Ctrl Pts',(13.5431278038094,0.291353737189313,4.39625525192456));
#43360=CARTESIAN_POINT('Ctrl Pts',(13.5908436398722,-0.175723379082843,
4.45937622804808));
#43361=CARTESIAN_POINT('Ctrl Pts',(13.6385594759351,-0.481431012491488,
4.10064494554323));
#43362=CARTESIAN_POINT('Ctrl Pts',(13.6862753119979,-0.345033139360895,
3.64948986092447));
#43363=CARTESIAN_POINT('Ctrl Pts',(13.7339911480608,0.108213974662067,3.52021363031051));
#43364=CARTESIAN_POINT('Ctrl Pts',(13.7817069841236,0.462086530666827,3.83153260544464));
#43365=CARTESIAN_POINT('Ctrl Pts',(13.8294228201864,0.391617915445045,4.297557781203));
#43366=CARTESIAN_POINT('Ctrl Pts',(13.8771386562493,-0.0384794573460961,
4.49033106796769));
#43367=CARTESIAN_POINT('Ctrl Pts',(13.9248544923121,-0.433240552373761,
4.23282579030437));
#43368=CARTESIAN_POINT('Ctrl Pts',(13.9725703283749,-0.430150181893835,
3.76151300691929));
#43369=CARTESIAN_POINT('Ctrl Pts',(14.0202861644378,-0.032046280669499,
3.50920649887429));
#43370=CARTESIAN_POINT('Ctrl Pts',(14.0680020005006,0.39548621318905,3.70760321474174));
#43371=CARTESIAN_POINT('Ctrl Pts',(14.1157178365634,0.459837632138507,4.1745123976147));
#43372=CARTESIAN_POINT('Ctrl Pts',(14.1634336726263,0.101913077983734,4.48116416053968));
#43373=CARTESIAN_POINT('Ctrl Pts',(14.2111495086891,-0.349599823817769,
4.34595547117883));
#43374=CARTESIAN_POINT('Ctrl Pts',(14.258865344752,-0.480069828122688,3.8930505494253));
#43375=CARTESIAN_POINT('Ctrl Pts',(14.3065811808148,-0.169684322438749,
3.53835895376334));
#43376=CARTESIAN_POINT('Ctrl Pts',(14.3542970168777,0.296524907469595,3.60759943412104));
#43377=CARTESIAN_POINT('Ctrl Pts',(14.4020128529405,0.49043075222644,4.0371873919842));
#43378=CARTESIAN_POINT('Ctrl Pts',(14.4497286890033,0.233966490966644,4.43262559558668));
#43379=CARTESIAN_POINT('Ctrl Pts',(14.4974445250662,-0.237352798985028,
4.43077705796148));
#43380=CARTESIAN_POINT('Ctrl Pts',(14.545160361129,-0.490707361486496,4.03333931965322));
#43381=CARTESIAN_POINT('Ctrl Pts',(14.5928761971918,-0.293437803431633,
3.60528557111603));
#43382=CARTESIAN_POINT('Ctrl Pts',(14.6405920332547,0.173300204635467,3.53970415608515));
#43383=CARTESIAN_POINT('Ctrl Pts',(14.6883078693175,0.480893968219416,3.89681949708321));
#43384=CARTESIAN_POINT('Ctrl Pts',(14.7360237053804,0.346875401282657,4.34868708154587));
#43385=CARTESIAN_POINT('Ctrl Pts',(14.7837395414432,-0.10568418401607,4.48034995378457));
#43386=CARTESIAN_POINT('Ctrl Pts',(14.831455377506,-0.461192356972643,4.17090007232882));
#43387=CARTESIAN_POINT('Ctrl Pts',(14.8791712135689,-0.393180492164677,
3.7045100248179));
#43388=CARTESIAN_POINT('Ctrl Pts',(14.9268870496317,0.0358950684576197,
3.50947296821438));
#43389=CARTESIAN_POINT('Ctrl Pts',(14.9746028856945,0.432007635398663,3.76489443262817));
#43390=CARTESIAN_POINT('Ctrl Pts',(15.0223187217574,0.431400943461215,4.23621695712364));
#43391=CARTESIAN_POINT('Ctrl Pts',(15.0700345578202,0.0346321271865876,
4.4906178152274));
#43392=CARTESIAN_POINT('Ctrl Pts',(15.1177503938831,-0.393939904367254,
4.2944767844824));
#43393=CARTESIAN_POINT('Ctrl Pts',(15.1654662299459,-0.46075086019608,3.82791319143947));
#43394=CARTESIAN_POINT('Ctrl Pts',(15.2131820660087,-0.104447211543591,
3.51937956259357));
#43395=CARTESIAN_POINT('Ctrl Pts',(15.2608979020716,0.347771918596306,3.652207076714));
#43396=CARTESIAN_POINT('Ctrl Pts',(15.3086137381344,0.480626744730421,4.10441818376995));
#43397=CARTESIAN_POINT('Ctrl Pts',(15.3563295741973,0.172114635785536,4.46074046598969));
#43398=CARTESIAN_POINT('Ctrl Pts',(15.4040454102601,-0.294452991525291,
4.39395768888776));
#43399=CARTESIAN_POINT('Ctrl Pts',(15.4517612463229,-0.490619905976795,
3.96539750426199));
#43400=CARTESIAN_POINT('Ctrl Pts',(15.4994770823858,-0.236243011612202,
3.56861332390027));
#43401=CARTESIAN_POINT('Ctrl Pts',(15.5471929184486,0.235079475381852,3.56797816593814));
#43402=CARTESIAN_POINT('Ctrl Pts',(15.5949087545115,0.490524862970081,3.9640753057054));
#43403=CARTESIAN_POINT('Ctrl Pts',(15.6426245905743,0.295513721197704,4.39316264501585));
#43404=CARTESIAN_POINT('Ctrl Pts',(15.6903404266371,-0.170872217813597,
4.46120267782338));
#43405=CARTESIAN_POINT('Ctrl Pts',(15.7380562626999,-0.480343569999647,
4.1057131950703));
#43406=CARTESIAN_POINT('Ctrl Pts',(15.7857720987628,-0.348708030819167,
3.6531456586776));
#43407=CARTESIAN_POINT('Ctrl Pts',(15.8334879348256,0.103151458625294,3.5190998009613));
#43408=CARTESIAN_POINT('Ctrl Pts',(15.8812037708885,0.460285376424935,3.82667199562295));
#43409=CARTESIAN_POINT('Ctrl Pts',(15.9289196069513,0.39473215065269,4.29341396369818));
#43410=CARTESIAN_POINT('Ctrl Pts',(15.9766354430142,-0.033309682798763,
4.49070937415524));
#43411=CARTESIAN_POINT('Ctrl Pts',(16.024351279077,-0.430762722000766,4.23737881579128));
#43412=CARTESIAN_POINT('Ctrl Pts',(16.0720671151398,-0.432639725453012,
3.76605963834362));
#43413=CARTESIAN_POINT('Ctrl Pts',(16.1197829512026,-0.0372170120039125,
3.50957149464017));
#43414=CARTESIAN_POINT('Ctrl Pts',(16.1674987872655,0.392382656225717,3.70345139362117));
#43415=CARTESIAN_POINT('Ctrl Pts',(16.2152146233283,0.461651293660056,4.16965644082667));
#43416=CARTESIAN_POINT('Ctrl Pts',(16.2629304593912,0.106978444708158,4.48006336792116));
#43417=CARTESIAN_POINT('Ctrl Pts',(16.310646295454,-0.345934356094203,4.34962071752925));
#43418=CARTESIAN_POINT('Ctrl Pts',(16.3583621315169,-0.481170314810987,
3.89811598262401));
#43419=CARTESIAN_POINT('Ctrl Pts',(16.4060779675797,-0.174540169679895,
3.54017290856226));
#43420=CARTESIAN_POINT('Ctrl Pts',(16.4537938036425,0.292372898913969,3.60449612791703));
#43421=CARTESIAN_POINT('Ctrl Pts',(16.5015096397054,0.490795435699827,4.0320166386149));
#43422=CARTESIAN_POINT('Ctrl Pts',(16.5492254757682,0.238512972024049,4.4301357774334));
#43423=CARTESIAN_POINT('Ctrl Pts',(16.596941311831,-0.23279962385521,4.43325461334514));
#43424=CARTESIAN_POINT('Ctrl Pts',(16.6446571478939,-0.490328743065594,
4.03850907134293));
#43425=CARTESIAN_POINT('Ctrl Pts',(16.6923729839567,-0.297581432841348,
3.60840005658827));
#43426=CARTESIAN_POINT('Ctrl Pts',(16.7400888200196,0.168439486040012,3.53790329540825));
#43427=CARTESIAN_POINT('Ctrl Pts',(16.7878046560824,0.479779833116189,3.89175704832657));
#43428=CARTESIAN_POINT('Ctrl Pts',(16.8355204921452,0.350530977080134,4.3450119692985));
#43429=CARTESIAN_POINT('Ctrl Pts',(16.8832363282081,-0.100615868820984,
4.4814370901721));
#43430=CARTESIAN_POINT('Ctrl Pts',(16.9309521642709,-0.459365614209645,
4.17575112327883));
#43431=CARTESIAN_POINT('Ctrl Pts',(16.9786680003337,-0.396272847821079,
3.70867019559999));
#43432=CARTESIAN_POINT('Ctrl Pts',(17.0263838363966,0.0307233721630972,
3.5091219099869));
#43433=CARTESIAN_POINT('Ctrl Pts',(17.0740996724594,0.429505846750062,3.76035452756312));
#43434=CARTESIAN_POINT('Ctrl Pts',(17.1218155085223,0.433866493469502,4.23165726989771));
#43435=CARTESIAN_POINT('Ctrl Pts',(17.1695313445851,0.039800863341802,4.49022557677993));
#43436=CARTESIAN_POINT('Ctrl Pts',(17.217247180648,-0.390814512007675,4.29861219341511));
#43437=CARTESIAN_POINT('Ctrl Pts',(17.2649630167107,-0.462538907526291,
3.83277863809798));
#43438=CARTESIAN_POINT('Ctrl Pts',(17.3126788527736,-0.109506707187599,
3.52050703244687));
#43439=CARTESIAN_POINT('Ctrl Pts',(17.3603946888365,0.344087187338735,3.64856119684745));
#43440=CARTESIAN_POINT('Ctrl Pts',(17.4081105248993,0.481700523269991,4.09934702176407));
#43441=CARTESIAN_POINT('Ctrl Pts',(17.4558263609621,0.176960856767158,4.45890094794434));
#43442=CARTESIAN_POINT('Ctrl Pts',(17.503542197025,-0.290284687397741,4.39703907252861));
#43443=CARTESIAN_POINT('Ctrl Pts',(17.5512580330878,-0.490957336521241,
3.97057010757845));
#43444=CARTESIAN_POINT('Ctrl Pts',(17.5989738691507,-0.240776309167652,
3.57112706567612));
#43445=CARTESIAN_POINT('Ctrl Pts',(17.6466897052135,0.230513307714322,3.56552463842171));
#43446=CARTESIAN_POINT('Ctrl Pts',(17.6944055412763,0.490119007219086,3.95890762096741));
#43447=CARTESIAN_POINT('Ctrl Pts',(17.7421213773392,0.299640880944266,4.39002636746625));
#43448=CARTESIAN_POINT('Ctrl Pts',(17.789837213402,-0.166002076869247,4.46297789939377));
#43449=CARTESIAN_POINT('Ctrl Pts',(17.8375530494648,-0.479202773223469,
4.11076970247734));
#43450=CARTESIAN_POINT('Ctrl Pts',(17.8852688855277,-0.352344189444135,
3.65683998336499));
#43451=CARTESIAN_POINT('Ctrl Pts',(17.9329847215905,0.0980774850139738,
3.51803938772416));
#43452=CARTESIAN_POINT('Ctrl Pts',(17.9807005576534,0.458433095867658,3.82183063825345));
#43453=CARTESIAN_POINT('Ctrl Pts',(18.0284163937162,0.397802540886209,4.28923755516265));
#43454=CARTESIAN_POINT('Ctrl Pts',(18.076132229779,-0.0281362083699241,
4.49103317467411));
#43455=CARTESIAN_POINT('Ctrl Pts',(18.1238480658419,-0.428237044548737,
4.24190547436581));
#43456=CARTESIAN_POINT('Ctrl Pts',(18.1715639019047,-0.435081213444543,
3.7706322547532));
#43457=CARTESIAN_POINT('Ctrl Pts',(18.2192797379675,-0.0423836094492617,
3.50999096487715));
#43458=CARTESIAN_POINT('Ctrl Pts',(18.2669955740304,0.389235515258945,3.69933251171255));
#43459=CARTESIAN_POINT('Ctrl Pts',(18.3147114100932,0.463413677146622,4.16478163940629));
#43460=CARTESIAN_POINT('Ctrl Pts',(18.3624272461561,0.112031928774586,4.4789092521418));
#43461=CARTESIAN_POINT('Ctrl Pts',(18.4101430822189,-0.342230463623947,
4.35324712966946));
#43462=CARTESIAN_POINT('Ctrl Pts',(18.4578589182817,-0.482217355384067,
3.90319273261591));
#43463=CARTESIAN_POINT('Ctrl Pts',(18.5055747543446,-0.179376629827252,
3.54203793877243));
#43464=CARTESIAN_POINT('Ctrl Pts',(18.5532905904074,0.288188414964166,3.60143675240633));
#43465=CARTESIAN_POINT('Ctrl Pts',(18.6010064264702,0.491105603945206,4.02684232898929));
#43466=CARTESIAN_POINT('Ctrl Pts',(18.6487222625331,0.243032960192409,4.42759818183915));
#43467=CARTESIAN_POINT('Ctrl Pts',(18.6964380985959,-0.228220590447982,
4.43568404486223));
#43468=CARTESIAN_POINT('Ctrl Pts',(18.7441539346588,-0.489895661254576,
4.0436745456279));
#43469=CARTESIAN_POINT('Ctrl Pts',(18.7918697707216,-0.301692008317894,
3.6115580391236));
#43470=CARTESIAN_POINT('Ctrl Pts',(18.8395856067845,0.163560057986223,3.53615376224111));
#43471=CARTESIAN_POINT('Ctrl Pts',(18.8873014428472,0.478612406344963,3.88670662268212));
#43472=CARTESIAN_POINT('Ctrl Pts',(18.9350172789101,0.35414761756175,4.34129853476112));
#43473=CARTESIAN_POINT('Ctrl Pts',(18.982733114973,-0.0955363776958117,
4.48247075080787));
#43474=CARTESIAN_POINT('Ctrl Pts',(19.0304489510358,-0.457487847288108,
4.18058265263639));
#43475=CARTESIAN_POINT('Ctrl Pts',(19.0781647870987,-0.399321187381313,
3.71286272589862));
#43476=CARTESIAN_POINT('Ctrl Pts',(19.1258806231614,0.0255482632835279,
3.50882537619781));
#43477=CARTESIAN_POINT('Ctrl Pts',(19.1735964592243,0.426956350589889,3.75584124112414));
#43478=CARTESIAN_POINT('Ctrl Pts',(19.2213122952871,0.436283851722622,4.22707185138688));
#43479=CARTESIAN_POINT('Ctrl Pts',(19.26902813135,0.0449651784623906,4.48977888620274));
#43480=CARTESIAN_POINT('Ctrl Pts',(19.3167439674128,-0.387645709555542,
4.3027144342981));
#43481=CARTESIAN_POINT('Ctrl Pts',(19.3644598034757,-0.464275578741542,
3.8376626582024));
#43482=CARTESIAN_POINT('Ctrl Pts',(19.4121756395385,-0.114554038379521,
3.52168776344319));
#43483=CARTESIAN_POINT('Ctrl Pts',(19.4598914756013,0.340364234683876,3.64495435060606));
#43484=CARTESIAN_POINT('Ctrl Pts',(19.5076073116642,0.482720800247919,4.09426482953845));
#43485=CARTESIAN_POINT('Ctrl Pts',(19.555323147727,0.181787415268628,4.45701044834135));
#43486=CARTESIAN_POINT('Ctrl Pts',(19.6030389837899,-0.28608412753634,4.40007637198121));
#43487=CARTESIAN_POINT('Ctrl Pts',(19.6507548198527,-0.491240257057309,
3.97574594767572));
#43488=CARTESIAN_POINT('Ctrl Pts',(19.6984706559155,-0.245282818621706,
3.57368850533185));
#43489=CARTESIAN_POINT('Ctrl Pts',(19.7461864919783,0.225921452997342,3.56311925573479));
#43490=CARTESIAN_POINT('Ctrl Pts',(19.7939023280412,0.489658867576397,3.95374471702426));
#43491=CARTESIAN_POINT('Ctrl Pts',(19.841618164104,0.303734463062876,4.38684635894002));
#43492=CARTESIAN_POINT('Ctrl Pts',(19.8893340001669,-0.161112940293692,
4.46470246728215));
#43493=CARTESIAN_POINT('Ctrl Pts',(19.9370498362297,-0.47800980043334,4.11581244897344));
#43494=CARTESIAN_POINT('Ctrl Pts',(19.9847656722926,-0.355939225796451,
3.66057517601247));
#43495=CARTESIAN_POINT('Ctrl Pts',(20.0324815083554,0.0929888682922082,
3.51702731322357));
#43496=CARTESIAN_POINT('Ctrl Pts',(20.0801973444182,0.456536973876988,3.81701888067549));
#43497=CARTESIAN_POINT('Ctrl Pts',(20.1279131804811,0.400815378068436,4.28501049648274));
#43498=CARTESIAN_POINT('Ctrl Pts',(20.1756290165439,-0.022934367574535,
4.49133741301101));
#43499=CARTESIAN_POINT('Ctrl Pts',(20.2233448526067,-0.425711472830213,
4.24633918020534));
#43500=CARTESIAN_POINT('Ctrl Pts',(20.2710606886696,-0.437384262562023,
3.77535541015343));
#43501=CARTESIAN_POINT('Ctrl Pts',(20.3187765247324,-0.0477164433392854,
3.51022640082505));
#43502=CARTESIAN_POINT('Ctrl Pts',(20.3664923607953,0.386374384143037,3.69571627142296));
#43503=CARTESIAN_POINT('Ctrl Pts',(20.4062555575143,0.45143962727185,4.08165775845481));
#43504=CARTESIAN_POINT('Ctrl Pts',(20.4380661148895,0.291471375703242,4.31996082336987));
#43505=CARTESIAN_POINT('Ctrl Pts',(20.461924032921,0.103697252552815,4.42124466395835));
#43506=CARTESIAN_POINT('Ctrl Pts',(20.4857819509523,-0.111451542568667,
4.41901444157942));
#43507=CARTESIAN_POINT('Ctrl Pts',(20.5096398689838,-0.298255971346869,
4.31460392554555));
#43508=CARTESIAN_POINT('Ctrl Pts',(20.5334977870152,-0.412709509332759,
4.13311446574462));
#43509=CARTESIAN_POINT('Ctrl Pts',(20.5573557050466,-0.425936384696969,
3.91915434697803));
#43510=CARTESIAN_POINT('Ctrl Pts',(20.581213623078,-0.335173342752607,3.72492109335083));
#43511=CARTESIAN_POINT('Ctrl Pts',(20.6050715411095,-0.162364888615448,
3.59797442377207));
#43512=CARTESIAN_POINT('Ctrl Pts',(20.6289294591408,0.0501004451364318,
3.56932214892951));
#43513=CARTESIAN_POINT('Ctrl Pts',(20.6527873771723,0.250339089241223,3.64598859455508));
#43514=CARTESIAN_POINT('Ctrl Pts',(20.6766452952037,0.389350172549011,3.80921715950176));
#43515=CARTESIAN_POINT('Ctrl Pts',(20.7005032132352,0.433161330121289,4.01909908002448));
#43516=CARTESIAN_POINT('Ctrl Pts',(20.7243611312665,0.371049143609512,4.22430982617278));
#43517=CARTESIAN_POINT('Ctrl Pts',(20.748219049298,0.218207240773441,4.37467120177868));
#43518=CARTESIAN_POINT('Ctrl Pts',(20.7720769673293,0.01200671405148,4.43341500212799));
#43519=CARTESIAN_POINT('Ctrl Pts',(20.7959348853608,-0.197129246586683,
4.38617716647524));
#43520=CARTESIAN_POINT('Ctrl Pts',(20.8197928033922,-0.358062019934396,
4.24450842127602));
#43521=CARTESIAN_POINT('Ctrl Pts',(20.8436507214237,-0.431438726014498,
4.04305074550709));
#43522=CARTESIAN_POINT('Ctrl Pts',(20.867508639455,-0.399316990859146,3.83106596928302));
#43523=CARTESIAN_POINT('Ctrl Pts',(20.8913665574865,-0.269551332195825,
3.66039017609669));
#43524=CARTESIAN_POINT('Ctrl Pts',(20.9152244755179,-0.0738730526583281,
3.57275822989076));
#43525=CARTESIAN_POINT('Ctrl Pts',(20.9390823935493,0.139869212314499,3.58959853735383));
#43526=CARTESIAN_POINT('Ctrl Pts',(20.9629403115807,0.319409638666883,3.70679317993256));
#43527=CARTESIAN_POINT('Ctrl Pts',(20.9867982296122,0.420845711130686,3.8956848776653));
#43528=CARTESIAN_POINT('Ctrl Pts',(21.0106561476436,0.419373541863394,4.11008446384341));
#43529=CARTESIAN_POINT('Ctrl Pts',(21.034514065675,0.315353119032788,4.29756540021079));
#43530=CARTESIAN_POINT('Ctrl Pts',(21.0583719837064,0.134220268060588,4.41228349058099));
#43531=CARTESIAN_POINT('Ctrl Pts',(21.0822299017379,-0.079733094278782,
4.42618703719455));
#43532=CARTESIAN_POINT('Ctrl Pts',(21.1060878197692,-0.274189543318984,
4.33587624407661));
#43533=CARTESIAN_POINT('Ctrl Pts',(21.1299457378007,-0.401599180171465,
4.16343456021562));
#43534=CARTESIAN_POINT('Ctrl Pts',(21.1538036558321,-0.430806878168669,
3.95102867450389));
#43535=CARTESIAN_POINT('Ctrl Pts',(21.1776615738635,-0.354670559489406,
3.75059761183336));
#43536=CARTESIAN_POINT('Ctrl Pts',(21.2015194918949,-0.191807627993766,
3.61115222665144));
#43537=CARTESIAN_POINT('Ctrl Pts',(21.2253774099264,0.0179574932869785,
3.56679071405539));
#43538=CARTESIAN_POINT('Ctrl Pts',(21.2492353279577,0.223331518303719,3.62836067225603));
#43539=CARTESIAN_POINT('Ctrl Pts',(21.2730932459892,0.374094903668402,3.78080656934254));
#43540=CARTESIAN_POINT('Ctrl Pts',(21.2969511640206,0.433381894944723,3.98685123093373));
#43541=CARTESIAN_POINT('Ctrl Pts',(21.320809082052,0.386695207821707,4.19611112472705));
#43542=CARTESIAN_POINT('Ctrl Pts',(21.3446670000834,0.245451009020076,4.35741650656472));
#43543=CARTESIAN_POINT('Ctrl Pts',(21.3685249181149,0.0441873525619181,
4.43132381671722));
#43544=CARTESIAN_POINT('Ctrl Pts',(21.3923828361462,-0.167881315237013,
4.39976070465745));
#43545=CARTESIAN_POINT('Ctrl Pts',(21.4162407541777,-0.338898428465248,
4.27044521104599));
#43546=CARTESIAN_POINT('Ctrl Pts',(21.4400986722091,-0.427045644525908,
4.07499849655415));
#43547=CARTESIAN_POINT('Ctrl Pts',(21.4639565902406,-0.410768568010174,
3.86121260673678));
#43548=CARTESIAN_POINT('Ctrl Pts',(21.4878145082719,-0.294047387504818,
3.68136401506497));
#43549=CARTESIAN_POINT('Ctrl Pts',(21.5116724263034,-0.105423611064507,
3.57943060117972));
#43550=CARTESIAN_POINT('Ctrl Pts',(21.5355303443348,0.108979109962582,3.58033786138646));
#43551=CARTESIAN_POINT('Ctrl Pts',(21.5593882623662,0.296733470072461,3.68386394585134));
#43552=CARTESIAN_POINT('Ctrl Pts',(21.5832461803976,0.411928413892185,3.86469390692879));
#43553=CARTESIAN_POINT('Ctrl Pts',(21.6071040984291,0.426395639810567,4.07860989342611));
#43554=CARTESIAN_POINT('Ctrl Pts',(21.6309620164605,0.33659751701124,4.27330361969026));
#43555=CARTESIAN_POINT('Ctrl Pts',(21.6548199344919,0.164492132570386,4.401167166299));
#43556=CARTESIAN_POINT('Ctrl Pts',(21.6786778525233,-0.0478360589596606,
4.43093441317345));
#43557=CARTESIAN_POINT('Ctrl Pts',(21.7025357705547,-0.248467031045983,
4.35532645760922));
#43558=CARTESIAN_POINT('Ctrl Pts',(21.7263936885861,-0.388341045935521,
4.1928315042612));
#43559=CARTESIAN_POINT('Ctrl Pts',(21.7502516066176,-0.433255096896122,
3.98318399549658));
#43560=CARTESIAN_POINT('Ctrl Pts',(21.774109524649,-0.372226475033738,3.77764845789182));
#43561=CARTESIAN_POINT('Ctrl Pts',(21.7979674426804,-0.220178340780001,
3.62648392906691));
#43562=CARTESIAN_POINT('Ctrl Pts',(21.8218253607118,-0.0142906046679706,
3.56665425395863));
#43563=CARTESIAN_POINT('Ctrl Pts',(21.8456832787432,0.195091573553633,3.61278941785858));
#43564=CARTESIAN_POINT('Ctrl Pts',(21.8695411967747,0.356768547853618,3.75360811649661));
#43565=CARTESIAN_POINT('Ctrl Pts',(21.8933991148061,0.431205894023261,3.95467634223136));
#43566=CARTESIAN_POINT('Ctrl Pts',(21.9172570328375,0.400201653291494,4.16682743688221));
#43567=CARTESIAN_POINT('Ctrl Pts',(21.941114950869,0.271337207055788,4.33818467892719));
#43568=CARTESIAN_POINT('Ctrl Pts',(21.9649728689003,0.0761234226178432,
4.4268465550088));
#43569=CARTESIAN_POINT('Ctrl Pts',(21.9888307869318,-0.137704612210607,
4.41113282132402));
#43570=CARTESIAN_POINT('Ctrl Pts',(22.0126887049632,-0.317860118355158,
4.29488591379237));
#43571=CARTESIAN_POINT('Ctrl Pts',(22.0365466229946,-0.420290167226249,
4.10653136780738));
#43572=CARTESIAN_POINT('Ctrl Pts',(22.060404541026,-0.419947821735935,3.89212700053744));
#43573=CARTESIAN_POINT('Ctrl Pts',(22.0842624590574,-0.316916794682727,
3.70410052003731));
#43574=CARTESIAN_POINT('Ctrl Pts',(22.1081203770888,-0.136390978688423,
3.58842952252864));
#43575=CARTESIAN_POINT('Ctrl Pts',(22.1319782951203,0.0774861468089536,
3.57339871771534));
#43576=CARTESIAN_POINT('Ctrl Pts',(22.1558362131517,0.27241579873489,3.66268354680831));
#43577=CARTESIAN_POINT('Ctrl Pts',(22.1796941311831,0.400732367405962,3.83445143701846));
#43578=CARTESIAN_POINT('Ctrl Pts',(22.2035520492145,0.431058956528623,4.04670046033727));
#43579=CARTESIAN_POINT('Ctrl Pts',(22.227409967246,0.355979888945518,4.24752994899471));
#43580=CARTESIAN_POINT('Ctrl Pts',(22.2512678852773,0.193854041863619,4.38783162256878));
#43581=CARTESIAN_POINT('Ctrl Pts',(22.2751258033088,-0.0156743990186396,
4.43329790005389));
#43582=CARTESIAN_POINT('Ctrl Pts',(22.2989837213402,-0.221370022215225,
4.37281103827166));
#43583=CARTESIAN_POINT('Ctrl Pts',(22.3228416393716,-0.372934645290675,
4.22116172228637));
#43584=CARTESIAN_POINT('Ctrl Pts',(22.346699557403,-0.43330658847365,4.01543234121164));
#43585=CARTESIAN_POINT('Ctrl Pts',(22.3705574754345,-0.387723268841402,
3.80592933171158));
#43586=CARTESIAN_POINT('Ctrl Pts',(22.3944153934659,-0.247331046528593,
3.64388188817752));
#43587=CARTESIAN_POINT('Ctrl Pts',(22.4182733114973,-0.0464596501027702,
3.56891502119853));
#43588=CARTESIAN_POINT('Ctrl Pts',(22.4421312295287,0.165772403721094,3.59936017830047));
#43589=CARTESIAN_POINT('Ctrl Pts',(22.4659891475602,0.337468575289321,3.7277726770023));
#43590=CARTESIAN_POINT('Ctrl Pts',(22.4898470655915,0.426644514167594,3.92275218663495));
#43591=CARTESIAN_POINT('Ctrl Pts',(22.513704983623,0.411494197867752,4.13662086224655));
#43592=CARTESIAN_POINT('Ctrl Pts',(22.5375629016544,0.295722435535401,4.31708206952049));
#43593=CARTESIAN_POINT('Ctrl Pts',(22.5614208196858,0.107638304484935,4.42000797176855));
#43594=CARTESIAN_POINT('Ctrl Pts',(22.5852787377172,-0.106765988085903,
4.42023067651324));
#43595=CARTESIAN_POINT('Ctrl Pts',(22.6091366557487,-0.295063722636797,
4.31769517074077));
#43596=CARTESIAN_POINT('Ctrl Pts',(22.6329945737801,-0.411209141905604,
4.13747522778479));
#43597=CARTESIAN_POINT('Ctrl Pts',(22.6568524918115,-0.426804986482714,
3.92363755172126));
#43598=CARTESIAN_POINT('Ctrl Pts',(22.6807104098429,-0.33803111495158,3.72847502015617));
#43599=CARTESIAN_POINT('Ctrl Pts',(22.7045683278743,-0.16660749730952,3.59970312177549));
#43600=CARTESIAN_POINT('Ctrl Pts',(22.7284262459057,0.0455714674079685,
3.56882345794434));
#43601=CARTESIAN_POINT('Ctrl Pts',(22.7522841639372,0.246577802732478,3.64336153500176));
#43602=CARTESIAN_POINT('Ctrl Pts',(22.7761420819686,0.387346815298129,3.80514019809748));
#43603=CARTESIAN_POINT('Ctrl Pts',(22.7920473606562,0.417963038852713,3.94471011778788));
#43604=CARTESIAN_POINT('Ctrl Pts',(22.8,0.415641328671541,4.01393920819689));
#43605=CARTESIAN_POINT('Ctrl Pts',(3.96816317011929,0.203757107801821,4.42939176513376));
#43606=CARTESIAN_POINT('Ctrl Pts',(3.9761158094631,0.132237748973037,4.46332948562603));
#43607=CARTESIAN_POINT('Ctrl Pts',(3.99202108815071,-0.0280119004087947,
4.49474661085258));
#43608=CARTESIAN_POINT('Ctrl Pts',(4.01587900618213,-0.261670681609628,
4.42079217330492));
#43609=CARTESIAN_POINT('Ctrl Pts',(4.03973692421355,-0.431283260509235,
4.24398813071681));
#43610=CARTESIAN_POINT('Ctrl Pts',(4.06359484224497,-0.495466080430727,
4.00749935521381));
#43611=CARTESIAN_POINT('Ctrl Pts',(4.08745276027639,-0.438477829352452,
3.76918881818141));
#43612=CARTESIAN_POINT('Ctrl Pts',(4.11131067830781,-0.274278321106756,
3.5873115455631));
#43613=CARTESIAN_POINT('Ctrl Pts',(4.13516859633923,-0.0430057845205295,
3.50635120590702));
#43614=CARTESIAN_POINT('Ctrl Pts',(4.15902651437064,0.198780450874126,3.54609966156282));
#43615=CARTESIAN_POINT('Ctrl Pts',(4.18288443240206,0.391960715466274,3.69684005745713));
#43616=CARTESIAN_POINT('Ctrl Pts',(4.20674235043348,0.489295238859844,3.92171081754005));
#43617=CARTESIAN_POINT('Ctrl Pts',(4.2306002684649,0.466984102771714,4.16572567991789));
#43618=CARTESIAN_POINT('Ctrl Pts',(4.25445818649632,0.330482445391075,4.36921595913043));
#43619=CARTESIAN_POINT('Ctrl Pts',(4.27831610452774,0.113168927396708,4.48242295331799));
#43620=CARTESIAN_POINT('Ctrl Pts',(4.30217402255916,-0.131817528672551,
4.47766435517297));
#43621=CARTESIAN_POINT('Ctrl Pts',(4.32603194059057,-0.344570980451485,
4.35610383169054));
#43622=CARTESIAN_POINT('Ctrl Pts',(4.349889858622,-0.473067456356951,4.14746621026076));
#43623=CARTESIAN_POINT('Ctrl Pts',(4.37374777665341,-0.485886045261059,
3.9027690893624));
#43624=CARTESIAN_POINT('Ctrl Pts',(4.39760569468484,-0.379892264971952,
3.68184757153936));
#43625=CARTESIAN_POINT('Ctrl Pts',(4.42146361271625,-0.181004475645389,
3.53872299041084));
#43626=CARTESIAN_POINT('Ctrl Pts',(4.44532153074767,0.0621438372772935,
3.50839320219298));
#43627=CARTESIAN_POINT('Ctrl Pts',(4.46917944877909,0.290096289836991,3.5982746675986));
#43628=CARTESIAN_POINT('Ctrl Pts',(4.49303736681051,0.447112297141319,3.78638891931142));
#43629=CARTESIAN_POINT('Ctrl Pts',(4.51689528484194,0.494797168872773,4.02673689903048));
#43630=CARTESIAN_POINT('Ctrl Pts',(4.54075320287334,0.421490654719143,4.26054697856981));
#43631=CARTESIAN_POINT('Ctrl Pts',(4.56461112090478,0.245118194360182,4.43064622472778));
#43632=CARTESIAN_POINT('Ctrl Pts',(4.58846903893618,0.00880765856895839,
4.49544073835303));
#43633=CARTESIAN_POINT('Ctrl Pts',(4.61232695696761,-0.229656589644598,
4.43908649592634));
#43634=CARTESIAN_POINT('Ctrl Pts',(4.63618487499902,-0.411963545977342,
4.2753636447643));
#43635=CARTESIAN_POINT('Ctrl Pts',(4.66004279303045,-0.493534193653132,
4.04430688170513));
#43636=CARTESIAN_POINT('Ctrl Pts',(4.68390071106186,-0.454422287381232,
3.80241587917234));
#43637=CARTESIAN_POINT('Ctrl Pts',(4.70775862909328,-0.304191753628974,
3.60883957626609));
#43638=CARTESIAN_POINT('Ctrl Pts',(4.7316165471247,-0.0795780500979935,
3.51091265195837));
#43639=CARTESIAN_POINT('Ctrl Pts',(4.75547446515612,0.164494654344808,3.53258090671894));
#43640=CARTESIAN_POINT('Ctrl Pts',(4.77933238318754,0.368343935055725,3.66854586202706));
#43641=CARTESIAN_POINT('Ctrl Pts',(4.80319030121895,0.482123090158262,3.88556038269908));
#43642=CARTESIAN_POINT('Ctrl Pts',(4.82704821925038,0.478010016947761,4.13055850707372));
#43643=CARTESIAN_POINT('Ctrl Pts',(4.85090613728179,0.357010473862124,4.34363152012653));
#43644=CARTESIAN_POINT('Ctrl Pts',(4.87476405531322,0.14871214514713,4.47267726617372));
#43645=CARTESIAN_POINT('Ctrl Pts',(4.89862197334463,-0.0959503538938319,
4.48614054517122));
#43646=CARTESIAN_POINT('Ctrl Pts',(4.92247989137606,-0.317150377772593,
4.38072921867179));
#43647=CARTESIAN_POINT('Ctrl Pts',(4.94633780940747,-0.460798495283114,
4.1822192273514));
#43648=CARTESIAN_POINT('Ctrl Pts',(4.97019572743889,-0.49176882879792,3.93915167139151));
#43649=CARTESIAN_POINT('Ctrl Pts',(4.99405364547031,-0.40248828815769,3.71096318925158));
#43650=CARTESIAN_POINT('Ctrl Pts',(5.01791156350173,-0.214788397502062,
3.55345208054429));
#43651=CARTESIAN_POINT('Ctrl Pts',(5.04176948153314,0.0254331070612992,
3.50513410186502));
#43652=CARTESIAN_POINT('Ctrl Pts',(5.06562739956457,0.259435524164246,3.57782431515618));
#43653=CARTESIAN_POINT('Ctrl Pts',(5.08948531759598,0.429998888727244,3.75374798322641));
#43654=CARTESIAN_POINT('Ctrl Pts',(5.11334323562741,0.495415812061873,3.98988697716804));
#43655=CARTESIAN_POINT('Ctrl Pts',(5.13720115365882,0.439690074491602,4.2284988806653));
#43656=CARTESIAN_POINT('Ctrl Pts',(5.16105907169025,0.276448136790977,4.41123658365534));
#43657=CARTESIAN_POINT('Ctrl Pts',(5.18491698972166,0.0456070993489057,
4.49341574008204));
#43658=CARTESIAN_POINT('Ctrl Pts',(5.20877490775308,-0.196386116196418,
4.45494130768376));
#43659=CARTESIAN_POINT('Ctrl Pts',(5.2326328257845,-0.390357576881318,4.3052213332044));
#43660=CARTESIAN_POINT('Ctrl Pts',(5.25649074381592,-0.488875976891831,
4.08086642869437));
#43661=CARTESIAN_POINT('Ctrl Pts',(5.28034866184734,-0.467850883838054,
3.83673747961128));
#43662=CARTESIAN_POINT('Ctrl Pts',(5.30420657987876,-0.332423505683668,
3.632530663945));
#43663=CARTESIAN_POINT('Ctrl Pts',(5.32806449791017,-0.115709525355139,
3.5181801106079));
#43664=CARTESIAN_POINT('Ctrl Pts',(5.3519224159416,0.129298585786916,3.52164764473745));
#43665=CARTESIAN_POINT('Ctrl Pts',(5.37578033397301,0.342689670681295,3.64208535978523));
#43666=CARTESIAN_POINT('Ctrl Pts',(5.39963825200445,0.472283796414913,3.85004295376459));
#43667=CARTESIAN_POINT('Ctrl Pts',(5.42349617003584,0.48639166917272,4.09466913029638));
#43668=CARTESIAN_POINT('Ctrl Pts',(5.44735408806728,0.381563529774833,4.31614612573549));
#43669=CARTESIAN_POINT('Ctrl Pts',(5.47121200609869,0.183432713764955,4.46031678178449));
#43670=CARTESIAN_POINT('Ctrl Pts',(5.49506992413012,-0.059552397366927,
4.49192744591021));
#43671=CARTESIAN_POINT('Ctrl Pts',(5.51892784216153,-0.287975325168481,
4.40324844967551));
#43672=CARTESIAN_POINT('Ctrl Pts',(5.54278576019295,-0.445980441674811,
4.21596422322942));
#43673=CARTESIAN_POINT('Ctrl Pts',(5.56664367822437,-0.494931191930538,
3.97587086145358));
#43674=CARTESIAN_POINT('Ctrl Pts',(5.59050159625579,-0.422857784100094,
3.74167773132221));
#43675=CARTESIAN_POINT('Ctrl Pts',(5.61435951428721,-0.247384129650275,
3.57065143242979));
#43676=CARTESIAN_POINT('Ctrl Pts',(5.63821743231862,-0.0114183168777074,
3.50461255354752));
#43677=CARTESIAN_POINT('Ctrl Pts',(5.66207535035005,0.227339585372105,3.55970939936999));
#43678=CARTESIAN_POINT('Ctrl Pts',(5.68593326838146,0.410506766445453,3.72246929038963));
#43679=CARTESIAN_POINT('Ctrl Pts',(5.70979118641288,0.493293861043031,3.9530929995654));
#43680=CARTESIAN_POINT('Ctrl Pts',(5.73364910444431,0.455457169749513,4.19518674831082));
#43681=CARTESIAN_POINT('Ctrl Pts',(5.75750702247572,0.306248793691327,4.38955201985635));
#43682=CARTESIAN_POINT('Ctrl Pts',(5.78136494050715,0.0821542461994931,
4.48866121222712));
#43683=CARTESIAN_POINT('Ctrl Pts',(5.80522285853855,-0.162029253596618,
4.46827942571263));
#43684=CARTESIAN_POINT('Ctrl Pts',(5.82908077656998,-0.366592184898752,
4.33339056701663));
#43685=CARTESIAN_POINT('Ctrl Pts',(5.85293869460139,-0.481513345756758,
4.11697862749145));
#43686=CARTESIAN_POINT('Ctrl Pts',(5.87679661263282,-0.478691368855474,
3.87196223809426));
#43687=CARTESIAN_POINT('Ctrl Pts',(5.90065453066423,-0.358816329143926,
3.65825454842257));
#43688=CARTESIAN_POINT('Ctrl Pts',(5.92451244869565,-0.151200892471453,
3.52811296978032));
#43689=CARTESIAN_POINT('Ctrl Pts',(5.94837036672708,0.093387223403125,3.5133605500302));
#43690=CARTESIAN_POINT('Ctrl Pts',(5.97222828475848,0.315139728168714,3.61760487120619));
#43691=CARTESIAN_POINT('Ctrl Pts',(5.99608620278992,0.459831779670103,3.81535495398299));
#43692=CARTESIAN_POINT('Ctrl Pts',(6.01994412082132,0.492082823488737,4.05825627791571));
#43693=CARTESIAN_POINT('Ctrl Pts',(6.04380203885276,0.404005480250355,4.28691141512903));
#43694=CARTESIAN_POINT('Ctrl Pts',(6.06765995688416,0.21713917558903,4.44541067075535));
#43695=CARTESIAN_POINT('Ctrl Pts',(6.09151787491559,-0.0228261843714051,
4.49499153360272));
#43696=CARTESIAN_POINT('Ctrl Pts',(6.11537579294701,-0.257204988275768,
4.42353981062321));
#43697=CARTESIAN_POINT('Ctrl Pts',(6.13923371097843,-0.428699479426561,
4.24850911946619));
#43698=CARTESIAN_POINT('Ctrl Pts',(6.16309162900984,-0.49534768549136,4.01273373861842));
#43699=CARTESIAN_POINT('Ctrl Pts',(6.18694954704127,-0.440903093044182,
3.77380201544612));
#43700=CARTESIAN_POINT('Ctrl Pts',(6.21080746507268,-0.278582990390117,
3.59026229064107));
#43701=CARTESIAN_POINT('Ctrl Pts',(6.23466538310411,-0.048260127889517,
3.50676273730504));
#43702=CARTESIAN_POINT('Ctrl Pts',(6.25852330113552,0.194087080856728,3.5441598063702));
#43703=CARTESIAN_POINT('Ctrl Pts',(6.28238121916694,0.388553448942855,3.69248145192407));
#43704=CARTESIAN_POINT('Ctrl Pts',(6.30623913719837,0.488798280742691,3.9170164641697));
#43705=CARTESIAN_POINT('Ctrl Pts',(6.33009705522977,0.468067515948433,4.15995908608738));
#43706=CARTESIAN_POINT('Ctrl Pts',(6.36190761260502,0.291040001689194,4.43610431491443));
#43707=CARTESIAN_POINT('Ctrl Pts',(6.40167080932402,-0.143168317426403,
4.54352222151223));
#43708=CARTESIAN_POINT('Ctrl Pts',(6.44938664538688,-0.535165231989368,
4.17285582464912));
#43709=CARTESIAN_POINT('Ctrl Pts',(6.49710248144971,-0.434543251113388,
3.64369891234367));
#43710=CARTESIAN_POINT('Ctrl Pts',(6.54481831751255,0.0645215567551043,
3.4416075490323));
#43711=CARTESIAN_POINT('Ctrl Pts',(6.59253415357539,0.504653900644641,3.75236619672659));
#43712=CARTESIAN_POINT('Ctrl Pts',(6.64024998963822,0.481186238846835,4.29049388273239));
#43713=CARTESIAN_POINT('Ctrl Pts',(6.68796582570107,0.01592709648968,4.56187610740764));
#43714=CARTESIAN_POINT('Ctrl Pts',(6.7356816617639,-0.464005405879062,4.31726850783359));
#43715=CARTESIAN_POINT('Ctrl Pts',(6.78339749782674,-0.517809574500644,
3.78131383674221));
#43716=CARTESIAN_POINT('Ctrl Pts',(6.83111333388957,-0.0961144992151805,
3.44617913151078));
#43717=CARTESIAN_POINT('Ctrl Pts',(6.87882916995242,0.413851019972934,3.61962818876606));
#43718=CARTESIAN_POINT('Ctrl Pts',(6.92654500601525,0.543767061592725,4.14237771887731));
#43719=CARTESIAN_POINT('Ctrl Pts',(6.97426084207809,0.174335412693353,4.53438003016987));
#43720=CARTESIAN_POINT('Ctrl Pts',(7.02197667814094,-0.355192171006393,
4.43565270890428));
#43721=CARTESIAN_POINT('Ctrl Pts',(7.06969251420376,-0.558540766450571,
3.93685892261342));
#43722=CARTESIAN_POINT('Ctrl Pts',(7.11740835026661,-0.248973074301851,
3.49604849518665));
#43723=CARTESIAN_POINT('Ctrl Pts',(7.16512418632944,0.289230577826905,3.51802452284194));
#43724=CARTESIAN_POINT('Ctrl Pts',(7.21284002239229,0.561829257914175,3.98260602935256));
#43725=CARTESIAN_POINT('Ctrl Pts',(7.26055585845511,0.318491529052478,4.46316069626365));
#43726=CARTESIAN_POINT('Ctrl Pts',(7.30827169451797,-0.217321894570402,
4.51838776411367));
#43727=CARTESIAN_POINT('Ctrl Pts',(7.35598753058078,-0.553565266295818,
4.09757137442565));
#43728=CARTESIAN_POINT('Ctrl Pts',(7.40370336664365,-0.381461142739227,
3.58715368886071));
#43729=CARTESIAN_POINT('Ctrl Pts',(7.45141920270646,0.140944621146953,3.45585912402047));
#43730=CARTESIAN_POINT('Ctrl Pts',(7.49913503876933,0.533918768911932,3.82425749787944));
#43731=CARTESIAN_POINT('Ctrl Pts',(7.54685087483214,0.436587096747522,4.3540429157916));
#43732=CARTESIAN_POINT('Ctrl Pts',(7.594566710895,-0.0616692246238245,4.5587052763707));
#43733=CARTESIAN_POINT('Ctrl Pts',(7.64228254695782,-0.503293747851232,
4.25029998493175));
#43734=CARTESIAN_POINT('Ctrl Pts',(7.68999838302067,-0.482735878399531,
3.7120403659385));
#43735=CARTESIAN_POINT('Ctrl Pts',(7.7377142190835,-0.0188742238918736,
3.43821850974892));
#43736=CARTESIAN_POINT('Ctrl Pts',(7.78543005514633,0.462319920793015,3.6802892401675));
#43737=CARTESIAN_POINT('Ctrl Pts',(7.83314589120918,0.518958568528469,4.21595528072725));
#43738=CARTESIAN_POINT('Ctrl Pts',(7.88086172727202,0.099029577569048,4.55330626409362));
#43739=CARTESIAN_POINT('Ctrl Pts',(7.92857756333485,-0.411839798232008,
4.38254759143289));
#43740=CARTESIAN_POINT('Ctrl Pts',(7.9762933993977,-0.544510350349916,3.86048957930736));
#43741=CARTESIAN_POINT('Ctrl Pts',(8.02400923546053,-0.177148669371157,
3.466546133148));
#43742=CARTESIAN_POINT('Ctrl Pts',(8.07172507152338,0.352891360472903,3.56248158116143));
#43743=CARTESIAN_POINT('Ctrl Pts',(8.1194409075862,0.558865824063627,4.06019692528064));
#43744=CARTESIAN_POINT('Ctrl Pts',(8.16715674364906,0.251625202160443,4.50263250666582));
#43745=CARTESIAN_POINT('Ctrl Pts',(8.21487257971187,-0.286686714637947,
4.48349292318459));
#43746=CARTESIAN_POINT('Ctrl Pts',(8.26258841577472,-0.561729810142263,
4.02035434884804));
#43747=CARTESIAN_POINT('Ctrl Pts',(8.31030425183756,-0.32092777766878,3.53852406277244));
#43748=CARTESIAN_POINT('Ctrl Pts',(8.3580200879004,0.21458717114652,3.4804742305729));
#43749=CARTESIAN_POINT('Ctrl Pts',(8.40573592396324,0.553043418849938,3.89951290636976));
#43750=CARTESIAN_POINT('Ctrl Pts',(8.45345176002607,0.383631385356639,4.41083042643994));
#43751=CARTESIAN_POINT('Ctrl Pts',(8.50116759608892,-0.13807525223727,4.54487604447167));
#43752=CARTESIAN_POINT('Ctrl Pts',(8.54888343215175,-0.532985261140852,
4.17855360686946));
#43753=CARTESIAN_POINT('Ctrl Pts',(8.59659926821459,-0.43844670370641,3.64826264467864));
#43754=CARTESIAN_POINT('Ctrl Pts',(8.64431510427743,0.0587242081113278,
3.4409775080543));
#43755=CARTESIAN_POINT('Ctrl Pts',(8.69203094034026,0.501967776032349,3.74705132745037));
#43756=CARTESIAN_POINT('Ctrl Pts',(8.73974677640311,0.484246611455832,4.28541180496438));
#43757=CARTESIAN_POINT('Ctrl Pts',(8.78746261246592,0.021834332487559,4.56167423035448));
#43758=CARTESIAN_POINT('Ctrl Pts',(8.83517844852879,-0.460628749968427,
4.32214256754115));
#43759=CARTESIAN_POINT('Ctrl Pts',(8.88289428459161,-0.520089363644054,
3.78678242815423));
#43760=CARTESIAN_POINT('Ctrl Pts',(8.93061012065447,-0.101943912081849,
3.44722326576734));
#43761=CARTESIAN_POINT('Ctrl Pts',(8.97832595671729,0.409818202553832,3.61528748398963));
#43762=CARTESIAN_POINT('Ctrl Pts',(9.02604179278014,0.545237955920739,4.1366391252272));
#43763=CARTESIAN_POINT('Ctrl Pts',(9.07375762884296,0.179957304801303,4.53251295530543));
#43764=CARTESIAN_POINT('Ctrl Pts',(9.12147346490582,-0.350580908316224,
4.43937194476168));
#43765=CARTESIAN_POINT('Ctrl Pts',(9.16918930096864,-0.559175278946307,
3.94274891673689));
#43766=CARTESIAN_POINT('Ctrl Pts',(9.21690513703149,-0.254270386902387,
3.49870043939378));
#43767=CARTESIAN_POINT('Ctrl Pts',(9.26462097309432,0.284134913886797,3.51500306204057));
#43768=CARTESIAN_POINT('Ctrl Pts',(9.31233680915716,0.56161475127612,3.97668583545263));
#43769=CARTESIAN_POINT('Ctrl Pts',(9.36005264522,0.323355121014866,4.45977836490307));
#43770=CARTESIAN_POINT('Ctrl Pts',(9.40776848128284,-0.211846492332409,
4.52064934726353));
#43771=CARTESIAN_POINT('Ctrl Pts',(9.45548431734568,-0.552506212093558,
4.10340002281193));
#43772=CARTESIAN_POINT('Ctrl Pts',(9.50320015340851,-0.385790975888367,
3.59119686639829));
#43773=CARTESIAN_POINT('Ctrl Pts',(9.55091598947136,0.135202049632292,3.45440391781584));
#43774=CARTESIAN_POINT('Ctrl Pts',(9.59863182553417,0.532036952624682,3.81864024657791));
#43775=CARTESIAN_POINT('Ctrl Pts',(9.64634766159704,0.440294135581046,4.34942202748599));
#43776=CARTESIAN_POINT('Ctrl Pts',(9.69406349765985,-0.0557775609627595,
4.55932418400469));
#43777=CARTESIAN_POINT('Ctrl Pts',(9.74177933372271,-0.500627865026369,
4.25559033604309));
#43778=CARTESIAN_POINT('Ctrl Pts',(9.78949516978553,-0.485743897486414,
3.71714394973028));
#43779=CARTESIAN_POINT('Ctrl Pts',(9.83721100584839,-0.0247938347541151,
3.43844862667992));
#43780=CARTESIAN_POINT('Ctrl Pts',(9.88492684191122,0.458924787935076,3.67543457032792));
#43781=CARTESIAN_POINT('Ctrl Pts',(9.93264267797406,0.521205716397956,4.21047394212484));
#43782=CARTESIAN_POINT('Ctrl Pts',(9.98035851403688,0.104855415711801,4.55223185431066));
#43783=CARTESIAN_POINT('Ctrl Pts',(10.0280743500997,-0.407785226630454,
4.3868667575037));
#43784=CARTESIAN_POINT('Ctrl Pts',(10.0757901861625,-0.54595042077573,3.86623596457089));
#43785=CARTESIAN_POINT('Ctrl Pts',(10.1235060222254,-0.182760942995651,
3.46844274359687));
#43786=CARTESIAN_POINT('Ctrl Pts',(10.1712218582882,0.34826072087591,3.55878673023755));
#43787=CARTESIAN_POINT('Ctrl Pts',(10.2189376943511,0.559469206087141,4.05430365143988));
#43788=CARTESIAN_POINT('Ctrl Pts',(10.2666535304139,0.256908510808291,4.49995269395588));
#43789=CARTESIAN_POINT('Ctrl Pts',(10.3143693664768,-0.281575222991369,
4.4864874848512));
#43790=CARTESIAN_POINT('Ctrl Pts',(10.3620852025396,-0.561484096926345,
4.02627333283551));
#43791=CARTESIAN_POINT('Ctrl Pts',(10.4098010386024,-0.325773485110519,
3.5419319750098));
#43792=CARTESIAN_POINT('Ctrl Pts',(10.4575168746653,0.209099930751681,3.47824153281512));
#43793=CARTESIAN_POINT('Ctrl Pts',(10.5052327107281,0.55195366278862,3.89368991932227));
#43794=CARTESIAN_POINT('Ctrl Pts',(10.552948546791,0.387939853388008,4.40676448870664));
#43795=CARTESIAN_POINT('Ctrl Pts',(10.6006643828538,-0.13232509260073,4.54630096923553));
#43796=CARTESIAN_POINT('Ctrl Pts',(10.6483802189166,-0.531073869970951,
4.18416086379456));
#43797=CARTESIAN_POINT('Ctrl Pts',(10.6960960549795,-0.442129340924997,
3.6529030034519));
#43798=CARTESIAN_POINT('Ctrl Pts',(10.7438118910423,0.0528293649267388,
3.44038965581316));
#43799=CARTESIAN_POINT('Ctrl Pts',(10.7915277271051,0.499274052081986,3.74177509795313));
#43800=CARTESIAN_POINT('Ctrl Pts',(10.839243563168,0.487227694891584,4.28029244094358));
#43801=CARTESIAN_POINT('Ctrl Pts',(10.8869593992308,0.0277526485205102,
4.56141292256198));
#43802=CARTESIAN_POINT('Ctrl Pts',(10.9346752352937,-0.457208082016334,
4.32697927894352));
#43803=CARTESIAN_POINT('Ctrl Pts',(10.9823910713565,-0.522307595786967,
3.79227553224832));
#43804=CARTESIAN_POINT('Ctrl Pts',(11.0301069074193,-0.107764007611043,
3.44832836054127));
#43805=CARTESIAN_POINT('Ctrl Pts',(11.0778227434822,0.405740926916492,3.61098974390844));
#43806=CARTESIAN_POINT('Ctrl Pts',(11.125538579545,0.54664772512998,4.13088523113667));
#43807=CARTESIAN_POINT('Ctrl Pts',(11.1732544156078,0.185559506100192,4.53058679668394));
#43808=CARTESIAN_POINT('Ctrl Pts',(11.2209702516707,-0.345930862581405,
4.4430423427091));
#43809=CARTESIAN_POINT('Ctrl Pts',(11.2686860877335,-0.559747597323992,
3.94864528834179));
#43810=CARTESIAN_POINT('Ctrl Pts',(11.3164019237964,-0.259539500620097,
3.50140805588402));
#43811=CARTESIAN_POINT('Ctrl Pts',(11.3641177598592,0.279007713031768,3.51203547753114));
#43812=CARTESIAN_POINT('Ctrl Pts',(11.411833595922,0.561337850721073,3.97076822846069));
#43813=CARTESIAN_POINT('Ctrl Pts',(11.4595494319849,0.328182802800164,4.45634496498341));
#43814=CARTESIAN_POINT('Ctrl Pts',(11.5072652680477,-0.206347562673641,
4.52285309839201));
#43815=CARTESIAN_POINT('Ctrl Pts',(11.5549811041106,-0.551385786278872,
4.10921718641821));
#43816=CARTESIAN_POINT('Ctrl Pts',(11.6026969401734,-0.390077958183356,
3.59528545163414));
#43817=CARTESIAN_POINT('Ctrl Pts',(11.6504127762362,0.129444461032819,3.45300931394821));
#43818=CARTESIAN_POINT('Ctrl Pts',(11.6981286122991,0.530096039923511,3.8130431397972));
#43819=CARTESIAN_POINT('Ctrl Pts',(11.7458444483619,0.443952268776438,4.34476232707146));
#43820=CARTESIAN_POINT('Ctrl Pts',(11.7935602844247,-0.0498797018717475,
4.55988096454574));
#43821=CARTESIAN_POINT('Ctrl Pts',(11.8412761204876,-0.497906374793238,
4.26085229740167));
#43822=CARTESIAN_POINT('Ctrl Pts',(11.8889919565504,-0.48869796246776,3.72227895182515));
#43823=CARTESIAN_POINT('Ctrl Pts',(11.9367077926133,-0.0307106916234339,
3.43874111807518));
#43824=CARTESIAN_POINT('Ctrl Pts',(11.9844236286761,0.455478679883424,3.67061595167475));
#43825=CARTESIAN_POINT('Ctrl Pts',(12.0321394647389,0.523394971212992,4.20496922507643));
#43826=CARTESIAN_POINT('Ctrl Pts',(12.0798553008018,0.110669607010866,4.5510961052335));
#43827=CARTESIAN_POINT('Ctrl Pts',(12.1275711368646,-0.403685360180124,
4.39114295225112));
#43828=CARTESIAN_POINT('Ctrl Pts',(12.1752869729274,-0.547329849620031,
3.8719972077086));
#43829=CARTESIAN_POINT('Ctrl Pts',(12.2230028089903,-0.188352916401613,
3.4703983969034));
#43830=CARTESIAN_POINT('Ctrl Pts',(12.2707186450531,0.34359139813055,3.55514088718992));
#43831=CARTESIAN_POINT('Ctrl Pts',(12.318434481116,0.560010444926212,4.04840434580723));
#43832=CARTESIAN_POINT('Ctrl Pts',(12.3661503171788,0.262163283277844,4.49721734887317));
#43833=CARTESIAN_POINT('Ctrl Pts',(12.4138661532417,-0.276432455305192,
4.48942800979656));
#43834=CARTESIAN_POINT('Ctrl Pts',(12.4615819893045,-0.561176016721412,
4.03218939850585));
#43835=CARTESIAN_POINT('Ctrl Pts',(12.5092978253673,-0.330583007179444,
3.54539076726965));
#43836=CARTESIAN_POINT('Ctrl Pts',(12.5570136614301,0.203589464528802,3.47606678951191));
#43837=CARTESIAN_POINT('Ctrl Pts',(12.604729497493,0.550802598333678,3.88787874069406));
#43838=CARTESIAN_POINT('Ctrl Pts',(12.6524453335558,0.392205230901379,4.40265336950419));
#43839=CARTESIAN_POINT('Ctrl Pts',(12.7001611696187,-0.126560234920843,
4.54766521348015));
#43840=CARTESIAN_POINT('Ctrl Pts',(12.7478770056815,-0.529103489635726,
4.18974766500481));
#43841=CARTESIAN_POINT('Ctrl Pts',(12.7955928417443,-0.44576286851447,3.65758191611243));
#43842=CARTESIAN_POINT('Ctrl Pts',(12.8433086778072,0.0469286537069902,
3.43986396243348));
#43843=CARTESIAN_POINT('Ctrl Pts',(12.89102451387,0.496524871139168,3.73652755085263));
#43844=CARTESIAN_POINT('Ctrl Pts',(12.9387403499328,0.490154659387074,4.27514194336855));
#43845=CARTESIAN_POINT('Ctrl Pts',(12.9864561859957,0.0336678819209607,
4.56108925568614));
#43846=CARTESIAN_POINT('Ctrl Pts',(13.0341720220585,-0.45373662956012,4.33177967103923));
#43847=CARTESIAN_POINT('Ctrl Pts',(13.0818878581214,-0.524467812480695,
3.79779170939055));
#43848=CARTESIAN_POINT('Ctrl Pts',(13.1296036941842,-0.113572133225654,
3.44949473238301));
#43849=CARTESIAN_POINT('Ctrl Pts',(13.177319530247,0.401618583502394,3.60673521324049));
#43850=CARTESIAN_POINT('Ctrl Pts',(13.2250353663099,0.547996775303968,4.12511679893576));
#43851=CARTESIAN_POINT('Ctrl Pts',(13.2727512023727,0.191141096329688,4.52860170299893));
#43852=CARTESIAN_POINT('Ctrl Pts',(13.3204670384356,-0.341242392487953,
4.4466635296155));
#43853=CARTESIAN_POINT('Ctrl Pts',(13.3681828744984,-0.560257741594785,
3.95454736418435));
#43854=CARTESIAN_POINT('Ctrl Pts',(13.4158987105612,-0.264779785921688,
3.5041710536014));
#43855=CARTESIAN_POINT('Ctrl Pts',(13.4636145466241,0.273849521323983,3.50912209380529));
#43856=CARTESIAN_POINT('Ctrl Pts',(13.5113303826869,0.560998599421335,3.96485386839523));
#43857=CARTESIAN_POINT('Ctrl Pts',(13.5590462187498,0.332974031597074,4.45286087643057));
#43858=CARTESIAN_POINT('Ctrl Pts',(13.6067620548126,-0.200825712906817,
4.52499877347948));
#43859=CARTESIAN_POINT('Ctrl Pts',(13.6544778908754,-0.550204115147588,
4.11502221869768));
#43860=CARTESIAN_POINT('Ctrl Pts',(13.7021937269383,-0.394321612469819,
3.5994189906415));
#43861=CARTESIAN_POINT('Ctrl Pts',(13.7499095630011,0.123672494356884,3.45167546721031));
#43862=CARTESIAN_POINT('Ctrl Pts',(13.7976253990639,0.528096246669736,3.80746679929733));
#43863=CARTESIAN_POINT('Ctrl Pts',(13.8453412351268,0.44756108986054,4.34006433209368));
#43864=CARTESIAN_POINT('Ctrl Pts',(13.8930570711896,-0.0439763023801491,
4.56037555616609));
#43865=CARTESIAN_POINT('Ctrl Pts',(13.9407729072525,-0.495129579482757,
4.26608528452492));
#43866=CARTESIAN_POINT('Ctrl Pts',(13.9884887433153,-0.491597745198497,
3.72744480185615));
#43867=CARTESIAN_POINT('Ctrl Pts',(14.0362045793781,-0.0366241372948624,
3.43909595144367));
#43868=CARTESIAN_POINT('Ctrl Pts',(14.083920415441,0.451981979421435,3.66583391943861));
#43869=CARTESIAN_POINT('Ctrl Pts',(14.1316362515038,0.525526089798339,4.19944174101915));
#43870=CARTESIAN_POINT('Ctrl Pts',(14.1793520875667,0.11647150565515,4.54989914301615));
#43871=CARTESIAN_POINT('Ctrl Pts',(14.2270679236295,-0.399540654275635,
4.39537570069553));
#43872=CARTESIAN_POINT('Ctrl Pts',(14.2747837596924,-0.548648483661927,
3.87777266878906));
#43873=CARTESIAN_POINT('Ctrl Pts',(14.3224995957551,-0.193923968459428,
3.47241287584284));
#43874=CARTESIAN_POINT('Ctrl Pts',(14.370215431818,0.338883910883161,3.5515444569815));
#43875=CARTESIAN_POINT('Ctrl Pts',(14.4179312678808,0.560489480462528,4.04249966364955));
#43876=CARTESIAN_POINT('Ctrl Pts',(14.4656471039437,0.267388935893957,4.49442677524682));
#43877=CARTESIAN_POINT('Ctrl Pts',(14.5133629400065,-0.271258982813659,
4.49231417140114));
#43878=CARTESIAN_POINT('Ctrl Pts',(14.5610787760694,-0.560805603747543,
4.03810188873054));
#43879=CARTESIAN_POINT('Ctrl Pts',(14.6087946121322,-0.335355809656676,
3.54890005536578));
#43880=CARTESIAN_POINT('Ctrl Pts',(14.656510448195,0.198056384554314,3.47395024222346));
#43881=CARTESIAN_POINT('Ctrl Pts',(14.7042262842579,0.549590353339887,3.88208001596329));
#43882=CARTESIAN_POINT('Ctrl Pts',(14.7519421203207,0.396427044118869,4.3984975254762));
#43883=CARTESIAN_POINT('Ctrl Pts',(14.7996579563836,-0.120781319530639,
4.54896862567174));
#43884=CARTESIAN_POINT('Ctrl Pts',(14.8473737924464,-0.527074338995675,
4.19531338994486));
#43885=CARTESIAN_POINT('Ctrl Pts',(14.8950896285092,-0.449346882879826,
3.66229886294881));
#43886=CARTESIAN_POINT('Ctrl Pts',(14.9428054645721,0.041022729875082,3.43940048630678));
#43887=CARTESIAN_POINT('Ctrl Pts',(14.9905213006349,0.493720538569869,3.73130926902151));
#43888=CARTESIAN_POINT('Ctrl Pts',(15.0382371366977,0.493027179828974,4.2699608843321));
#43889=CARTESIAN_POINT('Ctrl Pts',(15.0859529727606,0.0395793756528551,
4.56070326567839));
#43890=CARTESIAN_POINT('Ctrl Pts',(15.1336688088234,-0.450214778192253,
4.33654321062351));
#43891=CARTESIAN_POINT('Ctrl Pts',(15.1813846448863,-0.526569773778615,
3.80333034687015));
#43892=CARTESIAN_POINT('Ctrl Pts',(15.2291004809491,-0.119367643786657,
3.45072225173751));
#43893=CARTESIAN_POINT('Ctrl Pts',(15.2768163170119,0.397451630201876,3.60252436455885));
#43894=CARTESIAN_POINT('Ctrl Pts',(15.3245321530748,0.549284956596614,4.11933446935456));
#43895=CARTESIAN_POINT('Ctrl Pts',(15.3722479891376,0.196701455513243,4.52655789474516));
#43896=CARTESIAN_POINT('Ctrl Pts',(15.4199638252005,-0.336516018808871,
4.45023510325662));
#43897=CARTESIAN_POINT('Ctrl Pts',(15.4676796612633,-0.560705655094284,
3.96045448869));
#43898=CARTESIAN_POINT('Ctrl Pts',(15.5153954973261,-0.269990660741143,
3.50698912564524));
#43899=CARTESIAN_POINT('Ctrl Pts',(15.5631113333889,0.268660911710894,3.50626323446785));
#43900=CARTESIAN_POINT('Ctrl Pts',(15.6108271694518,0.560597035059331,3.95894341219528));
#43901=CARTESIAN_POINT('Ctrl Pts',(15.6585430055146,0.337728275218647,4.44932648624059));
#43902=CARTESIAN_POINT('Ctrl Pts',(15.7062588415775,-0.1952815563728,4.52708613419449));
#43903=CARTESIAN_POINT('Ctrl Pts',(15.7539746776403,-0.548961329954127,
4.12081447485494));
#43904=CARTESIAN_POINT('Ctrl Pts',(15.8016905137031,-0.398521467382777,
3.60359702428645));
#43905=CARTESIAN_POINT('Ctrl Pts',(15.849406349766,0.117886790727162,3.4504025257595));
#43906=CARTESIAN_POINT('Ctrl Pts',(15.8971221858288,0.526037794990907,3.80191184447176));
#43907=CARTESIAN_POINT('Ctrl Pts',(15.9448380218916,0.451120197982628,4.33532856438364));
#43908=CARTESIAN_POINT('Ctrl Pts',(15.9925538579545,-0.0380680182095728,
4.56080790392885));
#43909=CARTESIAN_POINT('Ctrl Pts',(16.0402696940173,-0.492297787528177,
4.27128871615743));
#43910=CARTESIAN_POINT('Ctrl Pts',(16.0879855300802,-0.494442923584513,
3.73264092602517));
#43911=CARTESIAN_POINT('Ctrl Pts',(16.135701366143,-0.0425335149309099,
3.43951308737216));
#43912=CARTESIAN_POINT('Ctrl Pts',(16.1834172022058,0.448435074945997,3.66108900478495));
#43913=CARTESIAN_POINT('Ctrl Pts',(16.2311330382687,0.52759883543946,4.19389210391969));
#43914=CARTESIAN_POINT('Ctrl Pts',(16.2788488743315,0.122260467197297,4.54864110061148));
#43915=CARTESIAN_POINT('Ctrl Pts',(16.3265647103944,-0.395351569291248,
4.39956453268331));
#43916=CARTESIAN_POINT('Ctrl Pts',(16.3742805464572,-0.549906176433804,
3.88356170630145));
#43917=CARTESIAN_POINT('Ctrl Pts',(16.42199638252,-0.199473480363076,3.47448595665642));
#43918=CARTESIAN_POINT('Ctrl Pts',(16.4697122185829,0.334138782019088,3.54799783908671));
#43919=CARTESIAN_POINT('Ctrl Pts',(16.5174280546457,0.560906259487099,4.0365902608309));
#43920=CARTESIAN_POINT('Ctrl Pts',(16.5651438907085,0.272584888215931,4.49158128304055));
#43921=CARTESIAN_POINT('Ctrl Pts',(16.6128597267714,-0.26605538016154,4.49514564908375));
#43922=CARTESIAN_POINT('Ctrl Pts',(16.6605755628342,-0.560372899148451,
4.04401014677825));
#43923=CARTESIAN_POINT('Ctrl Pts',(16.7082913988971,-0.340091362401967,
3.55245944950311));
#43924=CARTESIAN_POINT('Ctrl Pts',(16.7560072349599,0.19250130541649,3.4718921260458));
#43925=CARTESIAN_POINT('Ctrl Pts',(16.8037230710227,0.548317062457662,3.87629438922476));
#43926=CARTESIAN_POINT('Ctrl Pts',(16.8514389070856,0.400604824101502,4.39429741823411));
#43927=CARTESIAN_POINT('Ctrl Pts',(16.8991547431484,-0.114988988324618,
4.55021106103346));
#43928=CARTESIAN_POINT('Ctrl Pts',(16.9468705792113,-0.524986643439221,
4.20085742040038));
#43929=CARTESIAN_POINT('Ctrl Pts',(16.9945864152741,-0.45288098592576,3.66705332002498));
#43930=CARTESIAN_POINT('Ctrl Pts',(17.0423022513369,0.0351122494330066,
3.4389992789138));
#43931=CARTESIAN_POINT('Ctrl Pts',(17.0900180873998,0.490861365866046,3.72612083208173));
#43932=CARTESIAN_POINT('Ctrl Pts',(17.1377339234626,0.49584493715134,4.26474983932169));
#43933=CARTESIAN_POINT('Ctrl Pts',(17.1854497595254,0.0454864730955262,
4.56025499541263));
#43934=CARTESIAN_POINT('Ctrl Pts',(17.2331655955883,-0.446642919103261,
4.34126936858499));
#43935=CARTESIAN_POINT('Ctrl Pts',(17.2808814316511,-0.528613246204851,
3.80889082948154));
#43936=CARTESIAN_POINT('Ctrl Pts',(17.328597267714,-0.125149895556227,3.45201078225777));
#43937=CARTESIAN_POINT('Ctrl Pts',(17.3763131037768,0.393240529860342,3.59835766558462));
#43938=CARTESIAN_POINT('Ctrl Pts',(17.4240289398397,0.55051212592285,4.1135388846668));
#43939=CARTESIAN_POINT('Ctrl Pts',(17.4717447759024,0.202239966032548,4.52445559893916));
#43940=CARTESIAN_POINT('Ctrl Pts',(17.5194606119653,-0.331752266527324,
4.45375666691904));
#43941=CARTESIAN_POINT('Ctrl Pts',(17.5671764480281,-0.561091288070378,
3.96636600572338));
#43942=CARTESIAN_POINT('Ctrl Pts',(17.614892284091,-0.275171546279217,3.50986195899749));
#43943=CARTESIAN_POINT('Ctrl Pts',(17.6626081201538,0.263442460518632,3.50345921706735));
#43944=CARTESIAN_POINT('Ctrl Pts',(17.7103239562167,0.560133202238927,3.95303751636628));
#43945=CARTESIAN_POINT('Ctrl Pts',(17.7580397922795,0.342445005586054,4.44574218699675));
#43946=CARTESIAN_POINT('Ctrl Pts',(17.8057556283423,-0.189715708890181,
4.52911494868296));
#43947=CARTESIAN_POINT('Ctrl Pts',(17.8534714644052,-0.547657568741173,
4.12659331151364));
#43948=CARTESIAN_POINT('Ctrl Pts',(17.901187300468,-0.402677056422281,3.60781908849286));
#43949=CARTESIAN_POINT('Ctrl Pts',(17.9489031365308,0.112087992792125,3.44919063098808));
#43950=CARTESIAN_POINT('Ctrl Pts',(17.9966189725937,0.523920913530056,3.79637889233847));
#43951=CARTESIAN_POINT('Ctrl Pts',(18.0443348086565,0.454629197813879,4.33055554996792));
#43952=CARTESIAN_POINT('Ctrl Pts',(18.0920506447194,-0.0321555056241734,
4.56117795981091));
#43953=CARTESIAN_POINT('Ctrl Pts',(18.1397664807822,-0.489411313471489,
4.27646201432672));
#43954=CARTESIAN_POINT('Ctrl Pts',(18.1874823168451,-0.497233181596917,
3.73786674717144));
#43955=CARTESIAN_POINT('Ctrl Pts',(18.2351981529079,-0.0484381681459794,
3.43999247952716));
#43956=CARTESIAN_POINT('Ctrl Pts',(18.2829139889707,0.444838360430441,3.65638173475637));
#43957=CARTESIAN_POINT('Ctrl Pts',(18.3306298250336,0.529612977905601,4.18832093020544));
#43958=CARTESIAN_POINT('Ctrl Pts',(18.3783456610964,0.128035848626906,4.54732211775687));
#43959=CARTESIAN_POINT('Ctrl Pts',(18.4260614971592,-0.391118570530631,
4.40370898293889));
#43960=CARTESIAN_POINT('Ctrl Pts',(18.4737773332221,-0.551102788237131,
3.88936367722697));
#43961=CARTESIAN_POINT('Ctrl Pts',(18.5214931692849,-0.205000835699102,
3.47661740907615));
#43962=CARTESIAN_POINT('Ctrl Pts',(18.5692090053478,0.329356538604741,3.54450142744705));
#43963=CARTESIAN_POINT('Ctrl Pts',(18.6169248414106,0.561260735706054,4.03067679373969));
#43964=CARTESIAN_POINT('Ctrl Pts',(18.6646406774734,0.2777505631021,4.48868118831814));
#43965=CARTESIAN_POINT('Ctrl Pts',(18.7123565135363,-0.260822225340423,
4.49792212833724));
#43966=CARTESIAN_POINT('Ctrl Pts',(18.7600723495991,-0.559877950986752,
4.04991351638789));
#43967=CARTESIAN_POINT('Ctrl Pts',(18.8077881856619,-0.344789139412875,
3.55606855432066));
#43968=CARTESIAN_POINT('Ctrl Pts',(18.8555040217248,0.186924844147682,3.46989266958543));
#43969=CARTESIAN_POINT('Ctrl Pts',(18.9032198577876,0.546982867117114,3.87052250311704));
#43970=CARTESIAN_POINT('Ctrl Pts',(18.9509356938504,0.404738106803207,4.39005351430856));
#43971=CARTESIAN_POINT('Ctrl Pts',(18.9986515299133,-0.109183884691052,
4.55139238155646));
#43972=CARTESIAN_POINT('Ctrl Pts',(19.0463673659761,-0.522840634850846,
4.20637914057629));
#43973=CARTESIAN_POINT('Ctrl Pts',(19.094083202039,-0.456364785113784,3.67184475922049));
#43974=CARTESIAN_POINT('Ctrl Pts',(19.1417990381018,0.029197868913272,3.43866038485254));
#43975=CARTESIAN_POINT('Ctrl Pts',(19.1895148741647,0.487947670564988,3.72096281627648));
#43976=CARTESIAN_POINT('Ctrl Pts',(19.2372307102275,0.498607618457993,4.25950938727589));
#43977=CARTESIAN_POINT('Ctrl Pts',(19.2849465462903,0.0513885179525073,
4.55974449445321));
#43978=CARTESIAN_POINT('Ctrl Pts',(19.3326623823531,-0.44302144872845,4.34595762039384));
#43979=CARTESIAN_POINT('Ctrl Pts',(19.380378218416,-0.530598003365269,3.81447253878192));
#43980=CARTESIAN_POINT('Ctrl Pts',(19.4280940544788,-0.130918245164485,
3.45336018235082));
#43981=CARTESIAN_POINT('Ctrl Pts',(19.4758098905417,0.38898574814073,3.59423557624425));
#43982=CARTESIAN_POINT('Ctrl Pts',(19.5235257266045,0.551678150913516,4.10773069407674));
#43983=CARTESIAN_POINT('Ctrl Pts',(19.5712415626673,0.207756005258534,4.52229503878775));
#43984=CARTESIAN_POINT('Ctrl Pts',(19.6189573987302,-0.326951650734615,
4.4572278489044));
#43985=CARTESIAN_POINT('Ctrl Pts',(19.666673234793,-0.561414624206118,3.9722812219163));
#43986=CARTESIAN_POINT('Ctrl Pts',(19.7143890708559,-0.280321816997631,
3.51278930393937));
#43987=CARTESIAN_POINT('Ctrl Pts',(19.7621049069187,0.258194652845487,3.5007102220535));
#43988=CARTESIAN_POINT('Ctrl Pts',(19.8098207429815,0.559607330995945,3.94713708427543));
#43989=CARTESIAN_POINT('Ctrl Pts',(19.8575365790444,0.347123361713752,4.44210790974427));
#43990=CARTESIAN_POINT('Ctrl Pts',(19.9052524151072,-0.184128152223511,
4.53108587353909));
#43991=CARTESIAN_POINT('Ctrl Pts',(19.9529682511701,-0.546294178096705,
4.13235642149579));
#43992=CARTESIAN_POINT('Ctrl Pts',(20.0006840872329,-0.406785648814185,
3.61208785870539));
#43993=CARTESIAN_POINT('Ctrl Pts',(20.0483999232957,0.106272459957556,3.44803398021027));
#43994=CARTESIAN_POINT('Ctrl Pts',(20.0961157593586,0.5217539278249,3.7908797683689));
#43995=CARTESIAN_POINT('Ctrl Pts',(20.1438315954214,0.458072423058868,4.32572464996293));
#43996=CARTESIAN_POINT('Ctrl Pts',(20.1915474314842,-0.0262105744965466,
4.56152565902554));
#43997=CARTESIAN_POINT('Ctrl Pts',(20.2392632675471,-0.486524960252488,
4.28152908133109));
#43998=CARTESIAN_POINT('Ctrl Pts',(20.2869791036099,-0.499865224545849,
3.74326461201656));
#43999=CARTESIAN_POINT('Ctrl Pts',(20.3346949396728,-0.0545328049175168,
3.440261547834));
#44000=CARTESIAN_POINT('Ctrl Pts',(20.3824107757356,0.441568512678419,3.6522489094147));
#44001=CARTESIAN_POINT('Ctrl Pts',(20.4221739724547,0.515928418030698,4.09332268501583));
#44002=CARTESIAN_POINT('Ctrl Pts',(20.4539845298298,0.333108474939506,4.36566768059473));
#44003=CARTESIAN_POINT('Ctrl Pts',(20.4778424478613,0.118510552090848,4.48142006140068));
#44004=CARTESIAN_POINT('Ctrl Pts',(20.5017003658927,-0.127372553428812,
4.47887124859312));
#44005=CARTESIAN_POINT('Ctrl Pts',(20.5255582839241,-0.340862259689409,
4.35954554232165));
#44006=CARTESIAN_POINT('Ctrl Pts',(20.5494162019555,-0.471665647836603,
4.15213005589169));
#44007=CARTESIAN_POINT('Ctrl Pts',(20.5732741199869,-0.486782001098211,
3.90760543082941));
#44008=CARTESIAN_POINT('Ctrl Pts',(20.5971320380184,-0.38305332993788,3.68562568155832));
#44009=CARTESIAN_POINT('Ctrl Pts',(20.6209899560498,-0.185558943137764,
3.54054450025879));
#44010=CARTESIAN_POINT('Ctrl Pts',(20.6448478740812,0.0572573647513246,
3.50779920733485));
#44011=CARTESIAN_POINT('Ctrl Pts',(20.6687057921126,0.28610038304352,3.59541756340761));
#44012=CARTESIAN_POINT('Ctrl Pts',(20.6925637101441,0.444969396676924,3.78196356026503));
#44013=CARTESIAN_POINT('Ctrl Pts',(20.7164216281754,0.495039040219165,4.02182741068269));
#44014=CARTESIAN_POINT('Ctrl Pts',(20.7402795462069,0.424054039808096,4.25635280284423));
#44015=CARTESIAN_POINT('Ctrl Pts',(20.7641374642383,0.249378454468877,4.42819351412177));
#44016=CARTESIAN_POINT('Ctrl Pts',(20.7879953822697,0.0137218901755031,
4.49532894963167));
#44017=CARTESIAN_POINT('Ctrl Pts',(20.8118533003011,-0.22528943893053,4.44134312218709));
#44018=CARTESIAN_POINT('Ctrl Pts',(20.8357112183326,-0.409211687104306,
4.27943679589328));
#44019=CARTESIAN_POINT('Ctrl Pts',(20.859569136364,-0.493070359673604,4.04920060553547));
#44020=CARTESIAN_POINT('Ctrl Pts',(20.8834270543954,-0.456359989112496,
3.80693350349834));
#44021=CARTESIAN_POINT('Ctrl Pts',(20.9072849724268,-0.308057122141145,
3.61187643128937));
#44022=CARTESIAN_POINT('Ctrl Pts',(20.9311428904583,-0.0844259229598539,
3.51172613733272));
#44023=CARTESIAN_POINT('Ctrl Pts',(20.9550008084896,0.159849727585384,3.53097210659131));
#44024=CARTESIAN_POINT('Ctrl Pts',(20.9788587265211,0.365037758375503,3.66490817000854));
#44025=CARTESIAN_POINT('Ctrl Pts',(21.0027166445525,0.480964117596,3.88078331455297));
#44026=CARTESIAN_POINT('Ctrl Pts',(21.026574562584,0.479281646861755,4.12581018556955));
#44027=CARTESIAN_POINT('Ctrl Pts',(21.0504324806153,0.360401759160676,4.34007303948752));
#44028=CARTESIAN_POINT('Ctrl Pts',(21.0742903986468,0.153393823636192,4.47117877170218));
#44029=CARTESIAN_POINT('Ctrl Pts',(21.0981483166782,-0.0911230798336762,
4.48706845966041));
#44030=CARTESIAN_POINT('Ctrl Pts',(21.1220062347096,-0.313357908298923,
4.38385664171252));
#44031=CARTESIAN_POINT('Ctrl Pts',(21.145864152741,-0.458968192403581,4.18678141884249));
#44032=CARTESIAN_POINT('Ctrl Pts',(21.1697220707724,-0.492348251467217,
3.94403305123036));
#44033=CARTESIAN_POINT('Ctrl Pts',(21.1935799888039,-0.405335751726616,
3.71497012710753));
#44034=CARTESIAN_POINT('Ctrl Pts',(21.2174379068353,-0.21920761957706,3.55560477096155));
#44035=CARTESIAN_POINT('Ctrl Pts',(21.2412958248667,0.0205227466613194,
3.50490615340017));
#44036=CARTESIAN_POINT('Ctrl Pts',(21.2651537428981,0.255234742309135,3.57527146741714));
#44037=CARTESIAN_POINT('Ctrl Pts',(21.2890116609295,0.427534891009427,3.74949447702405));
#44038=CARTESIAN_POINT('Ctrl Pts',(21.312869578961,0.495291113040325,3.98497291063177));
#44039=CARTESIAN_POINT('Ctrl Pts',(21.3367274969923,0.441935166474334,4.22412587691986));
#44040=CARTESIAN_POINT('Ctrl Pts',(21.3605854150238,0.280514033632862,4.40847396123464));
#44041=CARTESIAN_POINT('Ctrl Pts',(21.3844433330552,0.0504995785194436,
4.49293903542029));
#44042=CARTESIAN_POINT('Ctrl Pts',(21.4083012510867,-0.191863399122956,
4.45686708805594));
#44043=CARTESIAN_POINT('Ctrl Pts',(21.432159169118,-0.387310549425693,4.3090786928523));
#44044=CARTESIAN_POINT('Ctrl Pts',(21.4560170871495,-0.488049720266331,
4.08571213811173));
#44045=CARTESIAN_POINT('Ctrl Pts',(21.4798750051809,-0.469447440294381,
3.84138663085107));
#44046=CARTESIAN_POINT('Ctrl Pts',(21.5037329232123,-0.336052473678932,
3.63584641288874));
#44047=CARTESIAN_POINT('Ctrl Pts',(21.5275908412437,-0.120483523363382,
3.51935166631968));
#44048=CARTESIAN_POINT('Ctrl Pts',(21.5514487592752,0.124546930319796,3.5203885299332));
#44049=CARTESIAN_POINT('Ctrl Pts',(21.5753066773065,0.339122266949511,3.63870346233219));
#44050=CARTESIAN_POINT('Ctrl Pts',(21.599164595338,0.470772971804989,3.84536523971104));
#44051=CARTESIAN_POINT('Ctrl Pts',(21.6230225133694,0.487306861455871,4.08983942814686));
#44052=CARTESIAN_POINT('Ctrl Pts',(21.6468804314008,0.384680949508402,4.31234542922385));
#44053=CARTESIAN_POINT('Ctrl Pts',(21.6707383494323,0.187990066907445,4.45847446473699));
#44054=CARTESIAN_POINT('Ctrl Pts',(21.6945962674636,-0.0546695077989956,
4.49249400502822));
#44055=CARTESIAN_POINT('Ctrl Pts',(21.7184541854951,-0.283960898681086,
4.40608534582272));
#44056=CARTESIAN_POINT('Ctrl Pts',(21.7423121035264,-0.443816114896065,
4.22037775802082));
#44057=CARTESIAN_POINT('Ctrl Pts',(21.766170021558,-0.495146201710716,3.98078180541326));
#44058=CARTESIAN_POINT('Ctrl Pts',(21.7900279395893,-0.425399554695369,
3.74588522487523));
#44059=CARTESIAN_POINT('Ctrl Pts',(21.8138858576208,-0.25163112890579,3.57312662880273));
#44060=CARTESIAN_POINT('Ctrl Pts',(21.8377437756521,-0.0163320378044167,
3.50475019978512));
#44061=CARTESIAN_POINT('Ctrl Pts',(21.8616016936836,0.222960681415914,3.55747583725374));
#44062=CARTESIAN_POINT('Ctrl Pts',(21.885459611715,0.407733440703041,3.71841068663001));
#44063=CARTESIAN_POINT('Ctrl Pts',(21.9093175297464,0.492804267302335,3.94820179346412));
#44064=CARTESIAN_POINT('Ctrl Pts',(21.9331754477779,0.457371026827486,4.19065897275109));
#44065=CARTESIAN_POINT('Ctrl Pts',(21.9570333658092,0.310098111756678,4.38649483975425));
#44066=CARTESIAN_POINT('Ctrl Pts',(21.9808912838407,0.0869977614584207,
4.48782219052945));
#44067=CARTESIAN_POINT('Ctrl Pts',(22.0047492018721,-0.15737591128791,4.46986372771052));
#44068=CARTESIAN_POINT('Ctrl Pts',(22.0286071199035,-0.363266886890503,
4.33701078463543));
#44069=CARTESIAN_POINT('Ctrl Pts',(22.0524650379349,-0.480329213457224,
4.12174952472744));
#44070=CARTESIAN_POINT('Ctrl Pts',(22.0763229559664,-0.479937963428243,
3.87671718963328));
#44071=CARTESIAN_POINT('Ctrl Pts',(22.1001808739978,-0.362188808094022,
3.66183085982978));
#44072=CARTESIAN_POINT('Ctrl Pts',(22.1240387920292,-0.155874623354616,
3.529636096341));
#44073=CARTESIAN_POINT('Ctrl Pts',(22.1478967100606,0.0885551527323001,
3.51245811975107));
#44074=CARTESIAN_POINT('Ctrl Pts',(22.1717546280921,0.311330781786364,3.61449741325855));
#44075=CARTESIAN_POINT('Ctrl Pts',(22.1956125461234,0.457977554205651,3.81080259009947));
#44076=CARTESIAN_POINT('Ctrl Pts',(22.2194704641549,0.492636339578261,4.05337168730347));
#44077=CARTESIAN_POINT('Ctrl Pts',(22.2433283821863,0.406832120751761,4.28288995313029));
#44078=CARTESIAN_POINT('Ctrl Pts',(22.2671863002177,0.22154636656941,4.44323391967918));
#44079=CARTESIAN_POINT('Ctrl Pts',(22.2910442182491,-0.0179135091400202,
4.49519511936025));
#44080=CARTESIAN_POINT('Ctrl Pts',(22.3149021362805,-0.2529930437236,4.42606762362056));
#44081=CARTESIAN_POINT('Ctrl Pts',(22.338760054312,-0.426208888077552,4.25275498785448));
#44082=CARTESIAN_POINT('Ctrl Pts',(22.3626179723434,-0.495205048933098,
4.01763687303198));
#44083=CARTESIAN_POINT('Ctrl Pts',(22.3864758903748,-0.443110087468167,
3.77820606161377));
#44084=CARTESIAN_POINT('Ctrl Pts',(22.4103338084062,-0.282662637164788,
3.59300991103726));
#44085=CARTESIAN_POINT('Ctrl Pts',(22.4341917264377,-0.0530964769854286,
3.50733392083031));
#44086=CARTESIAN_POINT('Ctrl Pts',(22.458049644469,0.189453226607198,3.5421282117862));
#44087=CARTESIAN_POINT('Ctrl Pts',(22.4819075625005,0.385676439696491,3.6888846179772));
#44088=CARTESIAN_POINT('Ctrl Pts',(22.5057654805319,0.487591287867653,3.9117172269821));
#44089=CARTESIAN_POINT('Ctrl Pts',(22.5296233985634,0.470276727405835,4.15613734610506));
#44090=CARTESIAN_POINT('Ctrl Pts',(22.5534813165947,0.337966804695391,4.36237769267677));
#44091=CARTESIAN_POINT('Ctrl Pts',(22.5773392346262,0.123014588878675,4.48000670597833));
#44092=CARTESIAN_POINT('Ctrl Pts',(22.6011971526576,-0.122017660845505,
4.48026122441149));
#44093=CARTESIAN_POINT('Ctrl Pts',(22.625055070689,-0.337213993725473,4.36307837627545));
#44094=CARTESIAN_POINT('Ctrl Pts',(22.6489129887204,-0.469950950795418,
4.15711375897153));
#44095=CARTESIAN_POINT('Ctrl Pts',(22.6727709067518,-0.487774683880463,
3.912729067726));
#44096=CARTESIAN_POINT('Ctrl Pts',(22.6966288247832,-0.386319338946922,
3.6896872918462));
#44097=CARTESIAN_POINT('Ctrl Pts',(22.7204867428147,-0.190407614498503,
3.54252014522276));
#44098=CARTESIAN_POINT('Ctrl Pts',(22.7443446608461,0.0520814161336476,
3.50722927763546));
#44099=CARTESIAN_POINT('Ctrl Pts',(22.7682025788775,0.281801791424649,3.59241522467272));
#44100=CARTESIAN_POINT('Ctrl Pts',(22.7920604969089,0.442679857002608,3.77730419914427));
#44101=CARTESIAN_POINT('Ctrl Pts',(22.8079657755965,0.477669651496365,3.93681187972983));
#44102=CARTESIAN_POINT('Ctrl Pts',(22.8159184149403,0.475016281724327,4.01593044384941));
#44103=CARTESIAN_POINT('Ctrl Pts',(3.98408158505964,0.229225853138217,4.48306385360099));
#44104=CARTESIAN_POINT('Ctrl Pts',(3.99203422440344,0.148766887950233,4.52124364039387));
#44105=CARTESIAN_POINT('Ctrl Pts',(4.00793950309106,-0.0315132651739855,
4.55658776856145));
#44106=CARTESIAN_POINT('Ctrl Pts',(4.03179742112247,-0.29437836981663,4.47338935048851));
#44107=CARTESIAN_POINT('Ctrl Pts',(4.0556553391539,-0.485191777607318,4.27448557757091));
#44108=CARTESIAN_POINT('Ctrl Pts',(4.07951325718531,-0.557397168683185,
4.00843674174317));
#44109=CARTESIAN_POINT('Ctrl Pts',(4.10337117521674,-0.493285636019562,
3.74033843218029));
#44110=CARTESIAN_POINT('Ctrl Pts',(4.12722909324815,-0.308561908987092,
3.53572729771651));
#44111=CARTESIAN_POINT('Ctrl Pts',(4.15108701127957,-0.0483813190761145,
3.44464727048097));
#44112=CARTESIAN_POINT('Ctrl Pts',(4.17494492931099,0.223627135909104,3.48936410886239));
#44113=CARTESIAN_POINT('Ctrl Pts',(4.19880284734241,0.440954086798485,3.65894639349553));
#44114=CARTESIAN_POINT('Ctrl Pts',(4.22266076537383,0.55045499896491,3.91192501290154));
#44115=CARTESIAN_POINT('Ctrl Pts',(4.24651868340524,0.525355068663259,4.18644066347397));
#44116=CARTESIAN_POINT('Ctrl Pts',(4.27037660143667,0.371791302444591,4.41536633561891));
#44117=CARTESIAN_POINT('Ctrl Pts',(4.29423451946808,0.127314547262185,4.54272370785395));
#44118=CARTESIAN_POINT('Ctrl Pts',(4.31809243749951,-0.14829414195428,4.5373703057994));
#44119=CARTESIAN_POINT('Ctrl Pts',(4.34195035553092,-0.387640842632661,
4.40061524972397));
#44120=CARTESIAN_POINT('Ctrl Pts',(4.36580827356235,-0.53219881478122,4.16589884014724));
#44121=CARTESIAN_POINT('Ctrl Pts',(4.38966619159376,-0.546619671109945,
3.89061565172978));
#44122=CARTESIAN_POINT('Ctrl Pts',(4.41352410962518,-0.427377132892538,
3.64207991255526));
#44123=CARTESIAN_POINT('Ctrl Pts',(4.4373820276566,-0.203629241694984,3.48106538615089));
#44124=CARTESIAN_POINT('Ctrl Pts',(4.46123994568802,0.0699115445388116,
3.44694450735191));
#44125=CARTESIAN_POINT('Ctrl Pts',(4.48509786371944,0.326357054473012,3.54806076195131));
#44126=CARTESIAN_POINT('Ctrl Pts',(4.50895578175085,0.502999374434197,3.7596884705576));
#44127=CARTESIAN_POINT('Ctrl Pts',(4.53281369978229,0.556644646112557,4.03007889421215));
#44128=CARTESIAN_POINT('Ctrl Pts',(4.55667161781369,0.474175139017821,4.29311420882242));
#44129=CARTESIAN_POINT('Ctrl Pts',(4.58052953584512,0.275756894216243,4.48447511514554));
#44130=CARTESIAN_POINT('Ctrl Pts',(4.60438745387653,0.00990857728296194,
4.55736865895685));
#44131=CARTESIAN_POINT('Ctrl Pts',(4.62824537190795,-0.258362656684952,
4.49397038324719));
#44132=CARTESIAN_POINT('Ctrl Pts',(4.65210328993938,-0.463457183444019,
4.30978289334447));
#44133=CARTESIAN_POINT('Ctrl Pts',(4.67596120797079,-0.555223804526532,
4.04984504770563));
#44134=CARTESIAN_POINT('Ctrl Pts',(4.69981912600221,-0.511223081411799,
3.77771873014923));
#44135=CARTESIAN_POINT('Ctrl Pts',(4.72367704403363,-0.342214389453536,
3.55994623789246));
#44136=CARTESIAN_POINT('Ctrl Pts',(4.74753496206505,-0.0895249575417115,
3.44977887729433));
#44137=CARTESIAN_POINT('Ctrl Pts',(4.77139288009647,0.185055765100279,3.47415556892044));
#44138=CARTESIAN_POINT('Ctrl Pts',(4.79525079812788,0.414385312357242,3.62711554766008));
#44139=CARTESIAN_POINT('Ctrl Pts',(4.81910871615931,0.542386363113676,3.87125593216545));
#44140=CARTESIAN_POINT('Ctrl Pts',(4.84296663419071,0.537759173780872,4.14687774817434));
#44141=CARTESIAN_POINT('Ctrl Pts',(4.86682455222215,0.401635218192884,4.38658395388507));
#44142=CARTESIAN_POINT('Ctrl Pts',(4.89068247025356,0.167300511433038,4.53175985253543));
#44143=CARTESIAN_POINT('Ctrl Pts',(4.91454038828499,-0.107943727546613,
4.54690598239331));
#44144=CARTESIAN_POINT('Ctrl Pts',(4.9383983063164,-0.356792784813018,4.42831870213619));
#44145=CARTESIAN_POINT('Ctrl Pts',(4.96225622434782,-0.518396287352312,
4.20499583203957));
#44146=CARTESIAN_POINT('Ctrl Pts',(4.98611414237924,-0.553237776802617,
3.93154589703492));
#44147=CARTESIAN_POINT('Ctrl Pts',(5.00997206041066,-0.452797559930213,
3.67483485485756));
#44148=CARTESIAN_POINT('Ctrl Pts',(5.03382997844208,-0.241636005696979,
3.49763554798826));
#44149=CARTESIAN_POINT('Ctrl Pts',(5.05768789647349,0.0286121339618079,
3.44327803376872));
#44150=CARTESIAN_POINT('Ctrl Pts',(5.08154581450492,0.291863827488053,3.52505420509465));
#44151=CARTESIAN_POINT('Ctrl Pts',(5.10540373253633,0.48374686498243,3.72296756053861));
#44152=CARTESIAN_POINT('Ctrl Pts',(5.12926165056775,0.557340616988569,3.98862289364304));
#44153=CARTESIAN_POINT('Ctrl Pts',(5.15311956859917,0.49464940648741,4.25706023915787));
#44154=CARTESIAN_POINT('Ctrl Pts',(5.17697748663059,0.311002942120779,4.46263935401832));
#44155=CARTESIAN_POINT('Ctrl Pts',(5.20083540466201,0.0513077868555636,
4.55509054477827));
#44156=CARTESIAN_POINT('Ctrl Pts',(5.22469332269342,-0.22093351989189,4.5118069769771));
#44157=CARTESIAN_POINT('Ctrl Pts',(5.24855124072485,-0.439150562917527,
4.34337266196288));
#44158=CARTESIAN_POINT('Ctrl Pts',(5.27240915875626,-0.549983331088669,
4.09097437781523));
#44159=CARTESIAN_POINT('Ctrl Pts',(5.29626707678769,-0.526330193563486,
3.81633038019944));
#44160=CARTESIAN_POINT('Ctrl Pts',(5.32012499481911,-0.373974986765411,
3.5865986076849));
#44161=CARTESIAN_POINT('Ctrl Pts',(5.34398291285052,-0.130172708829089,
3.45795473641922));
#44162=CARTESIAN_POINT('Ctrl Pts',(5.36784083088195,0.145460342249349,3.46185569711558));
#44163=CARTESIAN_POINT('Ctrl Pts',(5.39169874891335,0.385524377387638,3.59734759862366));
#44164=CARTESIAN_POINT('Ctrl Pts',(5.41555666694479,0.531317200781484,3.83129898029949));
#44165=CARTESIAN_POINT('Ctrl Pts',(5.4394145849762,0.547188495794237,4.10650235661553));
#44166=CARTESIAN_POINT('Ctrl Pts',(5.46327250300762,0.42925729847004,4.35566300567327));
#44167=CARTESIAN_POINT('Ctrl Pts',(5.48713042103904,0.206360998935678,4.51785436177788));
#44168=CARTESIAN_POINT('Ctrl Pts',(5.51098833907045,-0.0669961859988386,
4.55341622035867));
#44169=CARTESIAN_POINT('Ctrl Pts',(5.53484625710188,-0.323970978517869,
4.45365273830571));
#44170=CARTESIAN_POINT('Ctrl Pts',(5.55870417513329,-0.501726041995696,
4.2429588044862));
#44171=CARTESIAN_POINT('Ctrl Pts',(5.58256209316472,-0.556795421465071,
3.97285482490167));
#44172=CARTESIAN_POINT('Ctrl Pts',(5.60642001119613,-0.475713153578786,
3.70938858005442));
#44173=CARTESIAN_POINT('Ctrl Pts',(5.63027792922756,-0.27830606148521,3.51698474346866));
#44174=CARTESIAN_POINT('Ctrl Pts',(5.65413584725897,-0.0128455564368745,
3.44269129419766));
#44175=CARTESIAN_POINT('Ctrl Pts',(5.67799376529039,0.255756037034639,3.5046750042392));
#44176=CARTESIAN_POINT('Ctrl Pts',(5.70185168332181,0.46181831285622,3.68777916820271));
#44177=CARTESIAN_POINT('Ctrl Pts',(5.72570960135323,0.554953431393631,3.94722983012095));
#44178=CARTESIAN_POINT('Ctrl Pts',(5.74956751938465,0.512387319539865,4.21958423627784));
#44179=CARTESIAN_POINT('Ctrl Pts',(5.77342543741606,0.344528550506956,4.43824431479549));
#44180=CARTESIAN_POINT('Ctrl Pts',(5.79728335544749,0.0924231668635294,
4.54974172178225));
#44181=CARTESIAN_POINT('Ctrl Pts',(5.82114127347891,-0.182282200065281,
4.52681230129395));
#44182=CARTESIAN_POINT('Ctrl Pts',(5.84499919151032,-0.412414601109181,
4.37506292652603));
#44183=CARTESIAN_POINT('Ctrl Pts',(5.86885710954175,-0.541700403334708,
4.13160044316952));
#44184=CARTESIAN_POINT('Ctrl Pts',(5.89271502757316,-0.538525691690445,
3.85595807909033));
#44185=CARTESIAN_POINT('Ctrl Pts',(5.91657294560459,-0.403666797469215,
3.61553786496538));
#44186=CARTESIAN_POINT('Ctrl Pts',(5.94043086363599,-0.170100341263849,
3.46912915944898));
#44187=CARTESIAN_POINT('Ctrl Pts',(5.96428878166742,0.105060216979666,3.45253275189516));
#44188=CARTESIAN_POINT('Ctrl Pts',(5.98814669969884,0.354530812822036,3.5698071562788));
#44189=CARTESIAN_POINT('Ctrl Pts',(6.01200461773026,0.517308736525128,3.79227513259484));
#44190=CARTESIAN_POINT('Ctrl Pts',(6.03586253576167,0.553591019453439,4.06553805729756));
#44191=CARTESIAN_POINT('Ctrl Pts',(6.0597204537931,0.454504394384077,4.32277408438697));
#44192=CARTESIAN_POINT('Ctrl Pts',(6.08357837182452,0.244280620740535,4.50108505220882));
#44193=CARTESIAN_POINT('Ctrl Pts',(6.10743628985593,-0.0256793573627324,
4.55686330558177));
#44194=CARTESIAN_POINT('Ctrl Pts',(6.13129420788736,-0.289354484390735,
4.47648043042773));
#44195=CARTESIAN_POINT('Ctrl Pts',(6.15515212591877,-0.482285035214929,
4.27957167009689));
#44196=CARTESIAN_POINT('Ctrl Pts',(6.17901004395019,-0.557263974895364,
4.01432540012922));
#44197=CARTESIAN_POINT('Ctrl Pts',(6.20286796198161,-0.496014047041978,
3.74552825888183));
#44198=CARTESIAN_POINT('Ctrl Pts',(6.22672588001303,-0.313404643062,3.53904687299508));
#44199=CARTESIAN_POINT('Ctrl Pts',(6.25058379804445,-0.0542924323345977,
3.44511024149985));
#44200=CARTESIAN_POINT('Ctrl Pts',(6.27444171607587,0.218347115212216,3.48718178027374));
#44201=CARTESIAN_POINT('Ctrl Pts',(6.29829963410728,0.437120926894882,3.65404298137615));
#44202=CARTESIAN_POINT('Ctrl Pts',(6.32215755213871,0.549895923261456,3.90664388593688));
#44203=CARTESIAN_POINT('Ctrl Pts',(6.34601547017011,0.526573903738089,4.17995327069166));
#44204=CARTESIAN_POINT('Ctrl Pts',(6.37782602754536,0.327418726170013,4.4906154426808));
#44205=CARTESIAN_POINT('Ctrl Pts',(6.41758922426438,-0.161063729547888,
4.61146011675295));
#44206=CARTESIAN_POINT('Ctrl Pts',(6.46530506032721,-0.60205854017139,4.19446204504257));
#44207=CARTESIAN_POINT('Ctrl Pts',(6.51302089639007,-0.488859252747234,
3.59916283817905));
#44208=CARTESIAN_POINT('Ctrl Pts',(6.56073673245289,0.0725864685289804,
3.37181094029106));
#44209=CARTESIAN_POINT('Ctrl Pts',(6.60845256851574,0.567733426150434,3.72141305678318));
#44210=CARTESIAN_POINT('Ctrl Pts',(6.65616840457857,0.541332409494817,4.32680434473755));
#44211=CARTESIAN_POINT('Ctrl Pts',(6.70388424064141,0.0179179137367747,
4.6321081579338));
#44212=CARTESIAN_POINT('Ctrl Pts',(6.75160007670425,-0.522004047715759,
4.35692568061372));
#44213=CARTESIAN_POINT('Ctrl Pts',(6.79931591276708,-0.582533501572452,
3.75397902491298));
#44214=CARTESIAN_POINT('Ctrl Pts',(6.84703174882993,-0.10812839031349,3.37695395054049));
#44215=CARTESIAN_POINT('Ctrl Pts',(6.89474758489276,0.465580583415614,3.57208337966475));
#44216=CARTESIAN_POINT('Ctrl Pts',(6.9424634209556,0.611735560770294,4.16017430964564));
#44217=CARTESIAN_POINT('Ctrl Pts',(6.99017925701844,0.196126575106773,4.60117519156627));
#44218=CARTESIAN_POINT('Ctrl Pts',(7.03789509308127,-0.399589635450545,
4.49010738789885));
#44219=CARTESIAN_POINT('Ctrl Pts',(7.08561092914412,-0.628355913977057,
3.92896656470948));
#44220=CARTESIAN_POINT('Ctrl Pts',(7.13332676520695,-0.280093617253323,
3.43305676608093));
#44221=CARTESIAN_POINT('Ctrl Pts',(7.1810426012698,0.325383132256395,3.45777970086456));
#44222=CARTESIAN_POINT('Ctrl Pts',(7.22875843733263,0.632055452459012,3.98043185926557));
#44223=CARTESIAN_POINT('Ctrl Pts',(7.27647427339546,0.358301574124045,4.52105375310108));
#44224=CARTESIAN_POINT('Ctrl Pts',(7.32419010945831,-0.244486178793781,
4.58318396235269));
#44225=CARTESIAN_POINT('Ctrl Pts',(7.37190594552114,-0.622758498112341,
4.10976736853928));
#44226=CARTESIAN_POINT('Ctrl Pts',(7.41962178158399,-0.42914211350377,3.53554970961824));
#44227=CARTESIAN_POINT('Ctrl Pts',(7.46733761764681,0.158562080980748,3.38784389968312));
#44228=CARTESIAN_POINT('Ctrl Pts',(7.51505345370967,0.600656274672958,3.80229045545538));
#44229=CARTESIAN_POINT('Ctrl Pts',(7.56276928977248,0.491158570126743,4.3982967283715));
#44230=CARTESIAN_POINT('Ctrl Pts',(7.61048512583535,-0.0693776073840611,
4.62854098691609));
#44231=CARTESIAN_POINT('Ctrl Pts',(7.65820096189817,-0.566203260219877,
4.28158638589565));
#44232=CARTESIAN_POINT('Ctrl Pts',(7.70591679796101,-0.543075747198986,
3.67604667390869));
#44233=CARTESIAN_POINT('Ctrl Pts',(7.75363263402386,-0.0212334191459514,
3.36799828595259));
#44234=CARTESIAN_POINT('Ctrl Pts',(7.80134847008666,0.520107884382028,3.64032679659274));
#44235=CARTESIAN_POINT('Ctrl Pts',(7.84906430614954,0.583826114817312,4.24294874421058));
#44236=CARTESIAN_POINT('Ctrl Pts',(7.89678014221235,0.111407840683781,4.62246712177016));
#44237=CARTESIAN_POINT('Ctrl Pts',(7.94449597827521,-0.463317967772962,
4.43036436352186));
#44238=CARTESIAN_POINT('Ctrl Pts',(7.99221181433803,-0.612571757364041,
3.84305138824375));
#44239=CARTESIAN_POINT('Ctrl Pts',(8.03992765040088,-0.199291476537812,
3.39986673810663));
#44240=CARTESIAN_POINT('Ctrl Pts',(8.08764348646372,0.397001233685627,3.50779369660314));
#44241=CARTESIAN_POINT('Ctrl Pts',(8.13535932252656,0.628721602366905,4.06772127707659));
#44242=CARTESIAN_POINT('Ctrl Pts',(8.18307515858938,0.283077249469033,4.56545936678474));
#44243=CARTESIAN_POINT('Ctrl Pts',(8.23079099465223,-0.32252129731946,4.54392741926377));
#44244=CARTESIAN_POINT('Ctrl Pts',(8.27850683071506,-0.631943574151527,
4.02289855323374));
#44245=CARTESIAN_POINT('Ctrl Pts',(8.32622266677791,-0.361042343138453,
3.48084159342964));
#44246=CARTESIAN_POINT('Ctrl Pts',(8.37393850284074,0.241409626929164,3.41553578665797));
#44247=CARTESIAN_POINT('Ctrl Pts',(8.42165433890358,0.622171422023167,3.88695246013618));
#44248=CARTESIAN_POINT('Ctrl Pts',(8.46937017496642,0.431583626935426,4.46218242893131));
#44249=CARTESIAN_POINT('Ctrl Pts',(8.51708601102927,-0.155334053534803,
4.61298316164806));
#44250=CARTESIAN_POINT('Ctrl Pts',(8.56480184709209,-0.599606082522386,
4.20087202506506));
#44251=CARTESIAN_POINT('Ctrl Pts',(8.61251768315494,-0.493250619804184,
3.60429701705146));
#44252=CARTESIAN_POINT('Ctrl Pts',(8.66023351921777,0.0660644767165412,
3.37110214695249));
#44253=CARTESIAN_POINT('Ctrl Pts',(8.70794935528061,0.564711547735832,3.71543385214437));
#44254=CARTESIAN_POINT('Ctrl Pts',(8.75566519134344,0.544775315265253,4.32108702952508));
#44255=CARTESIAN_POINT('Ctrl Pts',(8.80338102740629,0.0245635283409047,
4.6318810471339));
#44256=CARTESIAN_POINT('Ctrl Pts',(8.85109686346912,-0.518205324617361,
4.36240897642002));
#44257=CARTESIAN_POINT('Ctrl Pts',(8.89881269953197,-0.585098254365674,
3.76013116628075));
#44258=CARTESIAN_POINT('Ctrl Pts',(8.9465285355948,-0.114686454236133,3.3781285970023));
#44259=CARTESIAN_POINT('Ctrl Pts',(8.99424437165764,0.461043681496376,3.56720010581811));
#44260=CARTESIAN_POINT('Ctrl Pts',(9.04196020772047,0.613390310441866,4.15371841694351));
#44261=CARTESIAN_POINT('Ctrl Pts',(9.08967604378332,0.202451179085494,4.59907474052783));
#44262=CARTESIAN_POINT('Ctrl Pts',(9.13739187984615,-0.394401985136886,
4.49429151193569));
#44263=CARTESIAN_POINT('Ctrl Pts',(9.18510771590899,-0.629069737753471,
3.93559278228048));
#44264=CARTESIAN_POINT('Ctrl Pts',(9.23282355197184,-0.28605307070895,3.43604019168954));
#44265=CARTESIAN_POINT('Ctrl Pts',(9.28053938803466,0.319650532659854,3.45438057070715));
#44266=CARTESIAN_POINT('Ctrl Pts',(9.32825522409751,0.631814133431458,3.97377166707843));
#44267=CARTESIAN_POINT('Ctrl Pts',(9.37597106016033,0.363773093762905,4.51724864514637));
#44268=CARTESIAN_POINT('Ctrl Pts',(9.4236868962232,-0.238326375276645,4.58572823348297));
#44269=CARTESIAN_POINT('Ctrl Pts',(9.47140273228601,-0.621567066777005,
4.11632457242483));
#44270=CARTESIAN_POINT('Ctrl Pts',(9.51911856834886,-0.434013156817378,
3.54009826662536));
#44271=CARTESIAN_POINT('Ctrl Pts',(9.5668344044117,0.152101713198456,3.38620679908157));
#44272=CARTESIAN_POINT('Ctrl Pts',(9.61455024047453,0.598539239598464,3.79597107236355));
#44273=CARTESIAN_POINT('Ctrl Pts',(9.66226607653739,0.495328972565208,4.39309824928265));
#44274=CARTESIAN_POINT('Ctrl Pts',(9.7099819126002,-0.0627495115905886,
4.62923725529147));
#44275=CARTESIAN_POINT('Ctrl Pts',(9.75769774866305,-0.563204153727404,
4.28753800770644));
#44276=CARTESIAN_POINT('Ctrl Pts',(9.80541358472588,-0.54645975548653,3.68178818330365));
#44277=CARTESIAN_POINT('Ctrl Pts',(9.85312942078873,-0.027892955418244,
3.36825716649128));
#44278=CARTESIAN_POINT('Ctrl Pts',(9.90084525685157,0.516288374798902,3.63486531430293));
#44279=CARTESIAN_POINT('Ctrl Pts',(9.9485610929144,0.58635414632045,4.2367822623095));
#44280=CARTESIAN_POINT('Ctrl Pts',(9.99627692897723,0.117961883057689,4.62125841547385));
#44281=CARTESIAN_POINT('Ctrl Pts',(10.0439927650401,-0.458756592493822,
4.4352234064191));
#44282=CARTESIAN_POINT('Ctrl Pts',(10.0917086011029,-0.614191830280748,
3.8495160464768));
#44283=CARTESIAN_POINT('Ctrl Pts',(10.1394244371658,-0.205605259764808,
3.40200041654811));
#44284=CARTESIAN_POINT('Ctrl Pts',(10.1871402732286,0.391791784436726,3.5036370055096));
#44285=CARTESIAN_POINT('Ctrl Pts',(10.2348561092915,0.629400404498524,4.06109136983801));
#44286=CARTESIAN_POINT('Ctrl Pts',(10.2825719453542,0.289020948539269,4.56244458923262));
#44287=CARTESIAN_POINT('Ctrl Pts',(10.3302877814171,-0.316770891622519,
4.54729628801251));
#44288=CARTESIAN_POINT('Ctrl Pts',(10.3780036174799,-0.631667147860668,
4.02955738427466));
#44289=CARTESIAN_POINT('Ctrl Pts',(10.4257194535428,-0.366493742769977,
3.48467547975859));
#44290=CARTESIAN_POINT('Ctrl Pts',(10.4734352896056,0.235236505537468,3.41302401146715));
#44291=CARTESIAN_POINT('Ctrl Pts',(10.5211511256685,0.620945451230968,3.88040162523195));
#44292=CARTESIAN_POINT('Ctrl Pts',(10.5688669617313,0.436430634585191,4.45760826680378));
#44293=CARTESIAN_POINT('Ctrl Pts',(10.6165827977941,-0.148865149148659,
4.61458619576145));
#44294=CARTESIAN_POINT('Ctrl Pts',(10.664298633857,-0.597455775834545,4.20718016452724));
#44295=CARTESIAN_POINT('Ctrl Pts',(10.7120144699198,-0.497393570532806,
3.60951740033105));
#44296=CARTESIAN_POINT('Ctrl Pts',(10.7597303059826,0.059432803973042,3.37044081575797));
#44297=CARTESIAN_POINT('Ctrl Pts',(10.8074461420455,0.56168112009921,3.70949811708754));
#44298=CARTESIAN_POINT('Ctrl Pts',(10.8551619781083,0.548129021063343,4.31532776744164));
#44299=CARTESIAN_POINT('Ctrl Pts',(10.9028778141712,0.0312216079359222,
4.63158707701274));
#44300=CARTESIAN_POINT('Ctrl Pts',(10.950593650234,-0.514357088165242,4.36785025554668));
#44301=CARTESIAN_POINT('Ctrl Pts',(10.9983094862968,-0.587593755803164,
3.7663108843084));
#44302=CARTESIAN_POINT('Ctrl Pts',(11.0460253223597,-0.12123403619496,3.37937182377895));
#44303=CARTESIAN_POINT('Ctrl Pts',(11.0937411584225,0.456456764276497,3.56236516706526));
#44304=CARTESIAN_POINT('Ctrl Pts',(11.1414569944854,0.61497629462275,4.14724531131301));
#44305=CARTESIAN_POINT('Ctrl Pts',(11.1891728305482,0.208753630990335,4.59690782052167));
#44306=CARTESIAN_POINT('Ctrl Pts',(11.236888666611,-0.389170704067994,4.49842069353791));
#44307=CARTESIAN_POINT('Ctrl Pts',(11.2846045026739,-0.629713593419695,
3.94222617449013));
#44308=CARTESIAN_POINT('Ctrl Pts',(11.3323203387367,-0.291980800545002,
3.43908624837263));
#44309=CARTESIAN_POINT('Ctrl Pts',(11.3800361747996,0.313882454172263,3.45104205114199));
#44310=CARTESIAN_POINT('Ctrl Pts',(11.4277520108624,0.631502621520784,3.96711438515144));
#44311=CARTESIAN_POINT('Ctrl Pts',(11.4754678469252,0.369204214609944,4.51338608528654));
#44312=CARTESIAN_POINT('Ctrl Pts',(11.5231836829881,-0.232140103514266,
4.58820744384271));
#44313=CARTESIAN_POINT('Ctrl Pts',(11.5708995190509,-0.620306592646703,
4.12286885598323));
#44314=CARTESIAN_POINT('Ctrl Pts',(11.6186153551137,-0.438835993107895,
3.54469790709399));
#44315=CARTESIAN_POINT('Ctrl Pts',(11.6663311911766,0.145624451261577,3.38463787584353));
#44316=CARTESIAN_POINT('Ctrl Pts',(11.7140470272394,0.596355721317347,3.78967435176932));
#44317=CARTESIAN_POINT('Ctrl Pts',(11.7617628633022,0.499444356375145,4.38785610674141));
#44318=CARTESIAN_POINT('Ctrl Pts',(11.8094786993651,-0.0561144459655822,
4.62986363095956));
#44319=CARTESIAN_POINT('Ctrl Pts',(11.8571945354279,-0.560142489144378,
4.29345769116983));
#44320=CARTESIAN_POINT('Ctrl Pts',(11.9049103714908,-0.549783065641843,
3.68756503815187));
#44321=CARTESIAN_POINT('Ctrl Pts',(11.9526262075536,-0.0345493934605723,
3.36858621802886));
#44322=CARTESIAN_POINT('Ctrl Pts',(12.0003420436164,0.512411518346294,3.62944438943981));
#44323=CARTESIAN_POINT('Ctrl Pts',(12.0480578796793,0.588817048391095,4.23058947975914));
#44324=CARTESIAN_POINT('Ctrl Pts',(12.0957737157421,0.1245028227835,4.61998070274044));
#44325=CARTESIAN_POINT('Ctrl Pts',(12.1434895518049,-0.454144260708352,
4.44003410676589));
#44326=CARTESIAN_POINT('Ctrl Pts',(12.1912053878678,-0.615743681684068,
3.85599741975318));
#44327=CARTESIAN_POINT('Ctrl Pts',(12.2389212239306,-0.211896205334937,
3.40420051794564));
#44328=CARTESIAN_POINT('Ctrl Pts',(12.2866370599935,0.386538816815474,3.49953544806202));
#44329=CARTESIAN_POINT('Ctrl Pts',(12.3343528960563,0.63000929582004,4.05445467686));
#44330=CARTESIAN_POINT('Ctrl Pts',(12.3820687321191,0.294932544534008,4.55936733800455));
#44331=CARTESIAN_POINT('Ctrl Pts',(12.429784568182,-0.310985300518122,4.55060436568669));
#44332=CARTESIAN_POINT('Ctrl Pts',(12.4775004042448,-0.631320558980542,
4.0362129322216));
#44333=CARTESIAN_POINT('Ctrl Pts',(12.5252162403077,-0.371904434015698,
3.48856660588983));
#44334=CARTESIAN_POINT('Ctrl Pts',(12.5729320763705,0.229037255191033,3.41057743478371));
#44335=CARTESIAN_POINT('Ctrl Pts',(12.6206479124333,0.619650508764677,3.87386407474765));
#44336=CARTESIAN_POINT('Ctrl Pts',(12.6683637484962,0.44122916559109,4.4529832757215));
#44337=CARTESIAN_POINT('Ctrl Pts',(12.716079584559,-0.142379709528176,4.61612096455669));
#44338=CARTESIAN_POINT('Ctrl Pts',(12.7637954206218,-0.595239106594286,
4.21346529139986));
#44339=CARTESIAN_POINT('Ctrl Pts',(12.8115112566847,-0.501481273143938,
3.61478115656484));
#44340=CARTESIAN_POINT('Ctrl Pts',(12.8592270927475,0.0527945297157079,
3.36984941301012));
#44341=CARTESIAN_POINT('Ctrl Pts',(12.9069429288104,0.558588303589165,3.70359464960132));
#44342=CARTESIAN_POINT('Ctrl Pts',(12.9546587648732,0.551421843290858,4.30953348024615));
#44343=CARTESIAN_POINT('Ctrl Pts',(13.002374600936,0.0378762195828894,4.63122295319618));
#44344=CARTESIAN_POINT('Ctrl Pts',(13.0500904369989,-0.510451719368595,
4.37325067561256));
#44345=CARTESIAN_POINT('Ctrl Pts',(13.0978062730617,-0.590023990114621,
3.77251655941407));
#44346=CARTESIAN_POINT('Ctrl Pts',(13.1455221091246,-0.127768152052348,
3.38068398698829));
#44347=CARTESIAN_POINT('Ctrl Pts',(13.1932379451874,0.451819146005312,3.55757883871291));
#44348=CARTESIAN_POINT('Ctrl Pts',(13.2409537812502,0.616493970155128,4.14075585037205));
#44349=CARTESIAN_POINT('Ctrl Pts',(13.2886696173131,0.215032895532453,4.59467459882739));
#44350=CARTESIAN_POINT('Ctrl Pts',(13.3363854533759,-0.383896195764066,
4.50249451293469));
#44351=CARTESIAN_POINT('Ctrl Pts',(13.3841012894387,-0.630287503488198,
3.94886598394213));
#44352=CARTESIAN_POINT('Ctrl Pts',(13.4318171255016,-0.297876098539286,
3.4421946086935));
#44353=CARTESIAN_POINT('Ctrl Pts',(13.4795329615644,0.308079511111167,3.44776450722078));
#44354=CARTESIAN_POINT('Ctrl Pts',(13.5272487976272,0.631120965295637,3.96046075600252));
#44355=CARTESIAN_POINT('Ctrl Pts',(13.5749646336901,0.374594326004835,4.50946650093658));
#44356=CARTESIAN_POINT('Ctrl Pts',(13.6226804697529,-0.225928046730791,
4.59062131891086));
#44357=CARTESIAN_POINT('Ctrl Pts',(13.6703963058158,-0.618977217803688,
4.12939949185215));
#44358=CARTESIAN_POINT('Ctrl Pts',(13.7181121418786,-0.443610085578744,
3.54934812035851));
#44359=CARTESIAN_POINT('Ctrl Pts',(13.7658279779415,0.139131014051702,3.38313730411011));
#44360=CARTESIAN_POINT('Ctrl Pts',(13.8135438140043,0.594105962672646,3.78340099315002));
#44361=CARTESIAN_POINT('Ctrl Pts',(13.8612596500671,0.503504264276035,4.38257088298437));
#44362=CARTESIAN_POINT('Ctrl Pts',(13.90897548613,-0.0494731474142026,4.63042004436449));
#44363=CARTESIAN_POINT('Ctrl Pts',(13.9566913221928,-0.557018606591754,
4.29934477874546));
#44364=CARTESIAN_POINT('Ctrl Pts',(14.0044071582556,-0.553045308503159,
3.69337659679301));
#44365=CARTESIAN_POINT('Ctrl Pts',(14.0521229943185,-0.0412019939202257,
3.36898540401303));
#44366=CARTESIAN_POINT('Ctrl Pts',(14.0998388303813,0.50847774565382,3.62406462413548));
#44367=CARTESIAN_POINT('Ctrl Pts',(14.1475546664442,0.591214547458171,4.22437108442359));
#44368=CARTESIAN_POINT('Ctrl Pts',(14.195270502507,0.131029933326566,4.61863412549262));
#44369=CARTESIAN_POINT('Ctrl Pts',(14.2429863385698,-0.4494814847335,4.44479593021223));
#44370=CARTESIAN_POINT('Ctrl Pts',(14.2907021746327,-0.617227139201166,
3.86249478815283));
#44371=CARTESIAN_POINT('Ctrl Pts',(14.3384180106955,-0.218163614480107,
3.40646679792233));
#44372=CARTESIAN_POINT('Ctrl Pts',(14.3861338467583,0.381242914296727,3.49548947984197));
#44373=CARTESIAN_POINT('Ctrl Pts',(14.4338496828212,0.630548208698617,4.0478119353149));
#44374=CARTESIAN_POINT('Ctrl Pts',(14.481565518884,0.300811380821271,4.55622795490698));
#44375=CARTESIAN_POINT('Ctrl Pts',(14.5292813549469,-0.305165166642291,
4.55385128484077));
#44376=CARTESIAN_POINT('Ctrl Pts',(14.5769971910097,-0.630903846008588,
4.04286445780787));
#44377=CARTESIAN_POINT('Ctrl Pts',(14.6247130270726,-0.37727381588172,3.49251453961553));
#44378=CARTESIAN_POINT('Ctrl Pts',(14.6724288631354,0.222812564473163,3.40819632836178));
#44379=CARTESIAN_POINT('Ctrl Pts',(14.7201446991982,0.618286738460357,3.86734053484336));
#44380=CARTESIAN_POINT('Ctrl Pts',(14.7678605352611,0.44597868695508,4.44830796940654));
#44381=CARTESIAN_POINT('Ctrl Pts',(14.8155763713239,-0.135878455045208,
4.6175872975589));
#44382=CARTESIAN_POINT('Ctrl Pts',(14.8632922073867,-0.592956321018707,
4.2197267075609));
#44383=CARTESIAN_POINT('Ctrl Pts',(14.9110080434496,-0.505513273594975,
3.62008770107973));
#44384=CARTESIAN_POINT('Ctrl Pts',(14.9587238795124,0.0461503912925444,
3.36932800439917));
#44385=CARTESIAN_POINT('Ctrl Pts',(15.0064397155752,0.555433441741075,3.69772410541485));
#44386=CARTESIAN_POINT('Ctrl Pts',(15.0541555516381,0.554653416196733,4.30370481154056));
#44387=CARTESIAN_POINT('Ctrl Pts',(15.1018713877009,0.0445266241191229,
4.63078871612938));
#44388=CARTESIAN_POINT('Ctrl Pts',(15.1495872237638,-0.506489652017253,
4.37860963676461));
#44389=CARTESIAN_POINT('Ctrl Pts',(15.1973030598266,-0.592388687361149,
3.77874750230084));
#44390=CARTESIAN_POINT('Ctrl Pts',(15.2450188958894,-0.134288076029725,
3.38206494088146));
#44391=CARTESIAN_POINT('Ctrl Pts',(15.2927347319523,0.447131341807447,3.5528416524037));
#44392=CARTESIAN_POINT('Ctrl Pts',(15.3404505680151,0.617943168462805,4.13425075493917));
#44393=CARTESIAN_POINT('Ctrl Pts',(15.3881664040779,0.221288275240951,4.59237532350063));
#44394=CARTESIAN_POINT('Ctrl Pts',(15.4358822401408,-0.378579046092452,
4.50651251762549));
#44395=CARTESIAN_POINT('Ctrl Pts',(15.4835980762036,-0.630791404211772,
3.95551147311801));
#44396=CARTESIAN_POINT('Ctrl Pts',(15.5313139122665,-0.303738309870084,
3.44536492739022));
#44397=CARTESIAN_POINT('Ctrl Pts',(15.5790297483293,0.302242348039936,3.44454830299756));
#44398=CARTESIAN_POINT('Ctrl Pts',(15.6267455843921,0.630669207148581,3.95381151868517));
#44399=CARTESIAN_POINT('Ctrl Pts',(15.674461420455,0.379942829239589,4.50549032746533));
#44400=CARTESIAN_POINT('Ctrl Pts',(15.7221772565178,-0.219690894932002,
4.59296959056563));
#44401=CARTESIAN_POINT('Ctrl Pts',(15.7698930925806,-0.617579089908608,
4.13591575463957));
#44402=CARTESIAN_POINT('Ctrl Pts',(15.8176089286435,-0.448334903946386,
3.5540483898953));
#44403=CARTESIAN_POINT('Ctrl Pts',(15.8653247647063,0.13262212282903,3.3817052505577));
#44404=CARTESIAN_POINT('Ctrl Pts',(15.9130406007692,0.591790213556878,3.77715169332057));
#44405=CARTESIAN_POINT('Ctrl Pts',(15.960756436832,0.507508245312566,4.37724316506909));
#44406=CARTESIAN_POINT('Ctrl Pts',(16.0084722728949,-0.0428263536203826,
4.63090643370248));
#44407=CARTESIAN_POINT('Ctrl Pts',(16.0561881089577,-0.553832853055588,
4.30519861652357));
#44408=CARTESIAN_POINT('Ctrl Pts',(16.1039039450205,-0.556246121716014,
3.69922221370673));
#44409=CARTESIAN_POINT('Ctrl Pts',(16.1516197810833,-0.0478500178579074,
3.36945468010413));
#44410=CARTESIAN_POINT('Ctrl Pts',(16.1993356171462,0.504487493666278,3.61872661594874));
#44411=CARTESIAN_POINT('Ctrl Pts',(16.247051453209,0.593546377218863,4.21812776701271));
#44412=CARTESIAN_POINT('Ctrl Pts',(16.2947672892719,0.137542489686435,4.61721883330181));
#44413=CARTESIAN_POINT('Ctrl Pts',(16.3424831253347,-0.444768782488292,
4.44950834783736));
#44414=CARTESIAN_POINT('Ctrl Pts',(16.3901989613976,-0.618642038056621,
3.86900742997889));
#44415=CARTESIAN_POINT('Ctrl Pts',(16.4379147974604,-0.224406791046256,
3.40879900475058));
#44416=CARTESIAN_POINT('Ctrl Pts',(16.4856306335233,0.375904665124208,3.49149955025639));
#44417=CARTESIAN_POINT('Ctrl Pts',(16.533346469586,0.631017083274371,4.04116388304691));
#44418=CARTESIAN_POINT('Ctrl Pts',(16.5810623056489,0.306656804407812,4.55302678864769));
#44419=CARTESIAN_POINT('Ctrl Pts',(16.6287781417117,-0.29931113646787,4.55703668482238));
#44420=CARTESIAN_POINT('Ctrl Pts',(16.6764939777746,-0.630417055231307,
4.04951122221356));
#44421=CARTESIAN_POINT('Ctrl Pts',(16.7242098138374,-0.382601291962586,
3.49651884241796));
#44422=CARTESIAN_POINT('Ctrl Pts',(16.7719256499003,0.216563124792967,3.40588095668335));
#44423=CARTESIAN_POINT('Ctrl Pts',(16.8196414859631,0.616854291799135,3.86083173012294));
#44424=CARTESIAN_POINT('Ctrl Pts',(16.8673573220259,0.450678671122871,4.44358286716973));
#44425=CARTESIAN_POINT('Ctrl Pts',(16.9150731580887,-0.129362107828251,
4.61898503189482));
#44426=CARTESIAN_POINT('Ctrl Pts',(16.9627889941516,-0.590607672668797,
4.22596371752193));
#44427=CARTESIAN_POINT('Ctrl Pts',(17.0105048302144,-0.509489124030439,
3.62543644444997));
#44428=CARTESIAN_POINT('Ctrl Pts',(17.0582206662773,0.0395011267029154,
3.3688766478407));
#44429=CARTESIAN_POINT('Ctrl Pts',(17.1059365023401,0.552216884982031,3.69188713660034));
#44430=CARTESIAN_POINT('Ctrl Pts',(17.153652338403,0.557823380833178,4.29784240874569));
#44431=CARTESIAN_POINT('Ctrl Pts',(17.2013681744658,0.0511720828492506,
4.63028441404532));
#44432=CARTESIAN_POINT('Ctrl Pts',(17.2490840105287,-0.502471326198846,
4.38392654375487));
#44433=CARTESIAN_POINT('Ctrl Pts',(17.2967998465914,-0.594687584883411,
3.78500302086511));
#44434=CARTESIAN_POINT('Ctrl Pts',(17.3445156826543,-0.140793083924855,
3.38351453206865));
#44435=CARTESIAN_POINT('Ctrl Pts',(17.3922315187171,0.442393872381948,3.5481541343218));
#44436=CARTESIAN_POINT('Ctrl Pts',(17.43994735478,0.61932372857571,4.1277307475695));
#44437=CARTESIAN_POINT('Ctrl Pts',(17.4876631908428,0.227519075297936,4.590010249934));
#44438=CARTESIAN_POINT('Ctrl Pts',(17.5353790269057,-0.373219845656906,
4.51047426130944));
#44439=CARTESIAN_POINT('Ctrl Pts',(17.5830948629685,-0.631225239619516,
3.96216190386831));
#44440=CARTESIAN_POINT('Ctrl Pts',(17.6308106990313,-0.309566783390781,
3.44859685231885));
#44441=CARTESIAN_POINT('Ctrl Pts',(17.6785265350942,0.29637161332294,3.44139379571298));
#44442=CARTESIAN_POINT('Ctrl Pts',(17.726242371157,0.630147397258769,3.94716741176515));
#44443=CARTESIAN_POINT('Ctrl Pts',(17.7739582072198,0.385249130227842,4.50145800652724));
#44444=CARTESIAN_POINT('Ctrl Pts',(17.8216740432827,-0.213429340911116,
4.59525199797214));
#44445=CARTESIAN_POINT('Ctrl Pts',(17.8693898793456,-0.616112364258878,
4.14241692054995));
#44446=CARTESIAN_POINT('Ctrl Pts',(17.9171057154084,-0.453009923400427,
3.55879819362073));
#44447=CARTESIAN_POINT('Ctrl Pts',(17.9648215514712,0.126098500570276,3.38034187425201));
#44448=CARTESIAN_POINT('Ctrl Pts',(18.012537387534,0.589408731192455,3.77092714642348));
#44449=CARTESIAN_POINT('Ctrl Pts',(18.0602532235969,0.511455854741549,4.3718735447732));
#44450=CARTESIAN_POINT('Ctrl Pts',(18.1079690596597,-0.0361748028784226,
4.6313227449477));
#44451=CARTESIAN_POINT('Ctrl Pts',(18.1556848957226,-0.55058558239424,4.31101855428765));
#44452=CARTESIAN_POINT('Ctrl Pts',(18.2034007317854,-0.559385149749292,
3.70510123958967));
#44453=CARTESIAN_POINT('Ctrl Pts',(18.2511165678482,-0.0544927268426965,
3.36999399417717));
#44454=CARTESIAN_POINT('Ctrl Pts',(18.2988324039111,0.500441205601937,3.6134309578002));
#44455=CARTESIAN_POINT('Ctrl Pts',(18.3465482399739,0.595812278664582,4.21186022100458));
#44456=CARTESIAN_POINT('Ctrl Pts',(18.3942640760367,0.144039768479226,4.61573498337195));
#44457=CARTESIAN_POINT('Ctrl Pts',(18.4419799120996,-0.440006677437314,
4.4541708362083));
#44458=CARTESIAN_POINT('Ctrl Pts',(18.4896957481624,-0.619988221090196,
3.87553462183804));
#44459=CARTESIAN_POINT('Ctrl Pts',(18.5374115842252,-0.230625041570952,
3.41119687937986));
#44460=CARTESIAN_POINT('Ctrl Pts',(18.5851274202881,0.370524662245315,3.48756610248778));
#44461=CARTESIAN_POINT('Ctrl Pts',(18.6328432563509,0.631415867466904,4.03451125849008));
#44462=CARTESIAN_POINT('Ctrl Pts',(18.6805590924138,0.31246816601179,4.54976419479712));
#44463=CARTESIAN_POINT('Ctrl Pts',(18.7282749284766,-0.293423860232864,
4.56016021181225));
#44464=CARTESIAN_POINT('Ctrl Pts',(18.7759907645394,-0.629860240718928,
4.05615248714788));
#44465=CARTESIAN_POINT('Ctrl Pts',(18.8237066006023,-0.387886270507855,
3.50057906951772));
#44466=CARTESIAN_POINT('Ctrl Pts',(18.8714224366651,0.210289630309142,3.40363157692976));
#44467=CARTESIAN_POINT('Ctrl Pts',(18.919138272728,0.615353327889266,3.85433838355196));
#44468=CARTESIAN_POINT('Ctrl Pts',(18.9668541087908,0.455328596044662,4.43880849385601));
#44469=CARTESIAN_POINT('Ctrl Pts',(19.0145699448537,-0.122831391686292,
4.62031401230505));
#44470=CARTESIAN_POINT('Ctrl Pts',(19.0622857809165,-0.588193422413584,
4.2321756285162));
#44471=CARTESIAN_POINT('Ctrl Pts',(19.1100016169793,-0.513408382846255,
3.63082679254236));
#44472=CARTESIAN_POINT('Ctrl Pts',(19.1577174530421,0.0328474745430158,
3.36849539350727));
#44473=CARTESIAN_POINT('Ctrl Pts',(19.205433289105,0.548938990540088,3.68608439142882));
#44474=CARTESIAN_POINT('Ctrl Pts',(19.2531491251678,0.560931385193363,4.2919469231649));
#44475=CARTESIAN_POINT('Ctrl Pts',(19.3008649612307,0.0578118574426247,
4.62971010270368));
#44476=CARTESIAN_POINT('Ctrl Pts',(19.3485807972935,-0.498397187901359,
4.38920080648958));
#44477=CARTESIAN_POINT('Ctrl Pts',(19.3962966333563,-0.596920427988996,
3.79128241936144));
#44478=CARTESIAN_POINT('Ctrl Pts',(19.4440124694192,-0.147282451949449,
3.38503260125846));
#44479=CARTESIAN_POINT('Ctrl Pts',(19.491728305482,0.437607261597584,3.54351680188243));
#44480=CARTESIAN_POINT('Ctrl Pts',(19.5394441415449,0.620635501579114,4.12119655861503));
#44481=CARTESIAN_POINT('Ctrl Pts',(19.5871599776077,0.233724595248439,4.58757962923414));
#44482=CARTESIAN_POINT('Ctrl Pts',(19.6348758136705,-0.367819173932889,
4.51437932582758));
#44483=CARTESIAN_POINT('Ctrl Pts',(19.6825916497334,-0.631588991354928,
3.96881649615688));
#44484=CARTESIAN_POINT('Ctrl Pts',(19.7303074857962,-0.315360815373557,
3.4518901025469));
#44485=CARTESIAN_POINT('Ctrl Pts',(19.778023321859,0.290467852693633,3.43830118837221));
#44486=CARTESIAN_POINT('Ctrl Pts',(19.8257391579219,0.629555794415491,3.94052945152661));
#44487=CARTESIAN_POINT('Ctrl Pts',(19.8734549939847,0.390512260364629,4.49736946054851));
#44488=CARTESIAN_POINT('Ctrl Pts',(19.9211708300476,-0.207143364153331,
4.59746927979605));
#44489=CARTESIAN_POINT('Ctrl Pts',(19.9688866661104,-0.61457855576007,4.14890039401813));
#44490=CARTESIAN_POINT('Ctrl Pts',(20.0166025021732,-0.45763207183192,3.5636005413983));
#44491=CARTESIAN_POINT('Ctrl Pts',(20.0643183382361,0.119556051622903,3.37904064719698));
#44492=CARTESIAN_POINT('Ctrl Pts',(20.1120341742989,0.586970881772813,3.7647406560623));
#44493=CARTESIAN_POINT('Ctrl Pts',(20.1597500103618,0.515329468049299,4.36643880344312));
#44494=CARTESIAN_POINT('Ctrl Pts',(20.2074658464246,-0.029486781418557,
4.63171390504007));
#44495=CARTESIAN_POINT('Ctrl Pts',(20.2551816824874,-0.547338447674763,
4.31671898245684));
#44496=CARTESIAN_POINT('Ctrl Pts',(20.3028975185503,-0.562346186529673,
3.71117381387971));
#44497=CARTESIAN_POINT('Ctrl Pts',(20.3506133546131,-0.0613491664957494,
3.37029669484294));
#44498=CARTESIAN_POINT('Ctrl Pts',(20.398329190676,0.496762641213801,3.60878154740643));
#44499=CARTESIAN_POINT('Ctrl Pts',(20.4380923873949,0.580417208789547,4.10498761157686));
#44500=CARTESIAN_POINT('Ctrl Pts',(20.4699029447702,0.374745574175769,4.41137453781958));
#44501=CARTESIAN_POINT('Ctrl Pts',(20.4937608628016,0.13332385162888,4.54159545884303));
#44502=CARTESIAN_POINT('Ctrl Pts',(20.517618780833,-0.143293564288956,4.53872805560682));
#44503=CARTESIAN_POINT('Ctrl Pts',(20.5414766988645,-0.38346854803195,4.40448715909776));
#44504=CARTESIAN_POINT('Ctrl Pts',(20.5653346168959,-0.530621786340447,
4.17114564603877));
#44505=CARTESIAN_POINT('Ctrl Pts',(20.5891925349273,-0.547627617499454,
3.89605651468078));
#44506=CARTESIAN_POINT('Ctrl Pts',(20.6130504529587,-0.430933317123153,
3.64633026976583));
#44507=CARTESIAN_POINT('Ctrl Pts',(20.6369083709901,-0.208752997660079,
3.48311457674551));
#44508=CARTESIAN_POINT('Ctrl Pts',(20.6607662890215,0.0644142843662171,
3.4462762657402));
#44509=CARTESIAN_POINT('Ctrl Pts',(20.684624207053,0.321861676845817,3.54484653226013));
#44510=CARTESIAN_POINT('Ctrl Pts',(20.7084821250844,0.500588620804837,3.75470996102831));
#44511=CARTESIAN_POINT('Ctrl Pts',(20.7323400431158,0.556916750317041,4.02455574134091));
#44512=CARTESIAN_POINT('Ctrl Pts',(20.7561979611472,0.47705893600668,4.28839577951569));
#44513=CARTESIAN_POINT('Ctrl Pts',(20.7800558791787,0.280549668164313,4.48171582646486));
#44514=CARTESIAN_POINT('Ctrl Pts',(20.8039137972101,0.0154370662995263,
4.55724289713534));
#44515=CARTESIAN_POINT('Ctrl Pts',(20.8277717152415,-0.253449631274377,
4.49650907789895));
#44516=CARTESIAN_POINT('Ctrl Pts',(20.8516296332729,-0.460361354274216,
4.31436517051053));
#44517=CARTESIAN_POINT('Ctrl Pts',(20.8754875513043,-0.554701993332711,
4.05535046556385));
#44518=CARTESIAN_POINT('Ctrl Pts',(20.8993454693358,-0.513402987365846,
3.78280103771366));
#44519=CARTESIAN_POINT('Ctrl Pts',(20.9232033873672,-0.346562912086465,
3.56336268648205));
#44520=CARTESIAN_POINT('Ctrl Pts',(20.9470613053986,-0.0949787932613798,
3.45069404477467));
#44521=CARTESIAN_POINT('Ctrl Pts',(20.97091922343,0.179830242856268,3.47234567582879));
#44522=CARTESIAN_POINT('Ctrl Pts',(20.9947771414614,0.410665878084123,3.62302316008453));
#44523=CARTESIAN_POINT('Ctrl Pts',(21.0186350594928,0.541082524061315,3.86588175144064));
#44524=CARTESIAN_POINT('Ctrl Pts',(21.0424929775243,0.539189751860116,4.14153590729571));
#44525=CARTESIAN_POINT('Ctrl Pts',(21.0663508955557,0.405450399288564,4.38258067876424));
#44526=CARTESIAN_POINT('Ctrl Pts',(21.0902088135871,0.172567379211795,4.53007405282339));
#44527=CARTESIAN_POINT('Ctrl Pts',(21.1140667316185,-0.102513065388571,
4.54794988212627));
#44528=CARTESIAN_POINT('Ctrl Pts',(21.1379246496499,-0.352526273278862,
4.43183703934844));
#44529=CARTESIAN_POINT('Ctrl Pts',(21.1617825676814,-0.516337204635697,
4.21012827746935));
#44530=CARTESIAN_POINT('Ctrl Pts',(21.1856404857128,-0.553889624765765,
3.93703742795684));
#44531=CARTESIAN_POINT('Ctrl Pts',(21.2094984037442,-0.456000943963824,
3.67934264238169));
#44532=CARTESIAN_POINT('Ctrl Pts',(21.2333563217756,-0.246607611160355,
3.50005731527167));
#44533=CARTESIAN_POINT('Ctrl Pts',(21.257214239807,0.0230880000356606,3.44302159274494));
#44534=CARTESIAN_POINT('Ctrl Pts',(21.2810721578385,0.287137966314551,3.52218226257825));
#44535=CARTESIAN_POINT('Ctrl Pts',(21.3049300758698,0.480974878350452,3.71818238470557));
#44536=CARTESIAN_POINT('Ctrl Pts',(21.3287879939013,0.557200331135927,3.9830945903298));
#44537=CARTESIAN_POINT('Ctrl Pts',(21.3526459119327,0.497175125126959,4.25214062911267));
#44538=CARTESIAN_POINT('Ctrl Pts',(21.3765038299641,0.31557705824565,4.45953141590455));
#44539=CARTESIAN_POINT('Ctrl Pts',(21.4003617479955,0.0568118044769688,
4.55455425412338));
#44540=CARTESIAN_POINT('Ctrl Pts',(21.424219666027,-0.215845483008899,4.51397347145443));
#44541=CARTESIAN_POINT('Ctrl Pts',(21.4480775840584,-0.435722670386138,
4.34771217465862));
#44542=CARTESIAN_POINT('Ctrl Pts',(21.4719355020898,-0.549053796006754,
4.0964257796693));
#44543=CARTESIAN_POINT('Ctrl Pts',(21.4957934201212,-0.528126312578589,
3.82156065496534));
#44544=CARTESIAN_POINT('Ctrl Pts',(21.5196513381527,-0.378057559853047,
3.59032881071252));
#44545=CARTESIAN_POINT('Ctrl Pts',(21.543509256184,-0.135543435662257,3.45927273145963));
#44546=CARTESIAN_POINT('Ctrl Pts',(21.5673671742155,0.14011475067701,3.46043919847993));
#44547=CARTESIAN_POINT('Ctrl Pts',(21.5912250922469,0.381511063826562,3.59354297881304));
#44548=CARTESIAN_POINT('Ctrl Pts',(21.6150830102783,0.529617529717794,3.8260365724933));
#44549=CARTESIAN_POINT('Ctrl Pts',(21.6389409283097,0.548218083101175,4.10106896286759));
#44550=CARTESIAN_POINT('Ctrl Pts',(21.6627988463412,0.432764382005563,4.35138723875747));
#44551=CARTESIAN_POINT('Ctrl Pts',(21.6866567643726,0.211488001244504,4.51578176317496));
#44552=CARTESIAN_POINT('Ctrl Pts',(21.710514682404,-0.0615029566383307,
4.55405359688301));
#44553=CARTESIAN_POINT('Ctrl Pts',(21.7343726004354,-0.319454766316188,
4.4568442340362));
#44554=CARTESIAN_POINT('Ctrl Pts',(21.7582305184669,-0.499291183856609,
4.24792401178047));
#44555=CARTESIAN_POINT('Ctrl Pts',(21.7820884364982,-0.557037306525311,
3.97837961532992));
#44556=CARTESIAN_POINT('Ctrl Pts',(21.8059463545297,-0.478572634356998,
3.71412199185867));
#44557=CARTESIAN_POINT('Ctrl Pts',(21.8298042725611,-0.283083917031579,
3.51976932853855));
#44558=CARTESIAN_POINT('Ctrl Pts',(21.8536621905926,-0.018373470940863,
3.44284614561161));
#44559=CARTESIAN_POINT('Ctrl Pts',(21.8775201086239,0.250829789278194,3.5021622566489));
#44560=CARTESIAN_POINT('Ctrl Pts',(21.9013780266554,0.458698333552465,3.68321325676341));
#44561=CARTESIAN_POINT('Ctrl Pts',(21.9252359446868,0.55440264058141,3.94172724469688));
#44562=CARTESIAN_POINT('Ctrl Pts',(21.9490938627182,0.514540400363477,4.21449050861997));
#44563=CARTESIAN_POINT('Ctrl Pts',(21.9729517807496,0.348859016457567,4.4348050005813));
#44564=CARTESIAN_POINT('Ctrl Pts',(21.996809698781,0.0978721002989983,4.54879782605011));
#44565=CARTESIAN_POINT('Ctrl Pts',(22.0206676168125,-0.177047210365213,
4.52859463409701));
#44566=CARTESIAN_POINT('Ctrl Pts',(22.0445255348439,-0.408673655425848,
4.3791356554785));
#44567=CARTESIAN_POINT('Ctrl Pts',(22.0683834528753,-0.540368259688198,
4.13696768164748));
#44568=CARTESIAN_POINT('Ctrl Pts',(22.0922413709067,-0.53992810512055,3.86130737872913));
#44569=CARTESIAN_POINT('Ctrl Pts',(22.1160992889381,-0.407460821505317,
3.61956119962225));
#44570=CARTESIAN_POINT('Ctrl Pts',(22.1399572069695,-0.175358268020808,
3.47084267015335));
#44571=CARTESIAN_POINT('Ctrl Pts',(22.163815125001,0.0996241586556461,3.45151752178681));
#44572=CARTESIAN_POINT('Ctrl Pts',(22.1876730430324,0.350245764837839,3.56631127970877));
#44573=CARTESIAN_POINT('Ctrl Pts',(22.2115309610638,0.51522274100534,3.78715374318048));
#44574=CARTESIAN_POINT('Ctrl Pts',(22.2353888790952,0.554213722627899,4.06004291426965));
#44575=CARTESIAN_POINT('Ctrl Pts',(22.2592467971266,0.457684352558003,4.31824995726588));
#44576=CARTESIAN_POINT('Ctrl Pts',(22.2831047151581,0.249238691275201,4.49863621678958));
#44577=CARTESIAN_POINT('Ctrl Pts',(22.3069626331895,-0.0201526192614011,
4.55709233866662));
#44578=CARTESIAN_POINT('Ctrl Pts',(22.3308205512209,-0.284616065231974,
4.47932420896945));
#44579=CARTESIAN_POINT('Ctrl Pts',(22.3546784692523,-0.479483130864429,
4.28434825342259));
#44580=CARTESIAN_POINT('Ctrl Pts',(22.3785363872838,-0.557103509392546,
4.01984140485232));
#44581=CARTESIAN_POINT('Ctrl Pts',(22.4023943053151,-0.498496906094933,
3.75048279151596));
#44582=CARTESIAN_POINT('Ctrl Pts',(22.4262522233466,-0.317994227800984,
3.542137933897));
#44583=CARTESIAN_POINT('Ctrl Pts',(22.450110141378,-0.0597333038680864,
3.44575282046209));
#44584=CARTESIAN_POINT('Ctrl Pts',(22.4739680594094,0.213134049493302,3.48489624527193));
#44585=CARTESIAN_POINT('Ctrl Pts',(22.4978259774408,0.433884304103661,3.6499965589521));
#44586=CARTESIAN_POINT('Ctrl Pts',(22.5216838954723,0.548538061567711,3.90068226732924));
#44587=CARTESIAN_POINT('Ctrl Pts',(22.5455418135037,0.529059256943919,4.17565382996358));
#44588=CARTESIAN_POINT('Ctrl Pts',(22.5693997315351,0.380211173855379,4.40767331583304));
#44589=CARTESIAN_POINT('Ctrl Pts',(22.5932576495665,0.138390873272415,4.54000544018811));
#44590=CARTESIAN_POINT('Ctrl Pts',(22.6171155675979,-0.137269333605106,
4.54029177230974));
#44591=CARTESIAN_POINT('Ctrl Pts',(22.6409734856293,-0.379364264814148,
4.40846158181013));
#44592=CARTESIAN_POINT('Ctrl Pts',(22.6648314036608,-0.528692759685234,
4.17675229015827));
#44593=CARTESIAN_POINT('Ctrl Pts',(22.6886893216921,-0.54874438127821,3.90182058373076));
#44594=CARTESIAN_POINT('Ctrl Pts',(22.7125472397236,-0.434607562942265,
3.65089956353622));
#44595=CARTESIAN_POINT('Ctrl Pts',(22.736405157755,-0.214207731687487,3.48533716867003));
#44596=CARTESIAN_POINT('Ctrl Pts',(22.7602630757864,0.0585913648593265,
3.44563509732658));
#44597=CARTESIAN_POINT('Ctrl Pts',(22.7841209938179,0.31702578011682,3.5414689143437));
#44598=CARTESIAN_POINT('Ctrl Pts',(22.8079789118493,0.498012898707086,3.74946820019106));
#44599=CARTESIAN_POINT('Ctrl Pts',(22.8238841905369,0.537376264140017,3.92891364167179));
#44600=CARTESIAN_POINT('Ctrl Pts',(22.8318368298807,0.534391234777113,4.01792167950194));
#44601=CARTESIAN_POINT('Ctrl Pts',(3.99999999999998,0.254694598474614,4.53673594206822));
#44602=CARTESIAN_POINT('Ctrl Pts',(4.00795263934379,0.165296026927429,4.57915779516171));
#44603=CARTESIAN_POINT('Ctrl Pts',(4.0238579180314,-0.0350146299391769,
4.61842892627033));
#44604=CARTESIAN_POINT('Ctrl Pts',(4.04771583606282,-0.327086058023631,
4.5259865276721));
#44605=CARTESIAN_POINT('Ctrl Pts',(4.07157375409423,-0.539100294705402,
4.30498302442502));
#44606=CARTESIAN_POINT('Ctrl Pts',(4.09543167212566,-0.619328256935644,
4.00937412827253));
#44607=CARTESIAN_POINT('Ctrl Pts',(4.11928959015708,-0.548093442686671,
3.71148804617917));
#44608=CARTESIAN_POINT('Ctrl Pts',(4.1431475081885,-0.342845496867427,3.48414304986991));
#44609=CARTESIAN_POINT('Ctrl Pts',(4.16700542621991,-0.0537568536316998,
3.38294333505492));
#44610=CARTESIAN_POINT('Ctrl Pts',(4.19086334425134,0.248473820944083,3.43262855616194));
#44611=CARTESIAN_POINT('Ctrl Pts',(4.21472126228276,0.489947458130694,3.62105272953394));
#44612=CARTESIAN_POINT('Ctrl Pts',(4.23857918031417,0.611614759069978,3.90213920826301));
#44613=CARTESIAN_POINT('Ctrl Pts',(4.26243709834559,0.583726034554802,4.20715564703007));
#44614=CARTESIAN_POINT('Ctrl Pts',(4.28629501637702,0.413100159498109,4.46151671210738));
#44615=CARTESIAN_POINT('Ctrl Pts',(4.31015293440843,0.141460167127662,4.60302446238992));
#44616=CARTESIAN_POINT('Ctrl Pts',(4.33401085243986,-0.164770755236008,
4.59707625642582));
#44617=CARTESIAN_POINT('Ctrl Pts',(4.35786877047126,-0.430710704813839,
4.44512666775742));
#44618=CARTESIAN_POINT('Ctrl Pts',(4.38172668850269,-0.59133017320549,4.18433147003372));
#44619=CARTESIAN_POINT('Ctrl Pts',(4.40558460653411,-0.607353296958831,
3.87846221409715));
#44620=CARTESIAN_POINT('Ctrl Pts',(4.42944252456553,-0.474862000813124,
3.60231225357117));
#44621=CARTESIAN_POINT('Ctrl Pts',(4.45330044259694,-0.226254007744579,
3.42340778189093));
#44622=CARTESIAN_POINT('Ctrl Pts',(4.47715836062837,0.0776792518003291,
3.38549581251083));
#44623=CARTESIAN_POINT('Ctrl Pts',(4.50101627865978,0.362617819109035,3.49784685630402));
#44624=CARTESIAN_POINT('Ctrl Pts',(4.5248741966912,0.558886451727075,3.73298802180378));
#44625=CARTESIAN_POINT('Ctrl Pts',(4.54873211472262,0.618492123352341,4.03342088939383));
#44626=CARTESIAN_POINT('Ctrl Pts',(4.57259003275404,0.5268596233165,4.32568143907503));
#44627=CARTESIAN_POINT('Ctrl Pts',(4.59644795078546,0.306395594072305,4.5383040055633));
#44628=CARTESIAN_POINT('Ctrl Pts',(4.62030586881688,0.0110094959969652,
4.61929657956068));
#44629=CARTESIAN_POINT('Ctrl Pts',(4.6441637868483,-0.287068723725306,4.54885427056805));
#44630=CARTESIAN_POINT('Ctrl Pts',(4.66802170487971,-0.514950820910697,
4.34420214192463));
#44631=CARTESIAN_POINT('Ctrl Pts',(4.69187962291114,-0.616913415399932,
4.05538321370614));
#44632=CARTESIAN_POINT('Ctrl Pts',(4.71573754094255,-0.568023875442366,
3.75302158112612));
#44633=CARTESIAN_POINT('Ctrl Pts',(4.73959545897398,-0.380237025278099,
3.51105289951885));
#44634=CARTESIAN_POINT('Ctrl Pts',(4.76345337700539,-0.0994718649854296,
3.38864510263028));
#44635=CARTESIAN_POINT('Ctrl Pts',(4.78731129503681,0.205616875855751,3.41573023112194));
#44636=CARTESIAN_POINT('Ctrl Pts',(4.81116921306823,0.460426689658758,3.5856852332931));
#44637=CARTESIAN_POINT('Ctrl Pts',(4.83502713109965,0.60264963606909,3.85695148163183));
#44638=CARTESIAN_POINT('Ctrl Pts',(4.85888504913107,0.597508330613982,4.16319698927494));
#44639=CARTESIAN_POINT('Ctrl Pts',(4.88274296716248,0.446259962523644,4.42953638764361));
#44640=CARTESIAN_POINT('Ctrl Pts',(4.90660088519391,0.185888877718945,4.59084243889714));
#44641=CARTESIAN_POINT('Ctrl Pts',(4.93045880322533,-0.119937101199393,
4.60767141961541));
#44642=CARTESIAN_POINT('Ctrl Pts',(4.95431672125674,-0.396435191853442,
4.47590818560059));
#44643=CARTESIAN_POINT('Ctrl Pts',(4.97817463928816,-0.575994079421511,
4.22777243672773));
#44644=CARTESIAN_POINT('Ctrl Pts',(5.00203255731958,-0.614706724807315,
3.92394012267834));
#44645=CARTESIAN_POINT('Ctrl Pts',(5.025890475351,-0.503106831702736,3.63870652046354));
#44646=CARTESIAN_POINT('Ctrl Pts',(5.04974839338242,-0.268483613891896,
3.44181901543221));
#44647=CARTESIAN_POINT('Ctrl Pts',(5.07360631141384,0.0317911608623165,
3.38142196567243));
#44648=CARTESIAN_POINT('Ctrl Pts',(5.09746422944526,0.32429213081186,3.47228409503311));
#44649=CARTESIAN_POINT('Ctrl Pts',(5.12132214747667,0.537494841237617,3.69218713785082));
#44650=CARTESIAN_POINT('Ctrl Pts',(5.1451800655081,0.619265421915264,3.98735881011802));
#44651=CARTESIAN_POINT('Ctrl Pts',(5.16903798353952,0.549608738483219,4.28562159765047));
#44652=CARTESIAN_POINT('Ctrl Pts',(5.19289590157094,0.34555774745058,4.51404212438126));
#44653=CARTESIAN_POINT('Ctrl Pts',(5.21675381960235,0.0570084743622218,
4.61676534947452));
#44654=CARTESIAN_POINT('Ctrl Pts',(5.24061173763377,-0.245480923587363,
4.56867264627043));
#44655=CARTESIAN_POINT('Ctrl Pts',(5.26446965566519,-0.487943548953736,
4.38152399072137));
#44656=CARTESIAN_POINT('Ctrl Pts',(5.28832757369661,-0.611090685285508,
4.10108232693608));
#44657=CARTESIAN_POINT('Ctrl Pts',(5.31218549172803,-0.584809503288917,
3.79592328078761));
#44658=CARTESIAN_POINT('Ctrl Pts',(5.33604340975945,-0.415526467847156,
3.5406665514248));
#44659=CARTESIAN_POINT('Ctrl Pts',(5.35990132779088,-0.144635892303038,
3.39772936223054));
#44660=CARTESIAN_POINT('Ctrl Pts',(5.38375924582228,0.161622098711782,3.40206374949372));
#44661=CARTESIAN_POINT('Ctrl Pts',(5.40761716385371,0.428359084093981,3.55260983746209));
#44662=CARTESIAN_POINT('Ctrl Pts',(5.43147508188512,0.590350605148055,3.81255500683439));
#44663=CARTESIAN_POINT('Ctrl Pts',(5.45533299991655,0.607985322415754,4.11833558293467));
#44664=CARTESIAN_POINT('Ctrl Pts',(5.47919091794796,0.476951067165249,4.39517988561105));
#44665=CARTESIAN_POINT('Ctrl Pts',(5.50304883597938,0.2292892841064,4.57539194177126));
#44666=CARTESIAN_POINT('Ctrl Pts',(5.5269067540108,-0.0744399746307492,
4.61490499480714));
#44667=CARTESIAN_POINT('Ctrl Pts',(5.55076467204222,-0.359966631867259,
4.5040570269359));
#44668=CARTESIAN_POINT('Ctrl Pts',(5.57462259007364,-0.55747164231658,4.26995338574299));
#44669=CARTESIAN_POINT('Ctrl Pts',(5.59848050810506,-0.618659650999605,
3.96983878834977));
#44670=CARTESIAN_POINT('Ctrl Pts',(5.62233842613648,-0.528568523057477,
3.67709942878664));
#44671=CARTESIAN_POINT('Ctrl Pts',(5.6461963441679,-0.309227993320144,3.46331805450751));
#44672=CARTESIAN_POINT('Ctrl Pts',(5.67005426219932,-0.0142727959960426,
3.38077003484781));
#44673=CARTESIAN_POINT('Ctrl Pts',(5.69391218023074,0.284172488697173,3.4496406091084));
#44674=CARTESIAN_POINT('Ctrl Pts',(5.71777009826216,0.513129859266986,3.65308904601577));
#44675=CARTESIAN_POINT('Ctrl Pts',(5.74162801629357,0.616613001744231,3.94136666067651));
#44676=CARTESIAN_POINT('Ctrl Pts',(5.765485934325,0.569317469330215,4.24398172424487));
#44677=CARTESIAN_POINT('Ctrl Pts',(5.78934385235641,0.382808307322586,4.48693660973462));
#44678=CARTESIAN_POINT('Ctrl Pts',(5.81320177038783,0.102692087527565,4.61082223133738));
#44679=CARTESIAN_POINT('Ctrl Pts',(5.83705968841925,-0.202535146533943,
4.58534517687525));
#44680=CARTESIAN_POINT('Ctrl Pts',(5.86091760645067,-0.458237017319611,
4.41673528603543));
#44681=CARTESIAN_POINT('Ctrl Pts',(5.88477552448209,-0.601887460912657,
4.14622225884759));
#44682=CARTESIAN_POINT('Ctrl Pts',(5.9086334425135,-0.598360014525416,3.83995392008642));
#44683=CARTESIAN_POINT('Ctrl Pts',(5.93249136054493,-0.448517265794504,
3.57282118150817));
#44684=CARTESIAN_POINT('Ctrl Pts',(5.95634927857635,-0.188999790056246,
3.41014534911766));
#44685=CARTESIAN_POINT('Ctrl Pts',(5.98020719660777,0.116733210556207,3.39170495376011));
#44686=CARTESIAN_POINT('Ctrl Pts',(6.00406511463918,0.393921897475357,3.52200944135141));
#44687=CARTESIAN_POINT('Ctrl Pts',(6.02792303267061,0.574785693380153,3.76919531120668));
#44688=CARTESIAN_POINT('Ctrl Pts',(6.05178095070201,0.61509921541814,4.07281983667942));
#44689=CARTESIAN_POINT('Ctrl Pts',(6.07563886873346,0.505003308517799,4.35863675364492));
#44690=CARTESIAN_POINT('Ctrl Pts',(6.09949678676485,0.27142206589204,4.55675943366228));
#44691=CARTESIAN_POINT('Ctrl Pts',(6.12335470479629,-0.0285325303540597,
4.61873507756083));
#44692=CARTESIAN_POINT('Ctrl Pts',(6.14721262282769,-0.321503980505702,
4.52942105023226));
#44693=CARTESIAN_POINT('Ctrl Pts',(6.17107054085913,-0.535870591003297,
4.31063422072759));
#44694=CARTESIAN_POINT('Ctrl Pts',(6.19492845889052,-0.619180264299368,
4.01591706164003));
#44695=CARTESIAN_POINT('Ctrl Pts',(6.21878637692196,-0.551125001039776,
3.71725450231754));
#44696=CARTESIAN_POINT('Ctrl Pts',(6.24264429495337,-0.348226295733882,
3.48783145534908));
#44697=CARTESIAN_POINT('Ctrl Pts',(6.2665022129848,-0.0603247367796791,
3.38345774569467));
#44698=CARTESIAN_POINT('Ctrl Pts',(6.29036013101621,0.242607149567705,3.43020375417728));
#44699=CARTESIAN_POINT('Ctrl Pts',(6.31421804904763,0.485688404846908,3.61560451082823));
#44700=CARTESIAN_POINT('Ctrl Pts',(6.33807596707905,0.61099356578022,3.89627130770405));
#44701=CARTESIAN_POINT('Ctrl Pts',(6.36193388511046,0.585080291527744,4.19994745529594));
#44702=CARTESIAN_POINT('Ctrl Pts',(6.3937444424857,0.363797450650833,4.54512657044717));
#44703=CARTESIAN_POINT('Ctrl Pts',(6.43350763920472,-0.178959141669374,
4.67939801199369));
#44704=CARTESIAN_POINT('Ctrl Pts',(6.48122347526757,-0.668951848353412,
4.21606826543601));
#44705=CARTESIAN_POINT('Ctrl Pts',(6.5289393113304,-0.543175254381078,3.55462676401443));
#44706=CARTESIAN_POINT('Ctrl Pts',(6.57665514739324,0.0806513803028556,
3.30201433154981));
#44707=CARTESIAN_POINT('Ctrl Pts',(6.62437098345608,0.630812951656228,3.69045991683978));
#44708=CARTESIAN_POINT('Ctrl Pts',(6.67208681951892,0.601478580142798,4.36311480674272));
#44709=CARTESIAN_POINT('Ctrl Pts',(6.71980265558175,0.0199087309838695,
4.70234020845997));
#44710=CARTESIAN_POINT('Ctrl Pts',(6.76751849164459,-0.580002689552455,
4.39658285339385));
#44711=CARTESIAN_POINT('Ctrl Pts',(6.81523432770743,-0.64725742864426,3.72664421308375));
#44712=CARTESIAN_POINT('Ctrl Pts',(6.86295016377027,-0.120142281411799,
3.30772876957018));
#44713=CARTESIAN_POINT('Ctrl Pts',(6.91066599983311,0.517310146858294,3.52453857056345));
#44714=CARTESIAN_POINT('Ctrl Pts',(6.95838183589594,0.679704059947864,4.17797090041396));
#44715=CARTESIAN_POINT('Ctrl Pts',(7.00609767195879,0.217917737520193,4.66797035296266));
#44716=CARTESIAN_POINT('Ctrl Pts',(7.05381350802161,-0.443987099894697,
4.54456206689342));
#44717=CARTESIAN_POINT('Ctrl Pts',(7.10152934408447,-0.698171061503544,
3.92107420680554));
#44718=CARTESIAN_POINT('Ctrl Pts',(7.14924518014729,-0.311214160204793,
3.3700650369752));
#44719=CARTESIAN_POINT('Ctrl Pts',(7.19696101621015,0.361535686685884,3.39753487888718));
#44720=CARTESIAN_POINT('Ctrl Pts',(7.24467685227297,0.702281647003851,3.97825768917858));
#44721=CARTESIAN_POINT('Ctrl Pts',(7.29239268833582,0.398111619195611,4.5789468099385));
#44722=CARTESIAN_POINT('Ctrl Pts',(7.34010852439865,-0.271650463017158,
4.64798016059173));
#44723=CARTESIAN_POINT('Ctrl Pts',(7.38782436046149,-0.691951729928866,
4.1219633626529));
#44724=CARTESIAN_POINT('Ctrl Pts',(7.43554019652432,-0.476823084268312,
3.48394573037578));
#44725=CARTESIAN_POINT('Ctrl Pts',(7.48325603258717,0.17617954081454,3.31982867534575));
#44726=CARTESIAN_POINT('Ctrl Pts',(7.53097186865001,0.667393780433987,3.78032341303133));
#44727=CARTESIAN_POINT('Ctrl Pts',(7.57868770471284,0.545730043505963,4.44255054095139));
#44728=CARTESIAN_POINT('Ctrl Pts',(7.62640354077568,-0.077085990144297,
4.69837669746149));
#44729=CARTESIAN_POINT('Ctrl Pts',(7.67411937683852,-0.629112772588521,
4.31287278685955));
#44730=CARTESIAN_POINT('Ctrl Pts',(7.72183521290136,-0.603415615998442,
3.64005298187887));
#44731=CARTESIAN_POINT('Ctrl Pts',(7.76955104896419,-0.0235926144000291,
3.29777806215626));
#44732=CARTESIAN_POINT('Ctrl Pts',(7.81726688502703,0.577895847971041,3.60036435301798));
#44733=CARTESIAN_POINT('Ctrl Pts',(7.86498272108987,0.648693661106154,4.26994220769392));
#44734=CARTESIAN_POINT('Ctrl Pts',(7.9126985571527,0.123786103798515,4.6916279794467));
#44735=CARTESIAN_POINT('Ctrl Pts',(7.96041439321555,-0.514796137313916,
4.47818113561083));
#44736=CARTESIAN_POINT('Ctrl Pts',(8.00813022927838,-0.680633164378164,
3.82561319718015));
#44737=CARTESIAN_POINT('Ctrl Pts',(8.05584606534123,-0.221434283704469,
3.33318734306526));
#44738=CARTESIAN_POINT('Ctrl Pts',(8.10356190140405,0.441111106898351,3.45310581204486));
#44739=CARTESIAN_POINT('Ctrl Pts',(8.1512777374669,0.698577380670183,4.07524562887252));
#44740=CARTESIAN_POINT('Ctrl Pts',(8.19899357352974,0.314529296777622,4.62828622690367));
#44741=CARTESIAN_POINT('Ctrl Pts',(8.24670940959258,-0.358355880000973,
4.60436191534297));
#44742=CARTESIAN_POINT('Ctrl Pts',(8.29442524565541,-0.70215733816079,4.02544275761943));
#44743=CARTESIAN_POINT('Ctrl Pts',(8.34214108171825,-0.401156908608127,
3.42315912408683));
#44744=CARTESIAN_POINT('Ctrl Pts',(8.3898569177811,0.268232082711808,3.35059734274305));
#44745=CARTESIAN_POINT('Ctrl Pts',(8.43757275384392,0.691299425196396,3.8743920139026));
#44746=CARTESIAN_POINT('Ctrl Pts',(8.48528858990677,0.479535868514212,4.51353443142269));
#44747=CARTESIAN_POINT('Ctrl Pts',(8.53300442596961,-0.172592854832336,
4.68109027882443));
#44748=CARTESIAN_POINT('Ctrl Pts',(8.58072026203244,-0.66622690390392,4.22319044326068));
#44749=CARTESIAN_POINT('Ctrl Pts',(8.62843609809529,-0.548054535901959,
3.56033138942427));
#44750=CARTESIAN_POINT('Ctrl Pts',(8.67615193415812,0.0734047453217555,
3.30122678585069));
#44751=CARTESIAN_POINT('Ctrl Pts',(8.72386777022095,0.627455319439314,3.68381637683837));
#44752=CARTESIAN_POINT('Ctrl Pts',(8.7715836062838,0.605304019074675,4.35676225408577));
#44753=CARTESIAN_POINT('Ctrl Pts',(8.81929944234663,0.0272927241942496,
4.70208786391332));
#44754=CARTESIAN_POINT('Ctrl Pts',(8.86701527840948,-0.575781899266294,
4.40267538529889));
#44755=CARTESIAN_POINT('Ctrl Pts',(8.9147311144723,-0.650107145087294,3.73347990440727));
#44756=CARTESIAN_POINT('Ctrl Pts',(8.96244695053515,-0.127428996390418,
3.30903392823725));
#44757=CARTESIAN_POINT('Ctrl Pts',(9.01016278659798,0.512269160438921,3.51911272764658));
#44758=CARTESIAN_POINT('Ctrl Pts',(9.05787862266082,0.681542664962993,4.17079770865984));
#44759=CARTESIAN_POINT('Ctrl Pts',(9.10559445872366,0.224945053369686,4.66563652575022));
#44760=CARTESIAN_POINT('Ctrl Pts',(9.1533102947865,-0.438223061957547,4.54921107910972));
#44761=CARTESIAN_POINT('Ctrl Pts',(9.20102613084934,-0.698964196560635,
3.92843664782408));
#44762=CARTESIAN_POINT('Ctrl Pts',(9.24874196691217,-0.317835754515511,
3.3733799439853));
#44763=CARTESIAN_POINT('Ctrl Pts',(9.29645780297501,0.355166151432911,3.39375807937372));
#44764=CARTESIAN_POINT('Ctrl Pts',(9.34417363903786,0.702013515586798,3.97085749870423));
#44765=CARTESIAN_POINT('Ctrl Pts',(9.39188947510068,0.404191066510942,4.57471892538967));
#44766=CARTESIAN_POINT('Ctrl Pts',(9.43960531116354,-0.264806258220881,
4.65080711970243));
#44767=CARTESIAN_POINT('Ctrl Pts',(9.48732114722635,-0.690627921460452,
4.12924912203773));
#44768=CARTESIAN_POINT('Ctrl Pts',(9.53503698328922,-0.482235337746388,
3.48899966685243));
#44769=CARTESIAN_POINT('Ctrl Pts',(9.58275281935202,0.169001376764621,3.31800968034731));
#44770=CARTESIAN_POINT('Ctrl Pts',(9.63046865541491,0.665041526572246,3.77330189814918));
#44771=CARTESIAN_POINT('Ctrl Pts',(9.6781844914777,0.550363809549371,4.43677447107931));
#44772=CARTESIAN_POINT('Ctrl Pts',(9.72590032754056,-0.0697214622184181,
4.69915032657822));
#44773=CARTESIAN_POINT('Ctrl Pts',(9.7736161636034,-0.625780442428439,4.31948567936979));
#44774=CARTESIAN_POINT('Ctrl Pts',(9.82133199966623,-0.607175613486645,
3.64643241687702));
#44775=CARTESIAN_POINT('Ctrl Pts',(9.86904783572907,-0.030992076082374,
3.29806570630264));
#44776=CARTESIAN_POINT('Ctrl Pts',(9.91676367179191,0.573651961662729,3.59429605827795));
#44777=CARTESIAN_POINT('Ctrl Pts',(9.96447950785474,0.651502576242943,4.26309058249416));
#44778=CARTESIAN_POINT('Ctrl Pts',(10.0121953439176,0.131068350403577,4.69028497663703));
#44779=CARTESIAN_POINT('Ctrl Pts',(10.0599111799804,-0.50972795835719,4.48358005533451));
#44780=CARTESIAN_POINT('Ctrl Pts',(10.1076270160433,-0.682433239785766,
3.83279612838271));
#44781=CARTESIAN_POINT('Ctrl Pts',(10.1553428521061,-0.228449576533966,
3.33555808949935));
#44782=CARTESIAN_POINT('Ctrl Pts',(10.2030586881689,0.435322847997542,3.44848728078164));
#44783=CARTESIAN_POINT('Ctrl Pts',(10.2507745242318,0.699331602909907,4.06787908823615));
#44784=CARTESIAN_POINT('Ctrl Pts',(10.2984903602946,0.321133386270249,4.62493648450936));
#44785=CARTESIAN_POINT('Ctrl Pts',(10.3462061963575,-0.351966560253669,
4.60810509117381));
#44786=CARTESIAN_POINT('Ctrl Pts',(10.3939220324203,-0.701850198794989,
4.03284143571381));
#44787=CARTESIAN_POINT('Ctrl Pts',(10.4416378684831,-0.407214000429435,
3.42741898450738));
#44788=CARTESIAN_POINT('Ctrl Pts',(10.489353704546,0.261373080323254,3.34780649011919));
#44789=CARTESIAN_POINT('Ctrl Pts',(10.5370695406088,0.689937239673316,3.86711333114163));
#44790=CARTESIAN_POINT('Ctrl Pts',(10.5847853766716,0.484921415782374,4.50845204490092));
#44791=CARTESIAN_POINT('Ctrl Pts',(10.6325012127345,-0.165405205696588,
4.68287142228737));
#44792=CARTESIAN_POINT('Ctrl Pts',(10.6802170487973,-0.66383768169814,4.23019946525991));
#44793=CARTESIAN_POINT('Ctrl Pts',(10.7279328848602,-0.552657800140614,
3.5661317972102));
#44794=CARTESIAN_POINT('Ctrl Pts',(10.775648720923,0.0660362430193439,3.30049197570278));
#44795=CARTESIAN_POINT('Ctrl Pts',(10.8233645569858,0.624088188116435,3.67722113622194));
#44796=CARTESIAN_POINT('Ctrl Pts',(10.8710803930487,0.609030347235101,4.3503630939397));
#44797=CARTESIAN_POINT('Ctrl Pts',(10.9187962291115,0.0346905673513346,
4.70176123146349));
#44798=CARTESIAN_POINT('Ctrl Pts',(10.9665120651743,-0.57150609431415,4.40872123214985));
#44799=CARTESIAN_POINT('Ctrl Pts',(11.0142279012372,-0.65287991581936,3.74034623636848));
#44800=CARTESIAN_POINT('Ctrl Pts',(11.0619437373,-0.134704064778877,3.31041528701663));
#44801=CARTESIAN_POINT('Ctrl Pts',(11.1096595733629,0.507172601636502,3.51374059022208));
#44802=CARTESIAN_POINT('Ctrl Pts',(11.1573754094257,0.68330486411552,4.16360539148934));
#44803=CARTESIAN_POINT('Ctrl Pts',(11.2050912454885,0.231947755880478,4.66322884435941));
#44804=CARTESIAN_POINT('Ctrl Pts',(11.2528070815514,-0.432410545554582,
4.55379904436673));
#44805=CARTESIAN_POINT('Ctrl Pts',(11.3005229176142,-0.699679589515398,
3.93580706063847));
#44806=CARTESIAN_POINT('Ctrl Pts',(11.348238753677,-0.324422100469907,3.37676444086124));
#44807=CARTESIAN_POINT('Ctrl Pts',(11.3959545897399,0.348757195312759,3.39004862475285));
#44808=CARTESIAN_POINT('Ctrl Pts',(11.4436704258027,0.701667392320496,3.9634605418422));
#44809=CARTESIAN_POINT('Ctrl Pts',(11.4913862618656,0.410225626419724,4.57042720558968));
#44810=CARTESIAN_POINT('Ctrl Pts',(11.5391020979284,-0.257932644354891,
4.65356178929341));
#44811=CARTESIAN_POINT('Ctrl Pts',(11.5868179339912,-0.689227399014534,
4.13652052554825));
#44812=CARTESIAN_POINT('Ctrl Pts',(11.6345337700541,-0.487594028032435,
3.49411036255383));
#44813=CARTESIAN_POINT('Ctrl Pts',(11.6822496061169,0.161804441490335,3.31626643773886));
#44814=CARTESIAN_POINT('Ctrl Pts',(11.7299654421798,0.662615402711184,3.76630556374144));
#44815=CARTESIAN_POINT('Ctrl Pts',(11.7776812782426,0.554936443973853,4.43094988641136));
#44816=CARTESIAN_POINT('Ctrl Pts',(11.8253971143054,-0.062349190059417,
4.69984629737339));
#44817=CARTESIAN_POINT('Ctrl Pts',(11.8731129503683,-0.622378603495518,
4.32606308493799));
#44818=CARTESIAN_POINT('Ctrl Pts',(11.9208287864311,-0.610868168815925,
3.65285112447858));
#44819=CARTESIAN_POINT('Ctrl Pts',(11.9685446224939,-0.0383880952977111,
3.29843131798253));
#44820=CARTESIAN_POINT('Ctrl Pts',(12.0162604585568,0.569344356809164,3.58827282720487));
#44821=CARTESIAN_POINT('Ctrl Pts',(12.0639762946196,0.654239125569198,4.25620973444184));
#44822=CARTESIAN_POINT('Ctrl Pts',(12.1116921306825,0.138336038556134,4.68886530024737));
#44823=CARTESIAN_POINT('Ctrl Pts',(12.1594079667453,-0.50460316123658,4.48892526128066));
#44824=CARTESIAN_POINT('Ctrl Pts',(12.2071238028081,-0.684157513748105,
3.83999763179777));
#44825=CARTESIAN_POINT('Ctrl Pts',(12.254839638871,-0.235439494268261,3.33800263898788));
#44826=CARTESIAN_POINT('Ctrl Pts',(12.3025554749338,0.429486235500398,3.44393000893412));
#44827=CARTESIAN_POINT('Ctrl Pts',(12.3502713109967,0.700008146713868,4.06050500791278));
#44828=CARTESIAN_POINT('Ctrl Pts',(12.3979871470595,0.327701805790174,4.62151732713591));
#44829=CARTESIAN_POINT('Ctrl Pts',(12.4457029831223,-0.345538145731053,
4.61178072157682));
#44830=CARTESIAN_POINT('Ctrl Pts',(12.4934188191852,-0.701465101239671,
4.04023646593735));
#44831=CARTESIAN_POINT('Ctrl Pts',(12.541134655248,-0.413225860851952,3.43174244451));
#44832=CARTESIAN_POINT('Ctrl Pts',(12.5888504913108,0.254485045853264,3.34508808005552));
#44833=CARTESIAN_POINT('Ctrl Pts',(12.6365663273737,0.688498419195676,3.85984940880123));
#44834=CARTESIAN_POINT('Ctrl Pts',(12.6842821634365,0.490253100280801,4.50331318193882));
#44835=CARTESIAN_POINT('Ctrl Pts',(12.7319979994994,-0.158199184135511,
4.68457671563321));
#44836=CARTESIAN_POINT('Ctrl Pts',(12.7797138355622,-0.661374723552845,
4.23718291779492));
#44837=CARTESIAN_POINT('Ctrl Pts',(12.827429671625,-0.557199677773407,3.57198039701723));
#44838=CARTESIAN_POINT('Ctrl Pts',(12.8751455076879,0.058660405724426,3.29983486358678));
#44839=CARTESIAN_POINT('Ctrl Pts',(12.9228613437507,0.62065173603916,3.67066174834999));
#44840=CARTESIAN_POINT('Ctrl Pts',(12.9705771798135,0.612689027194643,4.34392501712378));
#44841=CARTESIAN_POINT('Ctrl Pts',(13.0182930158764,0.0420845572448178,
4.7013566507062));
#44842=CARTESIAN_POINT('Ctrl Pts',(13.0660088519392,-0.567166809177069,
4.4147216801859));
#44843=CARTESIAN_POINT('Ctrl Pts',(13.1137246880021,-0.655580167748548,
3.74724140943759));
#44844=CARTESIAN_POINT('Ctrl Pts',(13.1614405240649,-0.141964170879043,
3.31187324159358));
#44845=CARTESIAN_POINT('Ctrl Pts',(13.2091563601277,0.502019708508231,3.50842246418533));
#44846=CARTESIAN_POINT('Ctrl Pts',(13.2568721961906,0.684991165006287,4.15639490180834));
#44847=CARTESIAN_POINT('Ctrl Pts',(13.3045880322534,0.238924694735218,4.66074749465585));
#44848=CARTESIAN_POINT('Ctrl Pts',(13.3523038683163,-0.426549999040181,
4.55832549625387));
#44849=CARTESIAN_POINT('Ctrl Pts',(13.4000197043791,-0.700317265381609,
3.94318460369993));
#44850=CARTESIAN_POINT('Ctrl Pts',(13.4477355404419,-0.330972411156884,
3.38021816378559));
#44851=CARTESIAN_POINT('Ctrl Pts',(13.4954513765048,0.342309500898352,3.3864069206363));
#44852=CARTESIAN_POINT('Ctrl Pts',(13.5431672125676,0.70124333116994,3.95606764360979));
#44853=CARTESIAN_POINT('Ctrl Pts',(13.5908830486304,0.416214620412595,4.5660721254426));
#44854=CARTESIAN_POINT('Ctrl Pts',(13.6385988846933,-0.251030380554765,
4.65624386434224));
#44855=CARTESIAN_POINT('Ctrl Pts',(13.6863147207561,-0.687750320459788,
4.14377676500662));
#44856=CARTESIAN_POINT('Ctrl Pts',(13.734030556819,-0.492898558687668,3.49927725007553));
#44857=CARTESIAN_POINT('Ctrl Pts',(13.7817463928818,0.15458953374652,3.31459914100992));
#44858=CARTESIAN_POINT('Ctrl Pts',(13.8294622289446,0.660115678675556,3.75933518700271));
#44859=CARTESIAN_POINT('Ctrl Pts',(13.8771780650075,0.559447438691528,4.42507743387505));
#44860=CARTESIAN_POINT('Ctrl Pts',(13.9248939010703,-0.0549699924482557,
4.7004645325629));
#44861=CARTESIAN_POINT('Ctrl Pts',(13.9726097371331,-0.61890763370075,4.33260427296601));
#44862=CARTESIAN_POINT('Ctrl Pts',(14.020325573196,-0.614492871807821,3.65930839172987));
#44863=CARTESIAN_POINT('Ctrl Pts',(14.0680414092588,-0.0457798505455885,
3.29887485658241));
#44864=CARTESIAN_POINT('Ctrl Pts',(14.1157572453217,0.564973511886205,3.58229532883235));
#44865=CARTESIAN_POINT('Ctrl Pts',(14.1634730813845,0.656903005118004,4.24930042782804));
#44866=CARTESIAN_POINT('Ctrl Pts',(14.2111889174473,0.145588360997982,4.6873691079691));
#44867=CARTESIAN_POINT('Ctrl Pts',(14.2589047535102,-0.499422315191365,
4.49421615972892));
#44868=CARTESIAN_POINT('Ctrl Pts',(14.306620589573,-0.685805794740406,3.8472169075166));
#44869=CARTESIAN_POINT('Ctrl Pts',(14.3543364256359,-0.242403260500786,
3.34052072000184));
#44870=CARTESIAN_POINT('Ctrl Pts',(14.4020522616987,0.423601917710294,3.43943450270243));
#44871=CARTESIAN_POINT('Ctrl Pts',(14.4497680977615,0.700606936934704,4.05312420698026));
#44872=CARTESIAN_POINT('Ctrl Pts',(14.4974839338244,0.334233825748585,4.61802913456711));
#44873=CARTESIAN_POINT('Ctrl Pts',(14.5451997698872,-0.339071350470923,
4.61538839828042));
#44874=CARTESIAN_POINT('Ctrl Pts',(14.59291560595,-0.701002088269634,4.04762702688518));
#44875=CARTESIAN_POINT('Ctrl Pts',(14.6406314420129,-0.419191822106764,
3.43612902386528));
#44876=CARTESIAN_POINT('Ctrl Pts',(14.6883472780757,0.24756874439201,3.34244241450009));
#44877=CARTESIAN_POINT('Ctrl Pts',(14.7360631141386,0.686983123580828,3.85260105372344));
#44878=CARTESIAN_POINT('Ctrl Pts',(14.7837789502014,0.495530329791292,4.49811841333687));
#44879=CARTESIAN_POINT('Ctrl Pts',(14.8314947862642,-0.150975590559777,
4.68620596944608));
#44880=CARTESIAN_POINT('Ctrl Pts',(14.8792106223271,-0.658838303041738,
4.24414002517693));
#44881=CARTESIAN_POINT('Ctrl Pts',(14.9269264583899,-0.561679664310124,
3.57787653921065));
#44882=CARTESIAN_POINT('Ctrl Pts',(14.9746422944528,0.0512780527100071,
3.29925552249156));
#44883=CARTESIAN_POINT('Ctrl Pts',(15.0223581305156,0.617146344912281,3.6641389418082));
#44884=CARTESIAN_POINT('Ctrl Pts',(15.0700739665784,0.616279652564493,4.337448738749));
#44885=CARTESIAN_POINT('Ctrl Pts',(15.1177898026413,0.0494738725853903,
4.70087416658037));
#44886=CARTESIAN_POINT('Ctrl Pts',(15.1655056387041,-0.562764525842253,
4.42067606290572));
#44887=CARTESIAN_POINT('Ctrl Pts',(15.2132214747669,-0.658207600943685,
3.75416465773151));
#44888=CARTESIAN_POINT('Ctrl Pts',(15.2609373108298,-0.14920850827279,3.31340763002542));
#44889=CARTESIAN_POINT('Ctrl Pts',(15.3086531468926,0.496811053413015,3.50315894024854));
#44890=CARTESIAN_POINT('Ctrl Pts',(15.3563689829554,0.686601380328997,4.14916704052379));
#44891=CARTESIAN_POINT('Ctrl Pts',(15.4040848190183,0.245875094968658,4.6581927522561));
#44892=CARTESIAN_POINT('Ctrl Pts',(15.4518006550811,-0.420642073376032,
4.56278993199436));
#44893=CARTESIAN_POINT('Ctrl Pts',(15.499516491144,-0.700877153329261,3.95056845754601));
#44894=CARTESIAN_POINT('Ctrl Pts',(15.5472323272068,-0.337485958999024,
3.3837407291352));
#44895=CARTESIAN_POINT('Ctrl Pts',(15.5949481632696,0.335823784368978,3.38283337152726));
#44896=CARTESIAN_POINT('Ctrl Pts',(15.6426639993325,0.70074137923783,3.94867962517506));
#44897=CARTESIAN_POINT('Ctrl Pts',(15.6903798353953,0.422157383260532,4.56165416869007));
#44898=CARTESIAN_POINT('Ctrl Pts',(15.7380956714582,-0.244100233491204,
4.65885304693675));
#44899=CARTESIAN_POINT('Ctrl Pts',(15.785811507521,-0.686196849863089,4.15101703442422));
#44900=CARTESIAN_POINT('Ctrl Pts',(15.8335273435838,-0.498148340509996,
3.50449975550414));
#44901=CARTESIAN_POINT('Ctrl Pts',(15.8812431796467,0.147357454930898,3.3130079753559));
#44902=CARTESIAN_POINT('Ctrl Pts',(15.9289590157095,0.657542632122849,3.75239154216938));
#44903=CARTESIAN_POINT('Ctrl Pts',(15.9766748517723,0.563896292642505,4.41915776575455));
#44904=CARTESIAN_POINT('Ctrl Pts',(16.0243906878352,-0.0475846890311933,
4.70100496347609));
#44905=CARTESIAN_POINT('Ctrl Pts',(16.072106523898,-0.615367918582998,4.33910851688972));
#44906=CARTESIAN_POINT('Ctrl Pts',(16.1198223599609,-0.618049319847516,
3.66580350138828));
#44907=CARTESIAN_POINT('Ctrl Pts',(16.1675381960237,-0.0531665207849041,
3.29939627283611));
#44908=CARTESIAN_POINT('Ctrl Pts',(16.2152540320865,0.560539912386559,3.57636422711252));
#44909=CARTESIAN_POINT('Ctrl Pts',(16.2629698681494,0.659493918998266,4.24236343010572));
#44910=CARTESIAN_POINT('Ctrl Pts',(16.3106857042122,0.152824512175573,4.68579656599215));
#44911=CARTESIAN_POINT('Ctrl Pts',(16.358401540275,-0.494185995685336,4.49945216299141));
#44912=CARTESIAN_POINT('Ctrl Pts',(16.4061173763379,-0.687377899679438,
3.85445315365633));
#44913=CARTESIAN_POINT('Ctrl Pts',(16.4538332124007,-0.249340101729437,
3.34311205284473));
#44914=CARTESIAN_POINT('Ctrl Pts',(16.5015490484636,0.417670548229327,3.43500126142608));
#44915=CARTESIAN_POINT('Ctrl Pts',(16.5492648845264,0.701127907061643,4.04573750526291));
#44916=CARTESIAN_POINT('Ctrl Pts',(16.5969807205892,0.340728720599694,4.61447229425484));
#44917=CARTESIAN_POINT('Ctrl Pts',(16.6446965566521,-0.3325668927742,4.61892772056098));
#44918=CARTESIAN_POINT('Ctrl Pts',(16.6924123927149,-0.700461211314163,
4.05501229764889));
#44919=CARTESIAN_POINT('Ctrl Pts',(16.7401282287777,-0.425111221523205,
3.4405782353328));
#44920=CARTESIAN_POINT('Ctrl Pts',(16.7878440648406,0.240624944169445,3.3398697873209));
#44921=CARTESIAN_POINT('Ctrl Pts',(16.8355599009034,0.685391521140609,3.84536907102113));
#44922=CARTESIAN_POINT('Ctrl Pts',(16.8832757369663,0.500752518144239,4.49286831610534));
#44923=CARTESIAN_POINT('Ctrl Pts',(16.9309915730291,-0.143735227331884,
4.68775900275617));
#44924=CARTESIAN_POINT('Ctrl Pts',(16.978707409092,-0.656228701898373,4.25107001464348));
#44925=CARTESIAN_POINT('Ctrl Pts',(17.0264232451548,-0.566097262135119,
3.58381956887496));
#44926=CARTESIAN_POINT('Ctrl Pts',(17.0741390812176,0.0438900039728252,
3.29875401676759));
#44927=CARTESIAN_POINT('Ctrl Pts',(17.1218549172805,0.613572404098014,3.65765344111895));
#44928=CARTESIAN_POINT('Ctrl Pts',(17.1695707533433,0.619801824515016,4.33093497816967));
#44929=CARTESIAN_POINT('Ctrl Pts',(17.2172865894061,0.0568576926029748,
4.70031383267802));
#44930=CARTESIAN_POINT('Ctrl Pts',(17.265002425469,-0.558299733294432,4.42658371892475));
#44931=CARTESIAN_POINT('Ctrl Pts',(17.3127182615318,-0.66076192356197,3.76111521224867));
#44932=CARTESIAN_POINT('Ctrl Pts',(17.3604340975947,-0.156436272293483,
3.31501828187956));
#44933=CARTESIAN_POINT('Ctrl Pts',(17.4081499336575,0.491547214903555,3.49795060305896));
#44934=CARTESIAN_POINT('Ctrl Pts',(17.4558657697204,0.688135331228569,4.14192261047223));
#44935=CARTESIAN_POINT('Ctrl Pts',(17.5035816057831,0.252798184563325,4.65556490092881));
#44936=CARTESIAN_POINT('Ctrl Pts',(17.551297441846,-0.414687424786488,4.56719185569987));
#44937=CARTESIAN_POINT('Ctrl Pts',(17.5990132779088,-0.701359191168653,
3.95795780201324));
#44938=CARTESIAN_POINT('Ctrl Pts',(17.6467291139717,-0.343962020502345,
3.38733174564023));
#44939=CARTESIAN_POINT('Ctrl Pts',(17.6944449500345,0.329300766127249,3.37932837435862));
#44940=CARTESIAN_POINT('Ctrl Pts',(17.7421607860974,0.700161592278611,3.94129730716402));
#44941=CARTESIAN_POINT('Ctrl Pts',(17.7898766221602,0.428053254869629,4.55717382605774));
#44942=CARTESIAN_POINT('Ctrl Pts',(17.837592458223,-0.23714297293205,4.66138904726133));
#44943=CARTESIAN_POINT('Ctrl Pts',(17.8853082942859,-0.684567159776581,
4.15824052958626));
#44944=CARTESIAN_POINT('Ctrl Pts',(17.9330241303487,-0.503342790378573,
3.50977729874859));
#44945=CARTESIAN_POINT('Ctrl Pts',(17.9807399664116,0.140109008348428,3.31149311751593));
#44946=CARTESIAN_POINT('Ctrl Pts',(18.0284558024744,0.654896548854854,3.7454754005085));
#44947=CARTESIAN_POINT('Ctrl Pts',(18.0761716385372,0.568282511669218,4.41319153957849));
#44948=CARTESIAN_POINT('Ctrl Pts',(18.1238874746001,-0.040194100132671,
4.70146753008449));
#44949=CARTESIAN_POINT('Ctrl Pts',(18.1716033106629,-0.611759851316993,
4.34557509424858));
#44950=CARTESIAN_POINT('Ctrl Pts',(18.2193191467258,-0.621537117901666,
3.67233573200791));
#44951=CARTESIAN_POINT('Ctrl Pts',(18.2670349827885,-0.0605472855394143,
3.29999550882718));
#44952=CARTESIAN_POINT('Ctrl Pts',(18.3147508188514,0.556044050773433,3.57048018084402));
#44953=CARTESIAN_POINT('Ctrl Pts',(18.3624666549143,0.662011579423562,4.23539951180373));
#44954=CARTESIAN_POINT('Ctrl Pts',(18.4101824909771,0.160043688331546,4.684147848987));
#44955=CARTESIAN_POINT('Ctrl Pts',(18.4578983270399,-0.488894784343999,
4.50463268947774));
#44956=CARTESIAN_POINT('Ctrl Pts',(18.5056141631028,-0.68887365394326,3.86170556644909));
#44957=CARTESIAN_POINT('Ctrl Pts',(18.5533299991656,-0.256249247442801,
3.34577634968359));
#44958=CARTESIAN_POINT('Ctrl Pts',(18.6010458352284,0.41169278588589,3.4306307775285));
#44959=CARTESIAN_POINT('Ctrl Pts',(18.6487616712913,0.701570999227752,4.03834572324048));
#44960=CARTESIAN_POINT('Ctrl Pts',(18.6964775073541,0.347185768921481,4.6108472012761));
#44961=CARTESIAN_POINT('Ctrl Pts',(18.744193343417,-0.326025495125306,4.62239829528727));
#44962=CARTESIAN_POINT('Ctrl Pts',(18.7919091794798,-0.699842530451103,
4.06239145790787));
#44963=CARTESIAN_POINT('Ctrl Pts',(18.8396250155426,-0.430983401602837,
3.44508958471478));
#44964=CARTESIAN_POINT('Ctrl Pts',(18.8873408516055,0.233654416470602,3.33737048427408));
#44965=CARTESIAN_POINT('Ctrl Pts',(18.9350566876683,0.683723788661416,3.83815426398688));
#44966=CARTESIAN_POINT('Ctrl Pts',(18.9827725237312,0.505919085286118,4.48756347340344));
#44967=CARTESIAN_POINT('Ctrl Pts',(19.030488359794,-0.136478898681533,4.68923564305365));
#44968=CARTESIAN_POINT('Ctrl Pts',(19.0782041958568,-0.653546209976322,
4.2579721164561));
#44969=CARTESIAN_POINT('Ctrl Pts',(19.1259200319197,-0.570451980578726,
3.58980882586423));
#44970=CARTESIAN_POINT('Ctrl Pts',(19.1736358679825,0.0364970801727598,
3.29833040216201));
#44971=CARTESIAN_POINT('Ctrl Pts',(19.2213517040453,0.609930310515188,3.65120596658116));
#44972=CARTESIAN_POINT('Ctrl Pts',(19.2690675401082,0.623255151928734,4.32438445905389));
#44973=CARTESIAN_POINT('Ctrl Pts',(19.316783376171,0.0642351969327414,4.69967571095415));
#44974=CARTESIAN_POINT('Ctrl Pts',(19.3644992122339,-0.553772927074266,
4.43244399258532));
#44975=CARTESIAN_POINT('Ctrl Pts',(19.4122150482967,-0.663242852612724,
3.76809229994096));
#44976=CARTESIAN_POINT('Ctrl Pts',(19.4599308843595,-0.163646658734412,
3.3167050201661));
#44977=CARTESIAN_POINT('Ctrl Pts',(19.5076467204224,0.486228775054438,3.49279802752061));
#44978=CARTESIAN_POINT('Ctrl Pts',(19.5553625564852,0.689592852244711,4.13466242315333));
#44979=CARTESIAN_POINT('Ctrl Pts',(19.6030783925481,0.259693185238344,4.65286421968052));
#44980=CARTESIAN_POINT('Ctrl Pts',(19.6507942286109,-0.408686697131164,
4.57153080275077));
#44981=CARTESIAN_POINT('Ctrl Pts',(19.6985100646738,-0.701763358503738,
3.96535177039745));
#44982=CARTESIAN_POINT('Ctrl Pts',(19.7462259007365,-0.350399813749482,
3.39099090115443));
#44983=CARTESIAN_POINT('Ctrl Pts',(19.7939417367994,0.322741052541778,3.37589215469092));
#44984=CARTESIAN_POINT('Ctrl Pts',(19.8416575728622,0.699504257835039,3.93392181877779));
#44985=CARTESIAN_POINT('Ctrl Pts',(19.8893734089251,0.433901159015506,4.55263101135276));
#44986=CARTESIAN_POINT('Ctrl Pts',(19.9370892449879,-0.23015857608315,4.663852686053));
#44987=CARTESIAN_POINT('Ctrl Pts',(19.9848050810507,-0.682862933423436,
4.16544436654047));
#44988=CARTESIAN_POINT('Ctrl Pts',(20.0325209171136,-0.508478494849655,
3.51511322409123));
#44989=CARTESIAN_POINT('Ctrl Pts',(20.0802367531764,0.132839643288252,3.31004731418368));
#44990=CARTESIAN_POINT('Ctrl Pts',(20.1279525892393,0.652187835720725,3.73860154375571));
#44991=CARTESIAN_POINT('Ctrl Pts',(20.1756684253021,0.572586513039731,4.4071529569233));
#44992=CARTESIAN_POINT('Ctrl Pts',(20.2233842613649,-0.0327629883405684,
4.70190215105461));
#44993=CARTESIAN_POINT('Ctrl Pts',(20.2711000974278,-0.608151935097038,
4.35190888358257));
#44994=CARTESIAN_POINT('Ctrl Pts',(20.3188159334906,-0.624827148513498,
3.67908301574286));
#44995=CARTESIAN_POINT('Ctrl Pts',(20.3665317695535,-0.0681655280739813,
3.30033184185188));
#44996=CARTESIAN_POINT('Ctrl Pts',(20.4142476056163,0.551956769749184,3.56531418539817));
#44997=CARTESIAN_POINT('Ctrl Pts',(20.4540108023353,0.644905999548395,4.11665253813788));
#44998=CARTESIAN_POINT('Ctrl Pts',(20.4858213597105,0.416382673412033,4.45708139504444));
#44999=CARTESIAN_POINT('Ctrl Pts',(20.509679277742,0.148137151166912,4.60177085628536));
#45000=CARTESIAN_POINT('Ctrl Pts',(20.5335371957734,-0.159214575149101,
4.59858486262053));
#45001=CARTESIAN_POINT('Ctrl Pts',(20.5573951138048,-0.426074836374489,
4.44942877587387));
#45002=CARTESIAN_POINT('Ctrl Pts',(20.5812530318362,-0.589577924844292,
4.19016123618585));
#45003=CARTESIAN_POINT('Ctrl Pts',(20.6051109498677,-0.608473233900696,
3.88450759853215));
#45004=CARTESIAN_POINT('Ctrl Pts',(20.6289688678991,-0.478813304308425,
3.60703485797333));
#45005=CARTESIAN_POINT('Ctrl Pts',(20.6528267859305,-0.231947052182395,
3.42568465323223));
#45006=CARTESIAN_POINT('Ctrl Pts',(20.6766847039619,0.0715712039811096,
3.38475332414555));
#45007=CARTESIAN_POINT('Ctrl Pts',(20.7005426219933,0.357622970648114,3.49427550111266));
#45008=CARTESIAN_POINT('Ctrl Pts',(20.7244005400248,0.556207844932749,3.72745636179159));
#45009=CARTESIAN_POINT('Ctrl Pts',(20.7482584580561,0.618794460414918,4.02728407199912));
#45010=CARTESIAN_POINT('Ctrl Pts',(20.7721163760876,0.530063832205264,4.32043875618714));
#45011=CARTESIAN_POINT('Ctrl Pts',(20.7959742941189,0.311720881859749,4.53523813880796));
#45012=CARTESIAN_POINT('Ctrl Pts',(20.8198322121505,0.01715224242355,4.619156844639));
#45013=CARTESIAN_POINT('Ctrl Pts',(20.8436901301818,-0.281609823618225,
4.55167503361081));
#45014=CARTESIAN_POINT('Ctrl Pts',(20.8675480482133,-0.511511021444125,
4.34929354512778));
#45015=CARTESIAN_POINT('Ctrl Pts',(20.8914059662447,-0.616333626991818,
4.06150032559224));
#45016=CARTESIAN_POINT('Ctrl Pts',(20.9152638842761,-0.570445985619195,
3.75866857192897));
#45017=CARTESIAN_POINT('Ctrl Pts',(20.9391218023075,-0.385068702031786,
3.51484894167474));
#45018=CARTESIAN_POINT('Ctrl Pts',(20.9629797203389,-0.105531663562905,
3.38966195221662));
#45019=CARTESIAN_POINT('Ctrl Pts',(20.9868376383704,0.199810758127152,3.41371924506628));
#45020=CARTESIAN_POINT('Ctrl Pts',(21.0106955564018,0.456293997792742,3.58113815016051));
#45021=CARTESIAN_POINT('Ctrl Pts',(21.0345534744332,0.60120093052663,3.85098018832832));
#45022=CARTESIAN_POINT('Ctrl Pts',(21.0584113924646,0.599097856858477,4.15726162902184));
#45023=CARTESIAN_POINT('Ctrl Pts',(21.082269310496,0.450499039416452,4.42508831804098));
#45024=CARTESIAN_POINT('Ctrl Pts',(21.1061272285275,0.191740934787398,4.58896933394457));
#45025=CARTESIAN_POINT('Ctrl Pts',(21.1299851465589,-0.113903050943465,
4.60883130459215));
#45026=CARTESIAN_POINT('Ctrl Pts',(21.1538430645903,-0.391694638258801,
4.47981743698434));
#45027=CARTESIAN_POINT('Ctrl Pts',(21.1777009826217,-0.573706216867813,
4.23347513609622));
#45028=CARTESIAN_POINT('Ctrl Pts',(21.2015589006531,-0.615430998064313,
3.9300418046833));
#45029=CARTESIAN_POINT('Ctrl Pts',(21.2254168186846,-0.506666136201032,
3.64371515765586));
#45030=CARTESIAN_POINT('Ctrl Pts',(21.2492747367159,-0.27400760274365,3.44450985958179));
#45031=CARTESIAN_POINT('Ctrl Pts',(21.2731326547474,0.0256532534100022,
3.38113703208972));
#45032=CARTESIAN_POINT('Ctrl Pts',(21.2969905727788,0.319041190319967,3.46909305773936));
#45033=CARTESIAN_POINT('Ctrl Pts',(21.3208484908102,0.534414865691478,3.68687029238709));
#45034=CARTESIAN_POINT('Ctrl Pts',(21.3447064088416,0.619109549231529,3.98121627002784));
#45035=CARTESIAN_POINT('Ctrl Pts',(21.3685643268731,0.552415083779586,4.28015538130547));
#45036=CARTESIAN_POINT('Ctrl Pts',(21.3924222449044,0.350640082858436,4.51058887057447));
#45037=CARTESIAN_POINT('Ctrl Pts',(21.4162801629359,0.0631240304344945,
4.61616947282646));
#45038=CARTESIAN_POINT('Ctrl Pts',(21.4401380809673,-0.239827566894842,
4.57107985485291));
#45039=CARTESIAN_POINT('Ctrl Pts',(21.4639959989987,-0.484134791346583,
4.38634565646493));
#45040=CARTESIAN_POINT('Ctrl Pts',(21.4878539170302,-0.610057871747176,
4.10713942122688));
#45041=CARTESIAN_POINT('Ctrl Pts',(21.5117118350615,-0.586805184862796,
3.80173467907963));
#45042=CARTESIAN_POINT('Ctrl Pts',(21.535569753093,-0.420062646027161,3.5448112085363));
#45043=CARTESIAN_POINT('Ctrl Pts',(21.5594276711244,-0.150603347961132,
3.39919379659958));
#45044=CARTESIAN_POINT('Ctrl Pts',(21.5832855891558,0.155682571034224,3.40048986702667));
#45045=CARTESIAN_POINT('Ctrl Pts',(21.6071435071872,0.423899860703612,3.54838249529388));
#45046=CARTESIAN_POINT('Ctrl Pts',(21.6310014252187,0.588462087630599,3.80670790527556));
#45047=CARTESIAN_POINT('Ctrl Pts',(21.6548593432501,0.609129304746478,4.11229849758833));
#45048=CARTESIAN_POINT('Ctrl Pts',(21.6787172612815,0.480847814502724,4.39042904829107));
#45049=CARTESIAN_POINT('Ctrl Pts',(21.7025751793129,0.234985935581564,4.57308906161293));
#45050=CARTESIAN_POINT('Ctrl Pts',(21.7264330973443,-0.0683364054776661,
4.61561318873779));
#45051=CARTESIAN_POINT('Ctrl Pts',(21.7502910153758,-0.35494863395129,4.5076031222497));
#45052=CARTESIAN_POINT('Ctrl Pts',(21.7741489334072,-0.554766252817153,
4.2754702655401));
#45053=CARTESIAN_POINT('Ctrl Pts',(21.7980068514386,-0.618928411339905,
3.9759774252466));
#45054=CARTESIAN_POINT('Ctrl Pts',(21.82186476947,-0.531745714018629,3.68235875884208));
#45055=CARTESIAN_POINT('Ctrl Pts',(21.8457226875014,-0.314536705157368,
3.46641202827438));
#45056=CARTESIAN_POINT('Ctrl Pts',(21.8695806055329,-0.0204149040773093,
3.3809420914381));
#45057=CARTESIAN_POINT('Ctrl Pts',(21.8934385235643,0.278698897140474,3.44684867604406));
#45058=CARTESIAN_POINT('Ctrl Pts',(21.9172964415957,0.509663226401888,3.6480158268968));
#45059=CARTESIAN_POINT('Ctrl Pts',(21.9411543596271,0.616001013860485,3.93525269592965));
#45060=CARTESIAN_POINT('Ctrl Pts',(21.9650122776585,0.571709773899469,4.23832204448885));
#45061=CARTESIAN_POINT('Ctrl Pts',(21.98887019569,0.387619921158457,4.48311516140836));
#45062=CARTESIAN_POINT('Ctrl Pts',(22.0127281137213,0.108746439139576,4.60977346157076));
#45063=CARTESIAN_POINT('Ctrl Pts',(22.0365860317528,-0.196718509442517,
4.5873255404835));
#45064=CARTESIAN_POINT('Ctrl Pts',(22.0604439497842,-0.454080423961193,
4.42126052632156));
#45065=CARTESIAN_POINT('Ctrl Pts',(22.0843018678156,-0.600407305919173,
4.15218583856754));
#45066=CARTESIAN_POINT('Ctrl Pts',(22.1081597858471,-0.599918246812857,
3.84589756782496));
#45067=CARTESIAN_POINT('Ctrl Pts',(22.1320177038785,-0.452732834916613,
3.57729153941473));
#45068=CARTESIAN_POINT('Ctrl Pts',(22.1558756219099,-0.194841912687001,
3.41204924396571));
#45069=CARTESIAN_POINT('Ctrl Pts',(22.1797335399413,0.110693164578993,3.39057692382254));
#45070=CARTESIAN_POINT('Ctrl Pts',(22.2035914579728,0.389160747889314,3.51812514615901));
#45071=CARTESIAN_POINT('Ctrl Pts',(22.2274493760041,0.572467927805029,3.76350489626149));
#45072=CARTESIAN_POINT('Ctrl Pts',(22.2513072940356,0.615791105677536,4.06671414123586));
#45073=CARTESIAN_POINT('Ctrl Pts',(22.2751652120669,0.508536584364246,4.35360996140145));
#45074=CARTESIAN_POINT('Ctrl Pts',(22.2990231300984,0.276931015980992,4.55403851389998));
#45075=CARTESIAN_POINT('Ctrl Pts',(22.3228810481298,-0.0223917293827815,
4.61898955797298));
#45076=CARTESIAN_POINT('Ctrl Pts',(22.3467389661613,-0.31623908674035,4.53258079431836));
#45077=CARTESIAN_POINT('Ctrl Pts',(22.3705968841927,-0.532757373651304,
4.31594151899069));
#45078=CARTESIAN_POINT('Ctrl Pts',(22.3944548022241,-0.619001969851995,
4.02204593667267));
#45079=CARTESIAN_POINT('Ctrl Pts',(22.4183127202555,-0.553883724721699,
3.72275952141814));
#45080=CARTESIAN_POINT('Ctrl Pts',(22.4421706382869,-0.35332581843718,3.49126595675675));
#45081=CARTESIAN_POINT('Ctrl Pts',(22.4660285563184,-0.0663701307507445,
3.38417172009386));
#45082=CARTESIAN_POINT('Ctrl Pts',(22.4898864743497,0.236814872379406,3.42766427875767));
#45083=CARTESIAN_POINT('Ctrl Pts',(22.5137443923812,0.482092168510832,3.61110849992699));
#45084=CARTESIAN_POINT('Ctrl Pts',(22.5376023104126,0.609484835267769,3.88964730767638));
#45085=CARTESIAN_POINT('Ctrl Pts',(22.561460228444,0.587841786482003,4.19517031382209));
#45086=CARTESIAN_POINT('Ctrl Pts',(22.5853181464754,0.422455543015367,4.45296893898932));
#45087=CARTESIAN_POINT('Ctrl Pts',(22.6091760645069,0.153767157666155,4.60000417439789));
#45088=CARTESIAN_POINT('Ctrl Pts',(22.6330339825383,-0.152521006364708,
4.60032232020799));
#45089=CARTESIAN_POINT('Ctrl Pts',(22.6568919005697,-0.421514535902825,
4.45384478734481));
#45090=CARTESIAN_POINT('Ctrl Pts',(22.6807498186011,-0.587434568575047,
4.19639082134502));
#45091=CARTESIAN_POINT('Ctrl Pts',(22.7046077366325,-0.60971407867596,3.89091209973551));
#45092=CARTESIAN_POINT('Ctrl Pts',(22.728465654664,-0.482895786937606,3.61211183522625));
#45093=CARTESIAN_POINT('Ctrl Pts',(22.7523235726954,-0.23800784887647,3.4281541921173));
#45094=CARTESIAN_POINT('Ctrl Pts',(22.7761814907268,0.0651013135850054,
3.38404091701771));
#45095=CARTESIAN_POINT('Ctrl Pts',(22.8000394087582,0.352249768808992,3.49052260401466));
#45096=CARTESIAN_POINT('Ctrl Pts',(22.8238973267896,0.553345940411564,3.72163220123786));
#45097=CARTESIAN_POINT('Ctrl Pts',(22.8398026054772,0.597082876783669,3.92101540361374));
#45098=CARTESIAN_POINT('Ctrl Pts',(22.847755244821,0.593766187829899,4.01991291515446));
#45099=CARTESIAN_POINT('',(22.8,0.337479661717902,3.51106003648017));
#45100=CARTESIAN_POINT('Ctrl Pts',(22.8,0.337504360408405,3.51101527402275));
#45101=CARTESIAN_POINT('Ctrl Pts',(22.8,0.337610992569967,3.51114843896934));
#45102=CARTESIAN_POINT('Ctrl Pts',(22.8,0.337717562131928,3.51128164981369));
#45103=CARTESIAN_POINT('Ctrl Pts',(22.8,0.337824069051012,3.51141490653789));
#45104=CARTESIAN_POINT('Ctrl Pts',(22.8,0.354145371784291,3.53183539523119));
#45105=CARTESIAN_POINT('Ctrl Pts',(22.8,0.368999739942303,3.55333386321799));
#45106=CARTESIAN_POINT('Ctrl Pts',(22.8,0.382262544471458,3.57576050230915));
#45107=CARTESIAN_POINT('Ctrl Pts',(22.8,0.395177725624396,3.59759933027929));
#45108=CARTESIAN_POINT('Ctrl Pts',(22.8,0.406583379369087,3.62031953557487));
#45109=CARTESIAN_POINT('Ctrl Pts',(22.8,0.416319965152677,3.64376476659274));
#45110=CARTESIAN_POINT('Ctrl Pts',(22.8,0.420499854003763,3.65382973822867));
#45111=CARTESIAN_POINT('Ctrl Pts',(22.8,0.424371599987778,3.66402799385056));
#45112=CARTESIAN_POINT('Ctrl Pts',(22.8,0.42792023461967,3.67434527679585));
#45113=CARTESIAN_POINT('Ctrl Pts',(22.8,0.430015882150509,3.68043815216119));
#45114=CARTESIAN_POINT('Ctrl Pts',(22.8,0.431995626466768,3.68656321156818));
#45115=CARTESIAN_POINT('Ctrl Pts',(22.8,0.433857425300493,3.69271766785326));
#45116=CARTESIAN_POINT('Ctrl Pts',(22.8,0.440667704273582,3.71523007009016));
#45117=CARTESIAN_POINT('Ctrl Pts',(22.8,0.445903532435623,3.73813926926309));
#45118=CARTESIAN_POINT('Ctrl Pts',(22.8,0.449441836754149,3.76130640751661));
#45119=CARTESIAN_POINT('Ctrl Pts',(22.8,0.450038513826676,3.76521316594877));
#45120=CARTESIAN_POINT('Ctrl Pts',(22.8,0.450586822418701,3.76912718643627));
#45121=CARTESIAN_POINT('Ctrl Pts',(22.8,0.451086059471329,3.77304770583064));
#45122=CARTESIAN_POINT('Ctrl Pts',(22.8,0.453684096906641,3.79345015011803));
#45123=CARTESIAN_POINT('Ctrl Pts',(22.8,0.454954433743694,3.81403106227893));
#45124=CARTESIAN_POINT('Ctrl Pts',(22.8,0.45484641916779,3.83463783350426));
#45125=CARTESIAN_POINT('Ctrl Pts',(22.8,0.454808390965019,3.84189276616533));
#45126=CARTESIAN_POINT('Ctrl Pts',(22.8,0.454599381710613,3.84915061719132));
#45127=CARTESIAN_POINT('Ctrl Pts',(22.8,0.454216814112443,3.8564037154462));
#45128=CARTESIAN_POINT('Ctrl Pts',(22.8,0.453866695925276,3.86304160538904));
#45129=CARTESIAN_POINT('Ctrl Pts',(22.8,0.453371644107099,3.86966645154658));
#45130=CARTESIAN_POINT('Ctrl Pts',(22.8,0.452731182295137,3.87626933737115));
#45131=CARTESIAN_POINT('Ctrl Pts',(22.8,0.450713457978438,3.89707120727158));
#45132=CARTESIAN_POINT('Ctrl Pts',(22.8,0.447253508643,3.9176725514372));
#45133=CARTESIAN_POINT('Ctrl Pts',(22.8,0.442312061254715,3.9379035771693));
#45134=CARTESIAN_POINT('Ctrl Pts',(22.8,0.437564183511961,3.95734209977996));
#45135=CARTESIAN_POINT('Ctrl Pts',(22.8,0.431447509288203,3.97643919003209));
#45136=CARTESIAN_POINT('Ctrl Pts',(22.8,0.423915075143768,3.9949978423605));
#45137=CARTESIAN_POINT('Ctrl Pts',(22.8,0.421325190817866,4.00137888225459));
#45138=CARTESIAN_POINT('Ctrl Pts',(22.8,0.418567902041021,4.00769582483512));
#45139=CARTESIAN_POINT('Ctrl Pts',(22.8,0.415641328671541,4.01393920819689));
#45140=CARTESIAN_POINT('Ctrl Pts',(22.6211545887425,-1.51173456864708E-7,
4.59404872180247));
#45141=CARTESIAN_POINT('Ctrl Pts',(22.6251143866744,-0.0492822808754852,
4.59404929162283));
#45142=CARTESIAN_POINT('Ctrl Pts',(22.6290741846063,-0.0985642856931001,
4.58798571459226));
#45143=CARTESIAN_POINT('Ctrl Pts',(22.6330339825383,-0.14630523394925,4.57585637376244));
#45144=CARTESIAN_POINT('Ctrl Pts',(22.6409866218821,-0.242185516210759,
4.55149647592026));
#45145=CARTESIAN_POINT('Ctrl Pts',(22.6489392612259,-0.331850026056775,
4.50267063163255));
#45146=CARTESIAN_POINT('Ctrl Pts',(22.6568919005697,-0.404335619758509,
4.43534871515538));
#45147=CARTESIAN_POINT('Ctrl Pts',(22.6648445399135,-0.476821213460227,
4.36802679867822));
#45148=CARTESIAN_POINT('Ctrl Pts',(22.6727971792573,-0.532127891017642,
4.28220881001161));
#45149=CARTESIAN_POINT('Ctrl Pts',(22.6807498186011,-0.563494481479829,
4.18838669541007));
#45150=CARTESIAN_POINT('Ctrl Pts',(22.6887024579449,-0.594861071942019,
4.09456458080851));
#45151=CARTESIAN_POINT('Ctrl Pts',(22.6966550972887,-0.602287575308989,
3.99273834027202));
#45152=CARTESIAN_POINT('Ctrl Pts',(22.7046077366325,-0.584864445036083,
3.89535850925222));
#45153=CARTESIAN_POINT('Ctrl Pts',(22.7125603759763,-0.567441314763176,
3.79797867823242));
#45154=CARTESIAN_POINT('Ctrl Pts',(22.7205130153201,-0.525168550850394,
3.70504525672934));
#45155=CARTESIAN_POINT('Ctrl Pts',(22.7284656546639,-0.463217512550482,
3.62791893879298));
#45156=CARTESIAN_POINT('Ctrl Pts',(22.7364182940078,-0.401266474250563,
3.5507926208566));
#45157=CARTESIAN_POINT('Ctrl Pts',(22.7443709333516,-0.319637161563486,
3.48947340648693));
#45158=CARTESIAN_POINT('Ctrl Pts',(22.7523235726954,-0.228304311476372,
3.45146158678551));
#45159=CARTESIAN_POINT('Ctrl Pts',(22.7602762120392,-0.136971461389268,
3.41344976708409));
#45160=CARTESIAN_POINT('Ctrl Pts',(22.768228851383,-0.0359350739021178,
3.3987453420509));
#45161=CARTESIAN_POINT('Ctrl Pts',(22.7761814907268,0.062441195712126,3.40914007736714));
#45162=CARTESIAN_POINT('Ctrl Pts',(22.7841209938178,0.160654966376612,3.41951764255099));
#45163=CARTESIAN_POINT('Ctrl Pts',(22.7920604969089,0.256217399931083,3.45491151845628));
#45164=CARTESIAN_POINT('Ctrl Pts',(22.8,0.337504360408238,3.51101527402264));
#45165=CARTESIAN_POINT('Ctrl Pts',(4.,-0.219914231356244,4.35301468169996));
#45166=CARTESIAN_POINT('Ctrl Pts',(4.00793950309107,-0.278596966840389,
4.31645650682028));
#45167=CARTESIAN_POINT('Ctrl Pts',(4.02383164552594,-0.377405665439666,
4.21337674819164));
#45168=CARTESIAN_POINT('Ctrl Pts',(4.04767642730463,-0.433534992178268,
4.00656196868444));
#45169=CARTESIAN_POINT('Ctrl Pts',(4.07153434533603,-0.383670022685343,
3.79803920418254));
#45170=CARTESIAN_POINT('Ctrl Pts',(4.09539226336747,-0.239994733226421,
3.63889579340969));
#45171=CARTESIAN_POINT('Ctrl Pts',(4.11925018139887,-0.0376302499649443,
3.56805514133307));
#45172=CARTESIAN_POINT('Ctrl Pts',(4.1431080994303,0.173933765839147,3.60283521426327));
#45173=CARTESIAN_POINT('Ctrl Pts',(4.16696601746172,0.342967344134064,3.73473372141871));
#45174=CARTESIAN_POINT('Ctrl Pts',(4.19082393549313,0.428135478754777,3.93149662217858));
#45175=CARTESIAN_POINT('Ctrl Pts',(4.21468185352456,0.40861313688017,4.1450106963618));
#45176=CARTESIAN_POINT('Ctrl Pts',(4.23853977155597,0.289173588337559,4.32306558264197));
#45177=CARTESIAN_POINT('Ctrl Pts',(4.25811226835493,0.13317859508208,4.40432939198872));
#45178=CARTESIAN_POINT('Ctrl Pts',(4.26973212581007,0.0319512750557707,
4.41584666103033));
#45179=CARTESIAN_POINT('Ctrl Pts',(4.2733993439214,2.51014653359152E-6,
4.41583996132385));
#45180=CARTESIAN_POINT('Origin',(3.42660065607856,0.,4.));
#45181=CARTESIAN_POINT('Ctrl Pts',(4.,-0.219892372743211,3.64701365460636));
#45182=CARTESIAN_POINT('Ctrl Pts',(4.00795263934381,-0.161099076858729,
3.61038844940468));
#45183=CARTESIAN_POINT('Ctrl Pts',(4.02385791803142,-0.0249198690254346,
3.56711791692558));
#45184=CARTESIAN_POINT('Ctrl Pts',(4.04771583606284,0.185569069288609,3.60813812632505));
#45185=CARTESIAN_POINT('Ctrl Pts',(4.07157375409426,0.350624105231944,3.74494568050885));
#45186=CARTESIAN_POINT('Ctrl Pts',(4.09543167212568,0.429971014252744,3.94413788601839));
#45187=CARTESIAN_POINT('Ctrl Pts',(4.1192895901571,0.40416308778273,4.15698104289539));
#45188=CARTESIAN_POINT('Ctrl Pts',(4.14314750818851,0.279534313346206,4.3314427366163));
#45189=CARTESIAN_POINT('Ctrl Pts',(4.16225119682902,0.125004509401131,4.40624063703925));
#45190=CARTESIAN_POINT('Ctrl Pts',(4.1734022461257,0.0278694809177792,4.41585864517498));
#45191=CARTESIAN_POINT('Ctrl Pts',(4.17660065607858,5.88453344126799E-6,
4.41584444980552));
#45192=CARTESIAN_POINT('Ctrl Pts',(3.95224475517896,-0.314128184302177,
3.49573985500833));
#45193=CARTESIAN_POINT('Ctrl Pts',(3.96019739452277,-0.230138771413741,
3.44341876234755));
#45194=CARTESIAN_POINT('Ctrl Pts',(3.97610267321038,-0.0355993848822847,
3.38160445914153));
#45195=CARTESIAN_POINT('Ctrl Pts',(3.9999605912418,0.265095483172694,3.44020405374152));
#45196=CARTESIAN_POINT('Ctrl Pts',(4.02381850927322,0.500885556761892,3.63564106712445));
#45197=CARTESIAN_POINT('Ctrl Pts',(4.04767642730465,0.614236921112272,3.92019793948569));
#45198=CARTESIAN_POINT('Ctrl Pts',(4.07153434533605,0.577368897990231,4.22425593648149));
#45199=CARTESIAN_POINT('Ctrl Pts',(4.09539226336749,0.399329932212592,4.47348393104611));
#45200=CARTESIAN_POINT('Ctrl Pts',(4.11925018139889,0.123637843932736,4.60692867011962));
#45201=CARTESIAN_POINT('Ctrl Pts',(4.14310809943032,-0.182283847264271,
4.59196468982869));
#45202=CARTESIAN_POINT('Ctrl Pts',(4.16696601746173,-0.443633876576525,
4.43224822622665));
#45203=CARTESIAN_POINT('Ctrl Pts',(4.19082393549315,-0.596502436238336,
4.16683582239239));
#45204=CARTESIAN_POINT('Ctrl Pts',(4.21468185352458,-0.603510379797736,
3.86062723727387));
#45205=CARTESIAN_POINT('Ctrl Pts',(4.23853977155598,-0.462943343075553,
3.58849923641164));
#45206=CARTESIAN_POINT('Ctrl Pts',(4.26239768958742,-0.209174182705692,
3.41699430327496));
#45207=CARTESIAN_POINT('Ctrl Pts',(4.28625560761882,0.0957438341235747,
3.38805018506757));
#45208=CARTESIAN_POINT('Ctrl Pts',(4.31011352565025,0.377249837899377,3.50874444390425));
#45209=CARTESIAN_POINT('Ctrl Pts',(4.33397144368167,0.566508000142931,3.7495640793295));
#45210=CARTESIAN_POINT('Ctrl Pts',(4.35782936171309,0.617239514437223,4.05162211295782));
#45211=CARTESIAN_POINT('Ctrl Pts',(4.3816872797445,0.517039159770137,4.34105713706075));
#45212=CARTESIAN_POINT('Ctrl Pts',(4.40554519777592,0.290408643717306,4.54709439922074));
#45213=CARTESIAN_POINT('Ctrl Pts',(4.42940311580735,-0.00723469473045889,
4.61935217913086));
#45214=CARTESIAN_POINT('Ctrl Pts',(4.45326103383876,-0.303108954077165,
4.54016147994594));
#45215=CARTESIAN_POINT('Ctrl Pts',(4.47711895187019,-0.524864817190473,
4.3288865854667));
#45216=CARTESIAN_POINT('Ctrl Pts',(4.5009768699016,-0.618276935702851,4.03718996201469));
#45217=CARTESIAN_POINT('Ctrl Pts',(4.52483478793302,-0.560503501787052,
3.7363993798876));
#45218=CARTESIAN_POINT('Ctrl Pts',(4.54869270596444,-0.365671693940747,
3.50006632967672));
#45219=CARTESIAN_POINT('Ctrl Pts',(4.57255062399586,-0.0814231961944085,
3.38598067979976));
#45220=CARTESIAN_POINT('Ctrl Pts',(4.59640854202727,0.222735490926488,3.42203947925158));
#45221=CARTESIAN_POINT('Ctrl Pts',(4.6202664600587,0.472429283332598,3.59942536936051));
#45222=CARTESIAN_POINT('Ctrl Pts',(4.64412437809011,0.606601247243452,3.87476266809168));
#45223=CARTESIAN_POINT('Ctrl Pts',(4.66798229612153,0.592442682719785,4.18072390587243));
#45224=CARTESIAN_POINT('Ctrl Pts',(4.69184021415295,0.433415744455024,4.44249322584619));
#45225=CARTESIAN_POINT('Ctrl Pts',(4.71569813218437,0.168406850663934,4.59606089882753));
#45226=CARTESIAN_POINT('Ctrl Pts',(4.7395560502158,-0.1377821054254,4.60387544567241));
#45227=CARTESIAN_POINT('Ctrl Pts',(4.7634139682472,-0.410279583628813,4.46402599681362));
#45228=CARTESIAN_POINT('Ctrl Pts',(4.78727188627863,-0.582452527843622,
4.21070955191949));
#45229=CARTESIAN_POINT('Ctrl Pts',(4.81112980431005,-0.612199963312297,
3.9058688819681));
#45230=CARTESIAN_POINT('Ctrl Pts',(4.83498772234147,-0.492247831758966,
3.62404583445569));
#45231=CARTESIAN_POINT('Ctrl Pts',(4.85884564037289,-0.251927696778831,
3.4341538212047));
#45232=CARTESIAN_POINT('Ctrl Pts',(4.88270355840431,0.0499956224363984,
3.38262661200963));
#45233=CARTESIAN_POINT('Ctrl Pts',(4.90656147643572,0.339693650112522,3.48206401309162));
#45234=CARTESIAN_POINT('Ctrl Pts',(4.93041939446714,0.546327327266884,3.70815087126575));
#45235=CARTESIAN_POINT('Ctrl Pts',(4.95427731249857,0.619369091246891,4.00560279122603));
#45236=CARTESIAN_POINT('Ctrl Pts',(4.97813523052998,0.540958241141728,4.3016846761146));
#45237=CARTESIAN_POINT('Ctrl Pts',(5.00199314856141,0.330268365670778,4.52399643996756));
#45238=CARTESIAN_POINT('Ctrl Pts',(5.02585106659282,0.0388188784636707,
4.61817680087201));
#45239=CARTESIAN_POINT('Ctrl Pts',(5.04970898462424,-0.262122881932824,
4.56119609516527));
#45240=CARTESIAN_POINT('Ctrl Pts',(5.07356690265566,-0.498968457612796,
4.36698765751594));
#45241=CARTESIAN_POINT('Ctrl Pts',(5.09742482068708,-0.613802653778546,
4.08304074106085));
#45242=CARTESIAN_POINT('Ctrl Pts',(5.12128273871849,-0.578545381446849,
3.77878810143205));
#45243=CARTESIAN_POINT('Ctrl Pts',(5.14514065674992,-0.40181800409162,3.52862779669421));
#45244=CARTESIAN_POINT('Ctrl Pts',(5.16899857478133,-0.126835179433317,
3.39373083558568));
#45245=CARTESIAN_POINT('Ctrl Pts',(5.19285649281276,0.179162301517353,3.4070831996169));
#45246=CARTESIAN_POINT('Ctrl Pts',(5.21671441084417,0.441349719463922,3.56541987207117));
#45247=CARTESIAN_POINT('Ctrl Pts',(5.24057232887559,0.595615108876583,3.83002322352904));
#45248=CARTESIAN_POINT('Ctrl Pts',(5.26443024690701,0.604236379939102,4.13619052690848));
#45249=CARTESIAN_POINT('Ctrl Pts',(5.28828816493843,0.465105397037983,4.40905553670335));
#45250=CARTESIAN_POINT('Ctrl Pts',(5.31214608296985,0.21224347534444,4.58189532532512));
#45251=CARTESIAN_POINT('Ctrl Pts',(5.33600400100126,-0.0925177574670201,
4.61244585639451));
#45252=CARTESIAN_POINT('Ctrl Pts',(5.35986191903269,-0.37465587844466,4.49323669288525));
#45253=CARTESIAN_POINT('Ctrl Pts',(5.3837198370641,-0.565180431721392,4.25341772246777));
#45254=CARTESIAN_POINT('Ctrl Pts',(5.40757775509553,-0.617502974236318,
3.95163121594683));
#45255=CARTESIAN_POINT('Ctrl Pts',(5.43143567312694,-0.518829219107294,
3.66167219466597));
#45256=CARTESIAN_POINT('Ctrl Pts',(5.45529359115837,-0.293287587282116,
3.45444353765392));
#45257=CARTESIAN_POINT('Ctrl Pts',(5.47915150918978,0.00397084862654925,
3.38061829634467));
#45258=CARTESIAN_POINT('Ctrl Pts',(5.50300942722121,0.300258303883157,3.45824875319892));
#45259=CARTESIAN_POINT('Ctrl Pts',(5.52686734525262,0.523124424966688,3.66835214690199));
#45260=CARTESIAN_POINT('Ctrl Pts',(5.55072526328404,0.618072374525773,3.95955247459688));
#45261=CARTESIAN_POINT('Ctrl Pts',(5.57458318131546,0.561884792553919,4.26064332401524));
#45262=CARTESIAN_POINT('Ctrl Pts',(5.59844109934688,0.368301073379394,4.49799978094171));
#45263=CARTESIAN_POINT('Ctrl Pts',(5.62229901737829,0.0846577094226282,
4.61358172616469));
#45264=CARTESIAN_POINT('Ctrl Pts',(5.64615693540972,-0.219686770477705,
4.57912622575047));
#45265=CARTESIAN_POINT('Ctrl Pts',(5.67001485344113,-0.470311850924231,
4.40305858798173));
#45266=CARTESIAN_POINT('Ctrl Pts',(5.69387277147256,-0.605932872639677,
4.12843214650112));
#45267=CARTESIAN_POINT('Ctrl Pts',(5.71773068950397,-0.593386801983745,
3.82240054650545));
#45268=CARTESIAN_POINT('Ctrl Pts',(5.74158860753539,-0.435741494202748,
3.55979685111874));
#45269=CARTESIAN_POINT('Ctrl Pts',(5.76544652556682,-0.171545522688555,
3.40483481554927));
#45270=CARTESIAN_POINT('Ctrl Pts',(5.78930444359822,0.134598003740687,3.39540688139736));
#45271=CARTESIAN_POINT('Ctrl Pts',(5.81316236162965,0.407828648458881,3.53381843004554));
#45272=CARTESIAN_POINT('Ctrl Pts',(5.83702027966106,0.58133408605803,3.78622407765735));
#45273=CARTESIAN_POINT('Ctrl Pts',(5.86087819769249,0.612687492198482,4.09090374899912));
#45274=CARTESIAN_POINT('Ctrl Pts',(5.8847361157239,0.494222140250734,4.3733550009975));
#45275=CARTESIAN_POINT('Ctrl Pts',(5.90859403375532,0.254905969192102,4.56451074097759));
#45276=CARTESIAN_POINT('Ctrl Pts',(5.93245195178675,-0.0467415727364197,
4.61762831145024));
#45277=CARTESIAN_POINT('Ctrl Pts',(5.95630986981815,-0.336959681931401,
4.51971877801409));
#45278=CARTESIAN_POINT('Ctrl Pts',(5.98016778784959,-0.544781677596122,
4.29472414464893));
#45279=CARTESIAN_POINT('Ctrl Pts',(6.00402570588099,-0.61939026621187,3.99766086682344));
#45280=CARTESIAN_POINT('Ctrl Pts',(6.02788362391242,-0.542540019317823,
3.70117063377655));
#45281=CARTESIAN_POINT('Ctrl Pts',(6.05174154194384,-0.333025929677459,
3.47775031355921));
#45282=CARTESIAN_POINT('Ctrl Pts',(6.07559945997526,-0.042074208138152,
3.38203805739984));
#45283=CARTESIAN_POINT('Ctrl Pts',(6.09945737800668,0.259158778028439,3.43742717299816));
#45284=CARTESIAN_POINT('Ctrl Pts',(6.12331529603809,0.497033648893269,3.63039418124561));
#45285=CARTESIAN_POINT('Ctrl Pts',(6.14717321406952,0.613345206175343,3.91371436613889));
#45286=CARTESIAN_POINT('Ctrl Pts',(6.17103113210093,0.579724447951105,4.21818191418763));
#45287=CARTESIAN_POINT('Ctrl Pts',(6.19488905013236,0.40425597056565,4.46920707734689));
#45288=CARTESIAN_POINT('Ctrl Pts',(6.21874696816377,0.13010450107023,4.60567007851858));
#45289=CARTESIAN_POINT('Ctrl Pts',(6.24260488619519,-0.176179318911185,
4.59370602015056));
#45290=CARTESIAN_POINT('Ctrl Pts',(6.26646280422661,-0.438782409775579,
4.43717629804221));
#45291=CARTESIAN_POINT('Ctrl Pts',(6.29032072225803,-0.595217424383659,
4.17259489198797));
#45292=CARTESIAN_POINT('Ctrl Pts',(6.31417864028945,-0.604035436411749,
3.86794272465182));
#45293=CARTESIAN_POINT('Ctrl Pts',(6.34598919766468,-0.423477061217623,
3.4998212904071));
#45294=CARTESIAN_POINT('Ctrl Pts',(6.3857523943837,0.100470573235224,3.30464850830547));
#45295=CARTESIAN_POINT('Ctrl Pts',(6.43346823044655,0.640013163212275,3.70919899990029));
#45296=CARTESIAN_POINT('Ctrl Pts',(6.48118406650937,0.590335835129396,4.3806576914582));
#45297=CARTESIAN_POINT('Ctrl Pts',(6.52889990257223,-0.000686065451295705,
4.70262946694599));
#45298=CARTESIAN_POINT('Ctrl Pts',(6.57661573863505,-0.591483599613884,
4.37932465573422));
#45299=CARTESIAN_POINT('Ctrl Pts',(6.6243315746979,-0.638898060441451,3.70770201230499));
#45300=CARTESIAN_POINT('Ctrl Pts',(6.67204741076074,-0.0997162142428727,
3.30448953810453));
#45301=CARTESIAN_POINT('Ctrl Pts',(6.71976324682356,0.531096731682035,3.53998115137447));
#45302=CARTESIAN_POINT('Ctrl Pts',(6.76747908288643,0.674163513320998,4.19791190586338));
#45303=CARTESIAN_POINT('Ctrl Pts',(6.81519491894923,0.19815244237474,4.67409883091767));
#45304=CARTESIAN_POINT('Ctrl Pts',(6.86291075501209,-0.459834002450772,
4.53124951681343));
#45305=CARTESIAN_POINT('Ctrl Pts',(6.91062659107492,-0.695543074258338,
3.90054607923755));
#45306=CARTESIAN_POINT('Ctrl Pts',(6.95834242713776,-0.292526745343327,
3.36117245204842));
#45307=CARTESIAN_POINT('Ctrl Pts',(7.00605826320061,0.379122722467859,3.40844412700009));
#45308=CARTESIAN_POINT('Ctrl Pts',(7.05377409926343,0.702617257610868,3.99895059076549));
#45309=CARTESIAN_POINT('Ctrl Pts',(7.10148993532628,0.380887926283931,4.59042078110798));
#45310=CARTESIAN_POINT('Ctrl Pts',(7.14920577138911,-0.290616845661789,
4.63969846327979));
#45311=CARTESIAN_POINT('Ctrl Pts',(7.19692160745196,-0.695243592084394,
4.10153121423426));
#45312=CARTESIAN_POINT('Ctrl Pts',(7.24463744351478,-0.461417505508394,
3.47012628326466));
#45313=CARTESIAN_POINT('Ctrl Pts',(7.29235327957764,0.196135405489393,3.32531254251214));
#45314=CARTESIAN_POINT('Ctrl Pts',(7.34006911564046,0.673574140181709,3.80007467379138));
#45315=CARTESIAN_POINT('Ctrl Pts',(7.38778495170331,0.532459385890787,4.45843130921146));
#45316=CARTESIAN_POINT('Ctrl Pts',(7.43550078776614,-0.0976210197556089,
4.69580341906706));
#45317=CARTESIAN_POINT('Ctrl Pts',(7.48321662382899,-0.638054538563543,
4.29420854311633));
#45318=CARTESIAN_POINT('Ctrl Pts',(7.53093245989182,-0.592552758097988,
3.62243743491725));
#45319=CARTESIAN_POINT('Ctrl Pts',(7.57864829595465,-0.00290066162856385,
3.29738783984629));
#45320=CARTESIAN_POINT('Ctrl Pts',(7.6263641320175,0.589415156704478,3.61755780248734));
#45321=CARTESIAN_POINT('Ctrl Pts',(7.67407996808033,0.64046196749915,4.28893031975233));
#45322=CARTESIAN_POINT('Ctrl Pts',(7.72179580414318,0.103362698669259,4.69497367861456));
#45323=CARTESIAN_POINT('Ctrl Pts',(7.769511640206,-0.528656126737314,4.46281201486565));
#45324=CARTESIAN_POINT('Ctrl Pts',(7.81722747626886,-0.675201896567852,
3.80564295658466));
#45325=CARTESIAN_POINT('Ctrl Pts',(7.86494331233168,-0.201699375449268,
3.32695496184095));
#45326=CARTESIAN_POINT('Ctrl Pts',(7.91265914839452,0.457026785680635,3.46633458176699));
#45327=CARTESIAN_POINT('Ctrl Pts',(7.96037498445737,0.696058217263005,4.09578736675475));
#45328=CARTESIAN_POINT('Ctrl Pts',(8.0080908205202,0.295888677698302,4.63727713897333));
#45329=CARTESIAN_POINT('Ctrl Pts',(8.05580665658303,-0.375999987428149,
4.59354550870361));
#45330=CARTESIAN_POINT('Ctrl Pts',(8.10352249264589,-0.702602078596463,
4.00475190491975));
#45331=CARTESIAN_POINT('Ctrl Pts',(8.1512383287087,-0.383993870066737,3.41159455373064));
#45332=CARTESIAN_POINT('Ctrl Pts',(8.19895416477156,0.287241817850264,3.35877897763223));
#45333=CARTESIAN_POINT('Ctrl Pts',(8.24667000083438,0.694698924651979,3.89480653282778));
#45334=CARTESIAN_POINT('Ctrl Pts',(8.29438583689724,0.464203319628796,4.52743486753713));
#45335=CARTESIAN_POINT('Ctrl Pts',(8.34210167296006,-0.192577336495663,
4.67571164775853));
#45336=CARTESIAN_POINT('Ctrl Pts',(8.3898175090229,-0.672511261332963,4.20347202468314));
#45337=CARTESIAN_POINT('Ctrl Pts',(8.43753334508575,-0.534867746972347,
3.54438091052171));
#45338=CARTESIAN_POINT('Ctrl Pts',(8.48524918114857,0.0939530494311211,
3.303691816829));
#45339=CARTESIAN_POINT('Ctrl Pts',(8.53296501721143,0.636495314888509,3.70243324182078));
#45340=CARTESIAN_POINT('Ctrl Pts',(8.58068085327425,0.594534138944492,4.37443479950165));
#45341=CARTESIAN_POINT('Ctrl Pts',(8.6283966893371,0.00660311512414562,
4.7025871193802));
#45342=CARTESIAN_POINT('Ctrl Pts',(8.67611252539993,-0.58739165091669,4.3855428768395));
#45343=CARTESIAN_POINT('Ctrl Pts',(8.72382836146277,-0.64197562573843,3.71444867815739));
#45344=CARTESIAN_POINT('Ctrl Pts',(8.77154419752561,-0.107023505379864,
3.30558065209521));
#45345=CARTESIAN_POINT('Ctrl Pts',(8.81926003358845,0.526209946737336,3.53440859822909));
#45346=CARTESIAN_POINT('Ctrl Pts',(8.86697586965128,0.676216707984864,4.19079629265377));
#45347=CARTESIAN_POINT('Ctrl Pts',(8.91469170571413,0.20524326135842,4.67197281575615));
#45348=CARTESIAN_POINT('Ctrl Pts',(8.96240754177695,-0.45420823024697,4.53606636251889));
#45349=CARTESIAN_POINT('Ctrl Pts',(9.0101233778398,-0.69655331512461,3.90788192013928));
#45350=CARTESIAN_POINT('Ctrl Pts',(9.05783921390263,-0.299242772872918,
3.36429092791464));
#45351=CARTESIAN_POINT('Ctrl Pts',(9.10555504996548,0.37286701214988,3.40448135822736));
#45352=CARTESIAN_POINT('Ctrl Pts',(9.15327088602831,0.702567282619003,3.99154572051203));
#45353=CARTESIAN_POINT('Ctrl Pts',(9.20098672209116,0.387089207071907,4.58637377773631));
#45354=CARTESIAN_POINT('Ctrl Pts',(9.24870255815397,-0.28385884346236,4.64272577234503));
#45355=CARTESIAN_POINT('Ctrl Pts',(9.29641839421684,-0.694134950315416,
4.10885280060212));
#45356=CARTESIAN_POINT('Ctrl Pts',(9.34413423027966,-0.46697625165475,3.47501862715065));
#45357=CARTESIAN_POINT('Ctrl Pts',(9.39185006634251,0.189013924253689,3.32328292626348));
#45358=CARTESIAN_POINT('Ctrl Pts',(9.43956590240535,0.671429705166911,3.79298692681914));
#45359=CARTESIAN_POINT('Ctrl Pts',(9.48728173846818,0.537261256551386,4.45279421778236));
#45360=CARTESIAN_POINT('Ctrl Pts',(9.53499757453101,-0.090282470782305,
4.69679361142145));
#45361=CARTESIAN_POINT('Ctrl Pts',(9.58271341059386,-0.634918416022234,
4.30091671014441));
#45362=CARTESIAN_POINT('Ctrl Pts',(9.63042924665669,-0.596499010353368,
3.62870336374299));
#45363=CARTESIAN_POINT('Ctrl Pts',(9.67814508271953,-0.0103053851599677,
3.29745743154951));
#45364=CARTESIAN_POINT('Ctrl Pts',(9.72586091878236,0.585351833794561,3.61136714997101));
#45365=CARTESIAN_POINT('Ctrl Pts',(9.77357675484522,0.643471456979869,4.28216439445919));
#45366=CARTESIAN_POINT('Ctrl Pts',(9.82129259090803,0.110681340139534,4.69384573385819));
#45367=CARTESIAN_POINT('Ctrl Pts',(9.8690084269709,-0.523749154402255,4.46835785966634));
#45368=CARTESIAN_POINT('Ctrl Pts',(9.91672426303372,-0.677212741539845,
3.81276975633088));
#45369=CARTESIAN_POINT('Ctrl Pts',(9.96444009909655,-0.208781447863971,
3.32911806666439));
#45370=CARTESIAN_POINT('Ctrl Pts',(10.0121559351594,0.451377061900895,3.4615475792254));
#45371=CARTESIAN_POINT('Ctrl Pts',(10.0598717712222,0.697029070393332,4.08844623493918));
#45372=CARTESIAN_POINT('Ctrl Pts',(10.1075876072851,0.302588558372737,4.63412335218805));
#45373=CARTESIAN_POINT('Ctrl Pts',(10.1553034433479,-0.369723682724971,
4.5974752378807));
#45374=CARTESIAN_POINT('Ctrl Pts',(10.2030192794108,-0.702512977046242,
4.01215641928927));
#45375=CARTESIAN_POINT('Ctrl Pts',(10.2507351154736,-0.390173794994359,
3.41567417381395));
#45376=CARTESIAN_POINT('Ctrl Pts',(10.2984509515364,0.280467986596366,3.3557873255338));
#45377=CARTESIAN_POINT('Ctrl Pts',(10.3461667875993,0.693551700540965,3.8874908887021));
#45378=CARTESIAN_POINT('Ctrl Pts',(10.3938826236621,0.469736216214169,4.52251329995044));
#45379=CARTESIAN_POINT('Ctrl Pts',(10.441598459725,-0.185445263282835,4.67770370795377));
#45380=CARTESIAN_POINT('Ctrl Pts',(10.4893142957878,-0.670329504065059,
4.21054837313121));
#45381=CARTESIAN_POINT('Ctrl Pts',(10.5370301318506,-0.539639846919137,
3.55004322755915));
#45382=CARTESIAN_POINT('Ctrl Pts',(10.5847459679134,0.0866093850789692,
3.30274030959437));
#45383=CARTESIAN_POINT('Ctrl Pts',(10.6324618039763,0.633323886102378,3.69574169404847));
#45384=CARTESIAN_POINT('Ctrl Pts',(10.6801776400391,0.598447317577389,4.36814816247366));
#45385=CARTESIAN_POINT('Ctrl Pts',(10.727893476102,0.0140073690254923,4.70247850861168));
#45386=CARTESIAN_POINT('Ctrl Pts',(10.7756093121648,-0.583295762033595,
4.39171203127037));
#45387=CARTESIAN_POINT('Ctrl Pts',(10.8233251482277,-0.644949419658282,
3.72123036834915));
#45388=CARTESIAN_POINT('Ctrl Pts',(10.8710409842905,-0.114336101388361,
3.30674714759503));
#45389=CARTESIAN_POINT('Ctrl Pts',(10.9187568203533,0.521273818073547,3.52888868827067));
#45390=CARTESIAN_POINT('Ctrl Pts',(10.9664726564162,0.678189969569843,4.18365899548663));
#45391=CARTESIAN_POINT('Ctrl Pts',(11.014188492479,0.212313836716152,4.66977242119035));
#45392=CARTESIAN_POINT('Ctrl Pts',(11.0619043285418,-0.44853335926228,4.54082352674158));
#45393=CARTESIAN_POINT('Ctrl Pts',(11.1096201646047,-0.697485469857315,
3.91522806604643));
#45394=CARTESIAN_POINT('Ctrl Pts',(11.1573360006675,-0.305925941288932,
3.36747997668469));
#45395=CARTESIAN_POINT('Ctrl Pts',(11.2050518367303,0.36657008644075,3.40058475730499));
#45396=CARTESIAN_POINT('Ctrl Pts',(11.2527676727932,0.702439163386103,3.98414177848112));
#45397=CARTESIAN_POINT('Ctrl Pts',(11.300483508856,0.393247548178179,4.58226164848818));
#45398=CARTESIAN_POINT('Ctrl Pts',(11.3481993449189,-0.277069341413063,
4.64568168744144));
#45399=CARTESIAN_POINT('Ctrl Pts',(11.3959151809817,-0.692949191524882,
4.11616229772746));
#45400=CARTESIAN_POINT('Ctrl Pts',(11.4436310170446,-0.47248313666557,3.47996928262364));
#45401=CARTESIAN_POINT('Ctrl Pts',(11.4913468531074,0.181871452681271,3.32132847698764));
#45402=CARTESIAN_POINT('Ctrl Pts',(11.5390626891702,0.669210688578896,3.78592217363756));
#45403=CARTESIAN_POINT('Ctrl Pts',(11.586778525233,0.54200345202451,4.44710683224685));
#45404=CARTESIAN_POINT('Ctrl Pts',(11.6344943612959,-0.082933894319074,
4.69770640718098));
#45405=CARTESIAN_POINT('Ctrl Pts',(11.6822101973587,-0.631711769407458,
4.30759145280778));
#45406=CARTESIAN_POINT('Ctrl Pts',(11.7299260334216,-0.600379006513997,
3.63501053441836));
#45407=CARTESIAN_POINT('Ctrl Pts',(11.7776418694844,-0.0177089639202829,
3.29760505835735));
#45408=CARTESIAN_POINT('Ctrl Pts',(11.8253577055473,0.581223492728864,3.60521966494218));
#45409=CARTESIAN_POINT('Ctrl Pts',(11.8730735416101,0.646409472732109,4.27536712768685));
#45410=CARTESIAN_POINT('Ctrl Pts',(11.9207893776729,0.11798768763725,4.69264072000881));
#45411=CARTESIAN_POINT('Ctrl Pts',(11.9685052137358,-0.518784006488825,
4.4738516814993));
#45412=CARTESIAN_POINT('Ctrl Pts',(12.0162210497986,-0.679148364938221,
3.81991735272367));
#45413=CARTESIAN_POINT('Ctrl Pts',(12.0639368858614,-0.215840329824027,
3.33135568986959));
#45414=CARTESIAN_POINT('Ctrl Pts',(12.1116527219243,0.445677201297934,3.45682038542343));
#45415=CARTESIAN_POINT('Ctrl Pts',(12.1593685579871,0.697922500842799,4.08109527893561));
#45416=CARTESIAN_POINT('Ctrl Pts',(12.2070843940499,0.309254828945687,4.63089912998995));
#45417=CARTESIAN_POINT('Ctrl Pts',(12.2548002301128,-0.36340631086944,4.60133860234362));
#45418=CARTESIAN_POINT('Ctrl Pts',(12.3025160661756,-0.702345843688318,
4.0195595833814));
#45419=CARTESIAN_POINT('Ctrl Pts',(12.3502319022385,-0.396310381268302,
3.41981869803717));
#45420=CARTESIAN_POINT('Ctrl Pts',(12.3979477383013,0.273663002289436,3.35286722952223));
#45421=CARTESIAN_POINT('Ctrl Pts',(12.4456635743641,0.69232743999824,3.88018774155459));
#45422=CARTESIAN_POINT('Ctrl Pts',(12.493379410427,0.475216936729713,4.51753369406595));
#45423=CARTESIAN_POINT('Ctrl Pts',(12.5410952464898,-0.178292591690169,
4.67962049203707));
#45424=CARTESIAN_POINT('Ctrl Pts',(12.5888110825527,-0.66807328977682,4.21760133486514));
#45425=CARTESIAN_POINT('Ctrl Pts',(12.6365269186155,-0.544352006232531,
3.55575552365962));
#45426=CARTESIAN_POINT('Ctrl Pts',(12.6842427546784,0.0792561005673328,
3.3018662506574));
#45427=CARTESIAN_POINT('Ctrl Pts',(12.7319585907411,0.630082110704352,3.68908394184497));
#45428=CARTESIAN_POINT('Ctrl Pts',(12.779674426804,0.60229402352211,4.36182063329482));
#45429=CARTESIAN_POINT('Ctrl Pts',(12.8273902628668,0.0214100670547408,
4.70229186986395));
#45430=CARTESIAN_POINT('Ctrl Pts',(12.8751060989297,-0.579135083425219,
4.39783767618763));
#45431=CARTESIAN_POINT('Ctrl Pts',(12.9228219349925,-0.647851575657132,
3.7280430229487));
#45432=CARTESIAN_POINT('Ctrl Pts',(12.9705377710554,-0.121635997485283,
3.30799064633195));
#45433=CARTESIAN_POINT('Ctrl Pts',(13.0182536071182,0.516279788787698,3.52342110712114));
#45434=CARTESIAN_POINT('Ctrl Pts',(13.065969443181,0.68008790103128,4.17650129834983));
#45435=CARTESIAN_POINT('Ctrl Pts',(13.1136852792439,0.219360829260397,4.66749763148232));
#45436=CARTESIAN_POINT('Ctrl Pts',(13.1614011153067,-0.44280866732052,4.54552061885334));
#45437=CARTESIAN_POINT('Ctrl Pts',(13.2091169513696,-0.698340151213866,
3.92258362801769));
#45438=CARTESIAN_POINT('Ctrl Pts',(13.2568327874324,-0.31257512890311,3.37073928277739));
#45439=CARTESIAN_POINT('Ctrl Pts',(13.3045486234952,0.36023244386594,3.39675473658331));
#45440=CARTESIAN_POINT('Ctrl Pts',(13.3522644595581,0.702233020544282,3.97673959790624));
#45441=CARTESIAN_POINT('Ctrl Pts',(13.3999802956209,0.39936220921291,4.57808484437918));
#45442=CARTESIAN_POINT('Ctrl Pts',(13.4476961316837,-0.270249063816132,
4.64856588328003));
#45443=CARTESIAN_POINT('Ctrl Pts',(13.4954119677466,-0.691686463226468,
4.123458892096));
#45444=CARTESIAN_POINT('Ctrl Pts',(13.5431278038094,-0.47793754049168,3.48497770064095));
#45445=CARTESIAN_POINT('Ctrl Pts',(13.5908436398723,0.174708779690948,3.31944941132403));
#45446=CARTESIAN_POINT('Ctrl Pts',(13.6385594759351,0.666917339243262,3.77888119920505));
#45447=CARTESIAN_POINT('Ctrl Pts',(13.6862753119979,0.54668544432619,4.44136978420615));
#45448=CARTESIAN_POINT('Ctrl Pts',(13.7339911480608,-0.075576105952426,
4.69854170502367));
#45449=CARTESIAN_POINT('Ctrl Pts',(13.7817069841236,-0.62843495524706,4.31423202967224));
#45450=CARTESIAN_POINT('Ctrl Pts',(13.8294228201864,-0.604192315423611,
3.64135824639153));
#45451=CARTESIAN_POINT('Ctrl Pts',(13.8771386562493,-0.025110575652917,
3.29783070386218));
#45452=CARTESIAN_POINT('Ctrl Pts',(13.9248544923121,0.577030592115723,3.59911603023956));
#45453=CARTESIAN_POINT('Ctrl Pts',(13.972570328375,0.649275688387581,4.26853927444071));
#45454=CARTESIAN_POINT('Ctrl Pts',(14.0202861644378,0.125280929622514,4.69135877091509));
#45455=CARTESIAN_POINT('Ctrl Pts',(14.0680020005006,-0.513761234509794,
4.47929287013608));
#45456=CARTESIAN_POINT('Ctrl Pts',(14.1157178365635,-0.681008551759042,
3.82708495184235));
#45457=CARTESIAN_POINT('Ctrl Pts',(14.1634336726263,-0.222875237264486,
3.33366758291179));
#45458=CARTESIAN_POINT('Ctrl Pts',(14.2111495086891,0.439927836986373,3.45215352543546));
#45459=CARTESIAN_POINT('Ctrl Pts',(14.258865344752,0.698738409372782,4.07373531525328));
#45460=CARTESIAN_POINT('Ctrl Pts',(14.3065811808148,0.315886748959774,4.62760483051036));
#45461=CARTESIAN_POINT('Ctrl Pts',(14.3542970168777,-0.357048573565392,
4.60513517296818));
#45462=CARTESIAN_POINT('Ctrl Pts',(14.4020128529405,-0.702100697086982,
4.02696057488784));
#45463=CARTESIAN_POINT('Ctrl Pts',(14.4497286890033,-0.402402947265751,
3.42402766604624));
#45464=CARTESIAN_POINT('Ctrl Pts',(14.4974445250662,0.266827620794843,3.35001901394789));
#45465=CARTESIAN_POINT('Ctrl Pts',(14.545160361129,0.691026279008849,3.87289790258421));
#45466=CARTESIAN_POINT('Ctrl Pts',(14.5928761971919,0.480644872403009,4.51249660299459));
#45467=CARTESIAN_POINT('Ctrl Pts',(14.6405920332547,-0.171120116202498,
4.6814617871012));
#45468=CARTESIAN_POINT('Ctrl Pts',(14.6883078693176,-0.665742869077823,
4.22463012647536));
#45469=CARTESIAN_POINT('Ctrl Pts',(14.7360237053803,-0.549003701508229,
3.56151716432844));
#45470=CARTESIAN_POINT('Ctrl Pts',(14.7837395414432,0.0718940126641393,
3.30106973710437));
#45471=CARTESIAN_POINT('Ctrl Pts',(14.831455377506,0.626770348775451,3.68246072472179));
#45472=CARTESIAN_POINT('Ctrl Pts',(14.8791712135689,0.606073829504824,4.35545291479698));
#45473=CARTESIAN_POINT('Ctrl Pts',(14.9268870496317,0.0288103869553486,
4.70202722386799));
#45474=CARTESIAN_POINT('Ctrl Pts',(14.9746028856946,-0.574910077240004,
4.4039191311837));
#45475=CARTESIAN_POINT('Ctrl Pts',(15.0223187217574,-0.650681771377263,
3.73488588523872));
#45476=CARTESIAN_POINT('Ctrl Pts',(15.0700345578202,-0.128922382832804,
3.30931101018402));
#45477=CARTESIAN_POINT('Ctrl Pts',(15.1177503938831,0.511228413592865,3.51800646209349));
#45478=CARTESIAN_POINT('Ctrl Pts',(15.1654662299459,0.681910291555949,4.16932399628639));
#45479=CARTESIAN_POINT('Ctrl Pts',(15.2131820660088,0.226383456244684,4.6651486993049));
#45480=CARTESIAN_POINT('Ctrl Pts',(15.2608979020716,-0.437034790293287,
4.55015711712348));
#45481=CARTESIAN_POINT('Ctrl Pts',(15.3086137381344,-0.699117264260319,
3.92994778903219));
#45482=CARTESIAN_POINT('Ctrl Pts',(15.3563295741972,-0.319189597155267,
3.37406848416447));
#45483=CARTESIAN_POINT('Ctrl Pts',(15.4040454102601,0.353854788380711,3.39299172148285));
#45484=CARTESIAN_POINT('Ctrl Pts',(15.4517612463229,0.70194887699091,3.96934000098645));
#45485=CARTESIAN_POINT('Ctrl Pts',(15.4994770823858,0.40543251098856,4.57384382934891));
#45486=CARTESIAN_POINT('Ctrl Pts',(15.5471929184486,-0.263398768235635,
4.65137803949801));
#45487=CARTESIAN_POINT('Ctrl Pts',(15.5949087545115,-0.690346905678043,
4.13074177323664));
#45488=CARTESIAN_POINT('Ctrl Pts',(15.6426245905743,-0.483338857283784,
3.4900433248913));
#45489=CARTESIAN_POINT('Ctrl Pts',(15.6903404266371,0.167526700878456,3.31764593799033));
#45490=CARTESIAN_POINT('Ctrl Pts',(15.7380562627,0.664549911894371,3.77186478559966));
#45491=CARTESIAN_POINT('Ctrl Pts',(15.7857720987628,0.551306713402943,4.43558371090429));
#45492=CARTESIAN_POINT('Ctrl Pts',(15.8334879348256,-0.0682099229505586,
4.69929941216862));
#45493=CARTESIAN_POINT('Ctrl Pts',(15.8812037708885,-0.625088337514006,
4.32083770313399));
#45494=CARTESIAN_POINT('Ctrl Pts',(15.9289196069513,-0.607938513517956,
3.64774579458877));
#45495=CARTESIAN_POINT('Ctrl Pts',(15.9766354430142,-0.0325093982219456,
3.29813434300035));
#45496=CARTESIAN_POINT('Ctrl Pts',(16.024351279077,0.572773597682653,3.59305692382598));
#45497=CARTESIAN_POINT('Ctrl Pts',(16.0720671151399,0.652069785580651,4.2616815931263));
#45498=CARTESIAN_POINT('Ctrl Pts',(16.1197829512026,0.132560255996602,4.69000002896988));
#45499=CARTESIAN_POINT('Ctrl Pts',(16.1674987872655,-0.508681396370837,
4.48468082119526));
#45500=CARTESIAN_POINT('Ctrl Pts',(16.2152146233283,-0.682793095381579,
3.83427175754402));
#45501=CARTESIAN_POINT('Ctrl Pts',(16.2629304593912,-0.229885388781225,
3.33605348899688));
#45502=CARTESIAN_POINT('Ctrl Pts',(16.310646295454,0.434129607578297,3.44754751763412));
#45503=CARTESIAN_POINT('Ctrl Pts',(16.3583621315168,0.699476705356048,4.06636716140204));
#45504=CARTESIAN_POINT('Ctrl Pts',(16.4060779675797,0.322483581772784,4.62424081966442));
#45505=CARTESIAN_POINT('Ctrl Pts',(16.4537938036425,-0.350651177000141,
4.60886452804932));
#45506=CARTESIAN_POINT('Ctrl Pts',(16.5015096397054,-0.701777564471952,
4.03435857174156));
#45507=CARTESIAN_POINT('Ctrl Pts',(16.5492254757682,-0.408450816253369,
3.42830061032894));
#45508=CARTESIAN_POINT('Ctrl Pts',(16.596941311831,0.259962601354342,3.34724299517707));
#45509=CARTESIAN_POINT('Ctrl Pts',(16.6446571478939,0.689648362099571,3.86562218151166));
#45510=CARTESIAN_POINT('Ctrl Pts',(16.6923729839567,0.486019420324727,4.50740258623259));
#45511=CARTESIAN_POINT('Ctrl Pts',(16.7400888200196,-0.163928633504336,
4.6832273886238));
#45512=CARTESIAN_POINT('Ctrl Pts',(16.7878046560824,-0.663338500820136,
4.23163396723712));
#45513=CARTESIAN_POINT('Ctrl Pts',(16.8355204921452,-0.553594416058007,
3.56732750958986));
#45514=CARTESIAN_POINT('Ctrl Pts',(16.8832363282081,0.064523939115192,3.30035085740826));
#45515=CARTESIAN_POINT('Ctrl Pts',(16.9309521642709,0.623388968170475,3.67587277835446));
#45516=CARTESIAN_POINT('Ctrl Pts',(16.9786680003338,0.609786315682611,4.34904571427615));
#45517=CARTESIAN_POINT('Ctrl Pts',(17.0263838363966,0.0362075067348799,
4.70168460001938));
#45518=CARTESIAN_POINT('Ctrl Pts',(17.0740996724594,-0.570621212771584,
4.40995572075944));
#45519=CARTESIAN_POINT('Ctrl Pts',(17.1218155085223,-0.653439692453966,
3.74175819514654));
#45520=CARTESIAN_POINT('Ctrl Pts',(17.1695313445851,-0.136194448093839,
3.31070809249149));
#45521=CARTESIAN_POINT('Ctrl Pts',(17.2172471806479,0.50612025357182,3.51264535462077));
#45522=CARTESIAN_POINT('Ctrl Pts',(17.2649630167108,0.683656938721366,4.16212788651693));
#45523=CARTESIAN_POINT('Ctrl Pts',(17.3126788527736,0.233380937628925,4.66272588556639));
#45524=CARTESIAN_POINT('Ctrl Pts',(17.3603946888365,-0.431212369515449,
4.55473250655174));
#45525=CARTESIAN_POINT('Ctrl Pts',(17.4081105248993,-0.699816722678643,
3.93731973111387));
#45526=CARTESIAN_POINT('Ctrl Pts',(17.4558263609621,-0.325768611341644,
3.37746721105403));
#45527=CARTESIAN_POINT('Ctrl Pts',(17.503542197025,0.347437828384778,3.38929612998149));
#45528=CARTESIAN_POINT('Ctrl Pts',(17.5512580330878,0.701586764287296,3.96194380963385));
#45529=CARTESIAN_POINT('Ctrl Pts',(17.5989738691507,0.411457779244836,4.56953907446917));
#45530=CARTESIAN_POINT('Ctrl Pts',(17.6466897052135,-0.256519215569882,
4.65411784373439));
#45531=CARTESIAN_POINT('Ctrl Pts',(17.6944055412764,-0.688930667671302,
4.13801013220155));
#45532=CARTESIAN_POINT('Ctrl Pts',(17.7421213773391,-0.488686487089258,
3.49516559270919));
#45533=CARTESIAN_POINT('Ctrl Pts',(17.789837213402,0.160326013994967,3.3159182573078));
#45534=CARTESIAN_POINT('Ctrl Pts',(17.8375530494648,0.662108669494809,3.76487371217125));
#45535=CARTESIAN_POINT('Ctrl Pts',(17.8852688855277,0.555866745946156,4.42974925503083));
#45536=CARTESIAN_POINT('Ctrl Pts',(17.9329847215905,-0.060836163514142,
4.69997944445332));
#45537=CARTESIAN_POINT('Ctrl Pts',(17.9807005576534,-0.621672287934692,
4.32740773946617));
#45538=CARTESIAN_POINT('Ctrl Pts',(18.0284163937162,-0.611617184687133,
3.65417246951162));
#45539=CARTESIAN_POINT('Ctrl Pts',(18.0761322297791,-0.0399046098013318,
3.29851594204507));
#45540=CARTESIAN_POINT('Ctrl Pts',(18.1238480658419,0.568452982276385,3.58704301871817));
#45541=CARTESIAN_POINT('Ctrl Pts',(18.1715639019047,0.65479145395626,4.25479484546229));
#45542=CARTESIAN_POINT('Ctrl Pts',(18.2192797379675,0.139824858206545,4.68856464509573));
#45543=CARTESIAN_POINT('Ctrl Pts',(18.2669955740304,-0.503545056316242,
4.49001493620888));
#45544=CARTESIAN_POINT('Ctrl Pts',(18.3147114100932,-0.684501797587214,
3.84147697155243));
#45545=CARTESIAN_POINT('Ctrl Pts',(18.3624272461561,-0.236870005719869,
3.33851314310973));
#45546=CARTESIAN_POINT('Ctrl Pts',(18.4101430822189,0.42828315711354,3.44300287363294));
#45547=CARTESIAN_POINT('Ctrl Pts',(18.4578589182817,0.70013730678616,4.05899163580144));
#45548=CARTESIAN_POINT('Ctrl Pts',(18.5055747543446,0.32904459463985,4.62080747111051));
#45549=CARTESIAN_POINT('Ctrl Pts',(18.5532905904074,-0.34421483176614,4.61252625334797));
#45550=CARTESIAN_POINT('Ctrl Pts',(18.6010064264702,-0.701376481735239,
4.0417527522082));
#45551=CARTESIAN_POINT('Ctrl Pts',(18.6487222625331,-0.414453316462639,
3.43263705626685));
#45552=CARTESIAN_POINT('Ctrl Pts',(18.6964380985959,0.253068706501803,3.34453948155689));
#45553=CARTESIAN_POINT('Ctrl Pts',(18.7441539346588,0.68819384232267,3.85836138648927));
#45554=CARTESIAN_POINT('Ctrl Pts',(18.7918697707216,0.491339983515996,4.50225220959958));
#45555=CARTESIAN_POINT('Ctrl Pts',(18.8395856067844,-0.156718942392259,
4.68491710048942));
#45556=CARTESIAN_POINT('Ctrl Pts',(18.8873014428473,-0.660860452068119,
4.23861207919858));
#45557=CARTESIAN_POINT('Ctrl Pts',(18.9350172789101,-0.558123639969822,
3.57318591405529));
#45558=CARTESIAN_POINT('Ctrl Pts',(18.9827331149729,0.0571466985584877,
3.29970969142451));
#45559=CARTESIAN_POINT('Ctrl Pts',(19.0304489510358,0.619938344467307,3.66932083449001));
#45560=CARTESIAN_POINT('Ctrl Pts',(19.0781647870986,0.613431069708698,4.3425997434341));
#45561=CARTESIAN_POINT('Ctrl Pts',(19.1258806231615,0.0436006047213211,
4.70126403633668));
#45562=CARTESIAN_POINT('Ctrl Pts',(19.1735964592243,-0.566268966340429,
4.41594677447179));
#45563=CARTESIAN_POINT('Ctrl Pts',(19.2213122952871,-0.656125032675529,
3.74865918919138));
#45564=CARTESIAN_POINT('Ctrl Pts',(19.26902813135,-0.143451385285705,3.31218173833215));
#45565=CARTESIAN_POINT('Ctrl Pts',(19.3167439674128,0.500955875668841,3.50733837970023));
#45566=CARTESIAN_POINT('Ctrl Pts',(19.3644598034757,0.68532764936022,4.15491376927485));
#45567=CARTESIAN_POINT('Ctrl Pts',(19.4121756395385,0.240352494576274,4.66022945763735));
#45568=CARTESIAN_POINT('Ctrl Pts',(19.4598914756013,-0.425342048711971,
4.55924628221868));
#45569=CARTESIAN_POINT('Ctrl Pts',(19.5076073116642,-0.700438454444525,
3.94469862920436));
#45570=CARTESIAN_POINT('Ctrl Pts',(19.555323147727,-0.332311429993836,3.3809350976725));
#45571=CARTESIAN_POINT('Ctrl Pts',(19.6030389837899,0.340982256434611,3.38566835039883));
#45572=CARTESIAN_POINT('Ctrl Pts',(19.6507548198527,0.701146760813864,3.95455188724214));
#45573=CARTESIAN_POINT('Ctrl Pts',(19.6984706559155,0.417437272672218,4.56517097885182));
#45574=CARTESIAN_POINT('Ctrl Pts',(19.7461864919784,-0.249611033919464,
4.6567851409082));
#45575=CARTESIAN_POINT('Ctrl Pts',(19.7939023280412,-0.687438163400574,
4.14526287985386));
#45576=CARTESIAN_POINT('Ctrl Pts',(19.841618164104,-0.493979350866992,3.5003444672369));
#45577=CARTESIAN_POINT('Ctrl Pts',(19.8893340001669,0.153106602982307,3.31426555646693));
#45578=CARTESIAN_POINT('Ctrl Pts',(19.9370498362297,0.659595612567133,3.75791065255607));
#45579=CARTESIAN_POINT('Ctrl Pts',(19.9847656722925,0.560361770063263,4.42386348253578));
#45580=CARTESIAN_POINT('Ctrl Pts',(20.0324815083554,-0.0534494809679074,
4.70058849011268));
#45581=CARTESIAN_POINT('Ctrl Pts',(20.0801973444182,-0.618198828117398,
4.33392863744107));
#45582=CARTESIAN_POINT('Ctrl Pts',(20.1279131804811,-0.615205937201001,
3.66066167313574));
#45583=CARTESIAN_POINT('Ctrl Pts',(20.1756290165439,-0.0473369003220797,
3.29892991724937));
#45584=CARTESIAN_POINT('Ctrl Pts',(20.2233448526068,0.564147630203746,3.58116102158214));
#45585=CARTESIAN_POINT('Ctrl Pts',(20.2710606886696,0.657292163719816,4.24771695100806));
#45586=CARTESIAN_POINT('Ctrl Pts',(20.3187765247324,0.147355317357748,4.68736342730055));
#45587=CARTESIAN_POINT('Ctrl Pts',(20.3664923607953,-0.498896366832293,
4.49468216892218));
#45588=CARTESIAN_POINT('Ctrl Pts',(20.4062555575143,-0.653992183610565,
3.9575054511282));
#45589=CARTESIAN_POINT('Ctrl Pts',(20.4380661148895,-0.465699721472375,
3.59327933193152));
#45590=CARTESIAN_POINT('Ctrl Pts',(20.461924032921,-0.215665100260693,3.41899970433759));
#45591=CARTESIAN_POINT('Ctrl Pts',(20.4857819509523,0.0900520562992202,
3.38718375849312));
#45592=CARTESIAN_POINT('Ctrl Pts',(20.5096398689838,0.372154449079436,3.50499792242313));
#45593=CARTESIAN_POINT('Ctrl Pts',(20.5334977870152,0.564103623124681,3.74397162737493));
#45594=CARTESIAN_POINT('Ctrl Pts',(20.5573557050466,0.61766411855396,4.04548854604559));
#45595=CARTESIAN_POINT('Ctrl Pts',(20.581213623078,0.520427284318709,4.33591550271974));
#45596=CARTESIAN_POINT('Ctrl Pts',(20.6050715411094,0.295805552416038,4.5441843692251));
#45597=CARTESIAN_POINT('Ctrl Pts',(20.6289294591409,-0.00108183093298003,
4.61939465531364));
#45598=CARTESIAN_POINT('Ctrl Pts',(20.6527873771723,-0.297740088546312,
4.543141139652));
#45599=CARTESIAN_POINT('Ctrl Pts',(20.6766452952037,-0.521574030203058,
4.33407743490148));
#45600=CARTESIAN_POINT('Ctrl Pts',(20.7005032132351,-0.617878846294169,
4.04332131262121));
#45601=CARTESIAN_POINT('Ctrl Pts',(20.7243611312665,-0.563090193646282,
3.74197268265107));
#45602=CARTESIAN_POINT('Ctrl Pts',(20.748219049298,-0.370613436173077,3.50371837193987));
#45603=CARTESIAN_POINT('Ctrl Pts',(20.7720769673294,-0.0875101228827464,
3.38681864340431));
#45604=CARTESIAN_POINT('Ctrl Pts',(20.7959348853608,0.216991017820888,3.41985835035499));
#45605=CARTESIAN_POINT('Ctrl Pts',(20.8197928033922,0.468432357761717,3.59475855107288));
#45606=CARTESIAN_POINT('Ctrl Pts',(20.8436507214236,0.605329007232586,3.86875129405724));
#45607=CARTESIAN_POINT('Ctrl Pts',(20.8675086394551,0.594206341669864,4.17483793696784));
#45608=CARTESIAN_POINT('Ctrl Pts',(20.8913665574864,0.437783978244149,4.43817193323088));
#45609=CARTESIAN_POINT('Ctrl Pts',(20.9152244755179,0.174311539695801,4.5943609607934));
#45610=CARTESIAN_POINT('Ctrl Pts',(20.9390823935493,-0.13178483570001,4.60521254097096));
#45611=CARTESIAN_POINT('Ctrl Pts',(20.9629403115808,-0.405656219889506,
4.46807317049539));
#45612=CARTESIAN_POINT('Ctrl Pts',(20.9867982296121,-0.580333613298163,
4.21647715910241));
#45613=CARTESIAN_POINT('Ctrl Pts',(21.0106561476436,-0.613103627724174,
3.91194658594648));
#45614=CARTESIAN_POINT('Ctrl Pts',(21.034514065675,-0.495953105920446,3.62894747086441));
#45615=CARTESIAN_POINT('Ctrl Pts',(21.0583719837064,-0.257528539509485,
3.43668080652407));
#45616=CARTESIAN_POINT('Ctrl Pts',(21.0822299017379,0.0438687693677006,
3.38216102944232));
#45617=CARTESIAN_POINT('Ctrl Pts',(21.1060878197692,0.334538969374667,3.47871971028568));
#45618=CARTESIAN_POINT('Ctrl Pts',(21.1299457378007,0.543405278604256,3.7027456213393));
#45619=CARTESIAN_POINT('Ctrl Pts',(21.153803655832,0.619394195209021,3.99945832503004));
#45620=CARTESIAN_POINT('Ctrl Pts',(21.1776615738635,0.543924359096133,4.29630348300169));
#45621=CARTESIAN_POINT('Ctrl Pts',(21.2015194918949,0.33545020099803,4.52069436823682));
#45622=CARTESIAN_POINT('Ctrl Pts',(21.2253774099264,0.0449493312674926,
4.61776129700707));
#45623=CARTESIAN_POINT('Ctrl Pts',(21.2492353279577,-0.256542874348706,
4.56376876117982));
#45624=CARTESIAN_POINT('Ctrl Pts',(21.2730932459892,-0.495303359101402,
4.37191940649105));
#45625=CARTESIAN_POINT('Ctrl Pts',(21.2969511640206,-0.612948680759938,
4.08912562603418));
#45626=CARTESIAN_POINT('Ctrl Pts',(21.320809082052,-0.580711353586496,3.78453820227854));
#45627=CARTESIAN_POINT('Ctrl Pts',(21.3446670000834,-0.406474282201139,
3.53263705712739));
#45628=CARTESIAN_POINT('Ctrl Pts',(21.3685249181149,-0.132843176680646,
3.39501888221951));
#45629=CARTESIAN_POINT('Ctrl Pts',(21.3923828361463,0.17327170411384,3.40533506996376));
#45630=CARTESIAN_POINT('Ctrl Pts',(21.4162407541777,0.437016933425986,3.56106303144932));
#45631=CARTESIAN_POINT('Ctrl Pts',(21.4400986722091,0.593899618413251,3.82412303814848));
#45632=CARTESIAN_POINT('Ctrl Pts',(21.4639565902405,0.605557669197671,4.13018975281259));
#45633=CARTESIAN_POINT('Ctrl Pts',(21.4878145082719,0.469140374803543,4.40442152661638));
#45634=CARTESIAN_POINT('Ctrl Pts',(21.5116724263034,0.218005479642704,4.57976122094124));
#45635=CARTESIAN_POINT('Ctrl Pts',(21.5355303443348,-0.0864376936408111,
4.61333350436739));
#45636=CARTESIAN_POINT('Ctrl Pts',(21.5593882623662,-0.369744496313637,
4.49692903910649));
#45637=CARTESIAN_POINT('Ctrl Pts',(21.5832461803976,-0.562638697999917,
4.2590118877088));
#45638=CARTESIAN_POINT('Ctrl Pts',(21.607104098429,-0.617952412054802,3.95775927442416));
#45639=CARTESIAN_POINT('Ctrl Pts',(21.6309620164605,-0.522159928676552,
3.66683566915707));
#45640=CARTESIAN_POINT('Ctrl Pts',(21.6548199344919,-0.298685119385998,
3.45737981799522));
#45641=CARTESIAN_POINT('Ctrl Pts',(21.6786778525233,-0.00217366238626178,
3.38060938201055));
#45642=CARTESIAN_POINT('Ctrl Pts',(21.7025357705547,0.294869314276287,3.45529682398599));
#45643=CARTESIAN_POINT('Ctrl Pts',(21.7263936885862,0.519808711519421,3.66317902991346));
#45644=CARTESIAN_POINT('Ctrl Pts',(21.7502516066175,0.617640719491047,3.95342313784609));
#45645=CARTESIAN_POINT('Ctrl Pts',(21.774109524649,0.564442747351711,4.25505655730362));
#45646=CARTESIAN_POINT('Ctrl Pts',(21.7979674426804,0.373223148373148,4.49432170089927));
#45647=CARTESIAN_POINT('Ctrl Pts',(21.8218253607118,0.0907403232229101,
4.61271172357229));
#45648=CARTESIAN_POINT('Ctrl Pts',(21.8456832787432,-0.213930982672105,
4.58127703989962));
#45649=CARTESIAN_POINT('Ctrl Pts',(21.8695411967746,-0.466290335940828,
4.40770428630285));
#45650=CARTESIAN_POINT('Ctrl Pts',(21.8933991148061,-0.604629000578284,
4.13443672906324));
#45651=CARTESIAN_POINT('Ctrl Pts',(21.9172570328375,-0.595119404811066,
3.82829572958469));
#45652=CARTESIAN_POINT('Ctrl Pts',(21.9411149508689,-0.440086903840403,
3.56414110135311));
#45653=CARTESIAN_POINT('Ctrl Pts',(21.9649728689003,-0.177441167154219,
3.40656584639871));
#45654=CARTESIAN_POINT('Ctrl Pts',(21.9888307869318,0.128593768301574,3.39410140682164));
#45655=CARTESIAN_POINT('Ctrl Pts',(22.0126887049631,0.403184024583593,3.52979567762293));
#45656=CARTESIAN_POINT('Ctrl Pts',(22.0365466229946,0.579184804342829,3.7804677133541));
#45657=CARTESIAN_POINT('Ctrl Pts',(22.060404541026,0.613559122762511,4.08482137310942));
#45658=CARTESIAN_POINT('Ctrl Pts',(22.0842624590574,0.497901522652627,4.36843389665204));
#45659=CARTESIAN_POINT('Ctrl Pts',(22.1081203770888,0.260493437687466,4.56195429652472));
#45660=CARTESIAN_POINT('Ctrl Pts',(22.1319782951203,-0.0406123884881684,
4.61806156357065));
#45661=CARTESIAN_POINT('Ctrl Pts',(22.1558362131517,-0.33178737942464,4.52303594266224));
#45662=CARTESIAN_POINT('Ctrl Pts',(22.1796941311831,-0.541831318374727,
4.30011378656432));
#45663=CARTESIAN_POINT('Ctrl Pts',(22.2035520492145,-0.619382740812877,
4.00380563470766));
#45664=CARTESIAN_POINT('Ctrl Pts',(22.2274099672459,-0.545478211438426,
3.70656690151735));
#45665=CARTESIAN_POINT('Ctrl Pts',(22.2512678852774,-0.338189400908512,
3.48108055383335));
#45666=CARTESIAN_POINT('Ctrl Pts',(22.2751258033088,-0.0482040696311437,
3.38248414587532));
#45667=CARTESIAN_POINT('Ctrl Pts',(22.2989837213402,0.253568469476171,3.43488718493857));
#45668=CARTESIAN_POINT('Ctrl Pts',(22.3228416393716,0.493336611197201,3.62547570084914));
#45669=CARTESIAN_POINT('Ctrl Pts',(22.346699557403,0.612470512379129,3.90764560936005));
#45670=CARTESIAN_POINT('Ctrl Pts',(22.3705574754344,0.581838691587799,4.21239868278141));
#45671=CARTESIAN_POINT('Ctrl Pts',(22.3944153934659,0.408931458591185,4.46521449128699));
#45672=CARTESIAN_POINT('Ctrl Pts',(22.4182733114973,0.13602935083686,4.60427268703701));
#45673=CARTESIAN_POINT('Ctrl Pts',(22.4421312295287,-0.170135649772668,
4.59556974592947));
#45674=CARTESIAN_POINT('Ctrl Pts',(22.4659891475601,-0.434697828443077,
4.44123378804823));
#45675=CARTESIAN_POINT('Ctrl Pts',(22.4898470655916,-0.592964587096883,
4.17900413283907));
#45676=CARTESIAN_POINT('Ctrl Pts',(22.513704983623,-0.606235276705168,3.87300312362118));
#45677=CARTESIAN_POINT('Ctrl Pts',(22.5375629016543,-0.471265070143009,
3.59805624874041));
#45678=CARTESIAN_POINT('Ctrl Pts',(22.5614208196858,-0.22105744785653,3.4213956854475));
#45679=CARTESIAN_POINT('Ctrl Pts',(22.5852787377172,0.0832042338527798,
3.38621941950615));
#45680=CARTESIAN_POINT('Ctrl Pts',(22.6091366557487,0.36712117327337,3.50112963696785));
#45681=CARTESIAN_POINT('Ctrl Pts',(22.63299457378,0.561265174232679,3.7380264683998));
#45682=CARTESIAN_POINT('Ctrl Pts',(22.6568524918115,0.618167971965146,4.03898443479498));
#45683=CARTESIAN_POINT('Ctrl Pts',(22.6807104098429,0.523905402647805,4.33040686810369));
#45684=CARTESIAN_POINT('Ctrl Pts',(22.7045683278744,0.301545895245711,4.54104106792393));
#45685=CARTESIAN_POINT('Ctrl Pts',(22.7284262459057,0.00542710047790416,
4.61936606261506));
#45686=CARTESIAN_POINT('Ctrl Pts',(22.7522841639372,-0.291974666000346,
4.54625809930836));
#45687=CARTESIAN_POINT('Ctrl Pts',(22.7761420819686,-0.518067845615496,
4.33953802216683));
#45688=CARTESIAN_POINT('Ctrl Pts',(22.7920473606562,-0.584213376873476,
4.14642833911731));
#45689=CARTESIAN_POINT('Ctrl Pts',(22.8,-0.592174260192535,4.04779597854866));
#45690=CARTESIAN_POINT('Ctrl Pts',(3.96816317011931,-0.282716247115855,
3.54616445487434));
#45691=CARTESIAN_POINT('Ctrl Pts',(3.97611580946312,-0.207125539895404,
3.49907532469992));
#45692=CARTESIAN_POINT('Ctrl Pts',(3.99202108815073,-0.0320395462633344,
3.44344227840288));
#45693=CARTESIAN_POINT('Ctrl Pts',(4.01587900618214,0.238586678544665,3.49618207793602));
#45694=CARTESIAN_POINT('Ctrl Pts',(4.03973692421357,0.450798406251909,3.67207593825259));
#45695=CARTESIAN_POINT('Ctrl Pts',(4.06359484224498,0.552814952159096,3.92817792166325));
#45696=CARTESIAN_POINT('Ctrl Pts',(4.0874527602764,0.519633627921064,4.20183097195279));
#45697=CARTESIAN_POINT('Ctrl Pts',(4.11131067830782,0.359398059257131,4.42613686623617));
#45698=CARTESIAN_POINT('Ctrl Pts',(4.13516859633924,0.11127440638865,4.54623750576341));
#45699=CARTESIAN_POINT('Ctrl Pts',(4.15902651437066,-0.164055973910312,
4.53276988152218));
#45700=CARTESIAN_POINT('Ctrl Pts',(4.18288443240208,-0.399271733473279,
4.38902461621758));
#45701=CARTESIAN_POINT('Ctrl Pts',(4.2067423504335,-0.536853866020863,4.15015270818839));
#45702=CARTESIAN_POINT('Ctrl Pts',(4.23060026846491,-0.543161034884179,
3.87456412255522));
#45703=CARTESIAN_POINT('Ctrl Pts',(4.25445818649634,-0.416650307492554,
3.62964815836115));
#45704=CARTESIAN_POINT('Ctrl Pts',(4.27831610452775,-0.188257351244862,
3.47529323740438));
#45705=CARTESIAN_POINT('Ctrl Pts',(4.30217402255918,0.0861697193074588,
3.44924344981891));
#45706=CARTESIAN_POINT('Ctrl Pts',(4.32603194059059,0.339525912432458,3.55786862136322));
#45707=CARTESIAN_POINT('Ctrl Pts',(4.34988985862202,0.509858789389686,3.77460696883261));
#45708=CARTESIAN_POINT('Ctrl Pts',(4.37374777665342,0.555517294574929,4.0464600464808));
#45709=CARTESIAN_POINT('Ctrl Pts',(4.39760569468486,0.465336694276122,4.30695238014399));
#45710=CARTESIAN_POINT('Ctrl Pts',(4.42146361271626,0.261368594047533,4.4923864940975));
#45711=CARTESIAN_POINT('Ctrl Pts',(4.4453215307477,-0.00651124555331369,
4.55741869872598));
#45712=CARTESIAN_POINT('Ctrl Pts',(4.4691794487791,-0.272798909000308,4.48614684730087));
#45713=CARTESIAN_POINT('Ctrl Pts',(4.49303736681053,-0.472379807908186,
4.29599884956661));
#45714=CARTESIAN_POINT('Ctrl Pts',(4.51689528484195,-0.55645097662433,4.03347107014466));
#45715=CARTESIAN_POINT('Ctrl Pts',(4.54075320287336,-0.504454724024634,
3.76275870240323));
#45716=CARTESIAN_POINT('Ctrl Pts',(4.56461112090479,-0.329105550388866,
3.55005829421323));
#45717=CARTESIAN_POINT('Ctrl Pts',(4.5884690389362,-0.0732811049967102,
3.44738088927219));
#45718=CARTESIAN_POINT('Ctrl Pts',(4.61232695696762,0.200462566687888,3.47983390993684));
#45719=CARTESIAN_POINT('Ctrl Pts',(4.63618487499904,0.425187680335341,3.63948170866684));
#45720=CARTESIAN_POINT('Ctrl Pts',(4.66004279303046,0.54594282425631,3.88728604994618));
#45721=CARTESIAN_POINT('Ctrl Pts',(4.68390071106188,0.533200076465109,4.16265202228146));
#45722=CARTESIAN_POINT('Ctrl Pts',(4.7077586290933,0.390075385898422,4.39824514461603));
#45723=CARTESIAN_POINT('Ctrl Pts',(4.73161654712472,0.151566638040082,4.53645648111246));
#45724=CARTESIAN_POINT('Ctrl Pts',(4.75547446515614,-0.124004281411749,
4.54348959519552));
#45725=CARTESIAN_POINT('Ctrl Pts',(4.77933238318755,-0.369252776249408,
4.41762469889406));
#45726=CARTESIAN_POINT('Ctrl Pts',(4.80319030121898,-0.524208909050512,
4.18963918784455));
#45727=CARTESIAN_POINT('Ctrl Pts',(4.82704821925039,-0.550981684424725,
3.91528172969931));
#45728=CARTESIAN_POINT('Ctrl Pts',(4.85090613728181,-0.443024429517375,
3.66164019632193));
#45729=CARTESIAN_POINT('Ctrl Pts',(4.87476405531323,-0.226735633849849,
3.49073685167984));
#45730=CARTESIAN_POINT('Ctrl Pts',(4.89862197334465,0.0449962004486201,
3.44436221885167));
#45731=CARTESIAN_POINT('Ctrl Pts',(4.92247989137607,0.305725238065515,3.53385615878353));
#45732=CARTESIAN_POINT('Ctrl Pts',(4.94633780940749,0.491696127187109,3.73733496539613));
#45733=CARTESIAN_POINT('Ctrl Pts',(4.9701957274389,0.557433919677865,4.00504252782125));
#45734=CARTESIAN_POINT('Ctrl Pts',(4.99405364547033,0.486863934612277,4.27151705483839));
#45735=CARTESIAN_POINT('Ctrl Pts',(5.01791156350174,0.297242455626679,4.47159826597145));
#45736=CARTESIAN_POINT('Ctrl Pts',(5.04176948153317,0.0349370995184326,
4.55636085499566));
#45737=CARTESIAN_POINT('Ctrl Pts',(5.06562739956458,-0.235911329089554,
4.505078060008));
#45738=CARTESIAN_POINT('Ctrl Pts',(5.08948531759601,-0.449073011639563,
4.33028992129829));
#45739=CARTESIAN_POINT('Ctrl Pts',(5.11334323562741,-0.552424110340463,
4.07473689991432));
#45740=CARTESIAN_POINT('Ctrl Pts',(5.13720115365885,-0.520692466332485,
3.80090867070902));
#45741=CARTESIAN_POINT('Ctrl Pts',(5.16105907169026,-0.361637330928202,
3.57576369465428));
#45742=CARTESIAN_POINT('Ctrl Pts',(5.18491698972168,-0.114152017308863,
3.45435605122152));
#45743=CARTESIAN_POINT('Ctrl Pts',(5.2087749077531,0.161246573981014,3.46637321630784));
#45744=CARTESIAN_POINT('Ctrl Pts',(5.23263282578452,0.397215985664045,3.60887666570863));
#45745=CARTESIAN_POINT('Ctrl Pts',(5.25649074381594,0.536055268906009,3.84702042432939));
#45746=CARTESIAN_POINT('Ctrl Pts',(5.28034866184735,0.543814437048104,4.12257185628156));
#45747=CARTESIAN_POINT('Ctrl Pts',(5.30420657987878,0.418596162124088,4.3681511305826));
#45748=CARTESIAN_POINT('Ctrl Pts',(5.32806449791019,0.191019723230217,4.5237074252207));
#45749=CARTESIAN_POINT('Ctrl Pts',(5.35192241594161,-0.0832662412662402,
4.55120298888854));
#45750=CARTESIAN_POINT('Ctrl Pts',(5.37578033397303,-0.337191341646214,
4.44391440730515));
#45751=CARTESIAN_POINT('Ctrl Pts',(5.39963825200445,-0.508663974085987,
4.22807666114996));
#45752=CARTESIAN_POINT('Ctrl Pts',(5.42349617003587,-0.555754409133215,
3.95646795866016));
#45753=CARTESIAN_POINT('Ctrl Pts',(5.4473540880673,-0.466947752701331,3.69550402606682));
#45754=CARTESIAN_POINT('Ctrl Pts',(5.47121200609871,-0.263959651332346,
3.50899765340418));
#45755=CARTESIAN_POINT('Ctrl Pts',(5.49506992413013,0.00357377490351851,
3.44255472911916));
#45756=CARTESIAN_POINT('Ctrl Pts',(5.51892784216155,0.270233315828591,3.51242235806964));
#45757=CARTESIAN_POINT('Ctrl Pts',(5.54278576019296,0.470813450024345,3.70151600181885));
#45758=CARTESIAN_POINT('Ctrl Pts',(5.56664367822439,0.556266870991092,3.96359711366712));
#45759=CARTESIAN_POINT('Ctrl Pts',(5.5905015962558,0.505697889589837,4.23457972281303));
#45760=CARTESIAN_POINT('Ctrl Pts',(5.61435951428722,0.331471999260015,4.4482011999181));
#45761=CARTESIAN_POINT('Ctrl Pts',(5.63821743231864,0.0761921759760934,
4.55222527486821));
#45762=CARTESIAN_POINT('Ctrl Pts',(5.66207535035006,-0.197718709731212,
4.52121522783523));
#45763=CARTESIAN_POINT('Ctrl Pts',(5.68593326838148,-0.423281985227643,
4.3627538599096));
#45764=CARTESIAN_POINT('Ctrl Pts',(5.70979118641289,-0.545341285237878,
4.11558929214995));
#45765=CARTESIAN_POINT('Ctrl Pts',(5.73364910444432,-0.534049786451273,
3.84015999362387));
#45766=CARTESIAN_POINT('Ctrl Pts',(5.75750702247573,-0.392168567195948,
3.6038159310769));
#45767=CARTESIAN_POINT('Ctrl Pts',(5.78136494050716,-0.154391451667357,
3.46434966433946));
#45768=CARTESIAN_POINT('Ctrl Pts',(5.80522285853857,0.121138580962943,3.45586449715393));
#45769=CARTESIAN_POINT('Ctrl Pts',(5.82908077656999,0.367046927720705,3.58043527923202));
#45770=CARTESIAN_POINT('Ctrl Pts',(5.85293869460141,0.523202308305842,3.80760107017232));
#45771=CARTESIAN_POINT('Ctrl Pts',(5.87679661263283,0.551420461789987,4.08181362911724));
#45772=CARTESIAN_POINT('Ctrl Pts',(5.90065453066425,0.44480131269862,4.33602054829434));
#45773=CARTESIAN_POINT('Ctrl Pts',(5.92451244869567,0.229416087376931,4.50806125053784));
#45774=CARTESIAN_POINT('Ctrl Pts',(5.94837036672709,-0.042067546589846,
4.55586721297736));
#45775=CARTESIAN_POINT('Ctrl Pts',(5.97222828475851,-0.30326465903273,4.46774835821298));
#45776=CARTESIAN_POINT('Ctrl Pts',(5.99608620278993,-0.490305038147314,
4.26525255699254));
#45777=CARTESIAN_POINT('Ctrl Pts',(6.01994412082133,-0.557452977205748,
3.99789477357902));
#45778=CARTESIAN_POINT('Ctrl Pts',(6.04380203885278,-0.488287539408226,
3.73105273207384));
#45779=CARTESIAN_POINT('Ctrl Pts',(6.06765995688417,-0.299724270968661,
3.52997381710292));
#45780=CARTESIAN_POINT('Ctrl Pts',(6.09151787491561,-0.0378669053578504,
3.44383251805177));
#45781=CARTESIAN_POINT('Ctrl Pts',(6.11537579294702,0.233243627260218,3.49368287747685));
#45782=CARTESIAN_POINT('Ctrl Pts',(6.13923371097844,0.447331678364145,3.6673537262422));
#45783=CARTESIAN_POINT('Ctrl Pts',(6.16309162900986,0.552012406214274,3.92234268746235));
#45784=CARTESIAN_POINT('Ctrl Pts',(6.18694954704127,0.521753629494025,4.19636433484848));
#45785=CARTESIAN_POINT('Ctrl Pts',(6.2108074650727,0.363831507594212,4.42228768590875));
#45786=CARTESIAN_POINT('Ctrl Pts',(6.23466538310411,0.117094415953721,4.54510476979165));
#45787=CARTESIAN_POINT('Ctrl Pts',(6.25852330113554,-0.158561881267111,
4.53433708369694));
#45788=CARTESIAN_POINT('Ctrl Pts',(6.28238121916695,-0.394905399742298,
4.39345989467659));
#45789=CARTESIAN_POINT('Ctrl Pts',(6.30623913719837,-0.535697351746728,
4.1553358869807));
#45790=CARTESIAN_POINT('Ctrl Pts',(6.33009705522979,-0.543633587309765,
3.88114808171798));
#45791=CARTESIAN_POINT('Ctrl Pts',(6.36190761260502,-0.381130543103143,
3.54983775818315));
#45792=CARTESIAN_POINT('Ctrl Pts',(6.40167080932404,0.0904237977681596,
3.37418170676098));
#45793=CARTESIAN_POINT('Ctrl Pts',(6.4493866453869,0.576013642360818,3.73827828410759));
#45794=CARTESIAN_POINT('Ctrl Pts',(6.49710248144972,0.531303907723303,4.34259299019566));
#45795=CARTESIAN_POINT('Ctrl Pts',(6.54481831751257,-0.000617460830772086,
4.63236849138271));
#45796=CARTESIAN_POINT('Ctrl Pts',(6.5925341535754,-0.532336898979176,4.34139325430452));
#45797=CARTESIAN_POINT('Ctrl Pts',(6.64024998963824,-0.575010046738857,
3.73693099107234));
#45798=CARTESIAN_POINT('Ctrl Pts',(6.68796582570108,-0.0897448725589052,
3.37403863313417));
#45799=CARTESIAN_POINT('Ctrl Pts',(6.73568166176391,0.477988548433368,3.58598174571673));
#45800=CARTESIAN_POINT('Ctrl Pts',(6.78339749782676,0.606749053262868,4.17812127049189));
#45801=CARTESIAN_POINT('Ctrl Pts',(6.83111333388958,0.178337754027021,4.60669083891839));
#45802=CARTESIAN_POINT('Ctrl Pts',(6.87882916995244,-0.413851892207341,
4.47812605548031));
#45803=CARTESIAN_POINT('Ctrl Pts',(6.92654500601527,-0.625990718083913,
3.91049119230943));
#45804=CARTESIAN_POINT('Ctrl Pts',(6.97426084207811,-0.263274891453005,
3.42505341469988));
#45805=CARTESIAN_POINT('Ctrl Pts',(7.02197667814094,0.341211513798207,3.46759805477058));
#45806=CARTESIAN_POINT('Ctrl Pts',(7.06969251420378,0.63235750294684,3.99905552874491));
#45807=CARTESIAN_POINT('Ctrl Pts',(7.11740835026662,0.342800202184808,4.53138035934227));
#45808=CARTESIAN_POINT('Ctrl Pts',(7.16512418632946,-0.261555976381552,
4.57573041153878));
#45809=CARTESIAN_POINT('Ctrl Pts',(7.2128400223923,-0.625721183287191,4.0913783776429));
#45810=CARTESIAN_POINT('Ctrl Pts',(7.26055585845514,-0.41527704940159,3.52311216844965));
#45811=CARTESIAN_POINT('Ctrl Pts',(7.30827169451797,0.176522415171576,3.39277939551711));
#45812=CARTESIAN_POINT('Ctrl Pts',(7.35598753058081,0.606218615784068,3.8200666455489));
#45813=CARTESIAN_POINT('Ctrl Pts',(7.40370336664364,0.479214941044062,4.4125894643569));
#45814=CARTESIAN_POINT('Ctrl Pts',(7.4514192027065,-0.0878591916424711,
4.62622502914213));
#45815=CARTESIAN_POINT('Ctrl Pts',(7.49913503876932,-0.574250874682306,
4.26478851416677));
#45816=CARTESIAN_POINT('Ctrl Pts',(7.54685087483217,-0.53329914461431,3.6601926322252));
#45817=CARTESIAN_POINT('Ctrl Pts',(7.594566710895,-0.00261060360317682,
3.36764708477891));
#45818=CARTESIAN_POINT('Ctrl Pts',(7.64228254695784,0.530475294557976,3.65580094934904));
#45819=CARTESIAN_POINT('Ctrl Pts',(7.68999838302067,0.576417567478113,4.26003809833172));
#45820=CARTESIAN_POINT('Ctrl Pts',(7.73771421908353,0.093026718772369,4.62547826040714));
#45821=CARTESIAN_POINT('Ctrl Pts',(7.78543005514634,-0.475791997136335,
4.41653211173522));
#45822=CARTESIAN_POINT('Ctrl Pts',(7.8331458912092,-0.607683601098078,3.82507811568403));
#45823=CARTESIAN_POINT('Ctrl Pts',(7.88086172727203,-0.181530003744534,
3.39425757752065));
#45824=CARTESIAN_POINT('Ctrl Pts',(7.92857756333487,0.411325389238953,3.51969962646458));
#45825=CARTESIAN_POINT('Ctrl Pts',(7.97629339939771,0.626454348233276,4.08620889879763));
#45826=CARTESIAN_POINT('Ctrl Pts',(8.02400923546054,0.266300640003926,4.57355121287022));
#45827=CARTESIAN_POINT('Ctrl Pts',(8.07172507152339,-0.338401043502061,
4.5341926229444));
#45828=CARTESIAN_POINT('Ctrl Pts',(8.11944090758622,-0.632343841791292,
4.00427672775865));
#45829=CARTESIAN_POINT('Ctrl Pts',(8.16715674364906,-0.345595560302635,
3.47043344766624));
#45830=CARTESIAN_POINT('Ctrl Pts',(8.2148725797119,0.258518441882999,3.42289928101069));
#45831=CARTESIAN_POINT('Ctrl Pts',(8.26258841577473,0.625230981070026,3.90532558443901));
#45832=CARTESIAN_POINT('Ctrl Pts',(8.31030425183758,0.417784289925175,4.47469286043008));
#45833=CARTESIAN_POINT('Ctrl Pts',(8.35802008790041,-0.173320143095541,
4.60814237859973));
#45834=CARTESIAN_POINT('Ctrl Pts',(8.40573592396325,-0.605262021838435,
4.18312539302794));
#45835=CARTESIAN_POINT('Ctrl Pts',(8.45345176002609,-0.481382472773795,
3.58994154129225));
#45836=CARTESIAN_POINT('Ctrl Pts',(8.50116759608892,0.0845580080604409,
3.37332068174828));
#45837=CARTESIAN_POINT('Ctrl Pts',(8.54888343215178,0.572847569000584,3.73218908285563));
#45838=CARTESIAN_POINT('Ctrl Pts',(8.59659926821459,0.535082392934658,4.33699236997728));
#45839=CARTESIAN_POINT('Ctrl Pts',(8.64431510427745,0.00594282213592907,
4.6323303784547));
#45840=CARTESIAN_POINT('Ctrl Pts',(8.69203094034027,-0.528654133672296,
4.34698967074364));
#45841=CARTESIAN_POINT('Ctrl Pts',(8.73974677640312,-0.577779864139828,
3.74300300926635));
#45842=CARTESIAN_POINT('Ctrl Pts',(8.78746261246595,-0.0963214550818077,
3.37502063878676));
#45843=CARTESIAN_POINT('Ctrl Pts',(8.8351784485288,0.473590428273928,3.58096643225285));
#45844=CARTESIAN_POINT('Ctrl Pts',(8.88289428459164,0.608596934220305,4.17171719864135));
#45845=CARTESIAN_POINT('Ctrl Pts',(8.93061012065447,0.184719511004659,4.60477741930878));
#45846=CARTESIAN_POINT('Ctrl Pts',(8.97832595671731,-0.408788681441581,
4.48246123012823));
#45847=CARTESIAN_POINT('Ctrl Pts',(9.02604179278014,-0.626899937697651,
3.91709346970068));
#45848=CARTESIAN_POINT('Ctrl Pts',(9.07375762884299,-0.269319335070538,
3.42786005172794));
#45849=CARTESIAN_POINT('Ctrl Pts',(9.12147346490582,0.335581356962483,3.46403155175812));
#45850=CARTESIAN_POINT('Ctrl Pts',(9.16918930096866,0.632312525313962,3.99239112474344));
#45851=CARTESIAN_POINT('Ctrl Pts',(9.21690513703149,0.348381372290835,4.52773804495445));
#45852=CARTESIAN_POINT('Ctrl Pts',(9.26462097309434,-0.255473755443411,
4.5784549981902));
#45853=CARTESIAN_POINT('Ctrl Pts',(9.31233680915717,-0.624723402584967,
4.09796782591368));
#45854=CARTESIAN_POINT('Ctrl Pts',(9.36005264522002,-0.420279936527615,
3.52751529167185));
#45855=CARTESIAN_POINT('Ctrl Pts',(9.40776848128285,0.170113062081096,3.39095273519949));
#45856=CARTESIAN_POINT('Ctrl Pts',(9.45548431734569,0.604288618254829,3.81368765339017));
#45857=CARTESIAN_POINT('Ctrl Pts',(9.50320015340853,0.483536638109595,4.40751606625661));
#45858=CARTESIAN_POINT('Ctrl Pts',(9.55091598947137,-0.0812544769791981,
4.62711620503893));
#45859=CARTESIAN_POINT('Ctrl Pts',(9.5986318255342,-0.571428355597161,4.27082588331087));
#45860=CARTESIAN_POINT('Ctrl Pts',(9.64634766159704,-0.536850782714826,
3.66583198574659));
#45861=CARTESIAN_POINT('Ctrl Pts',(9.69406349765987,-0.0092748755543832,
3.36770971750703));
#45862=CARTESIAN_POINT('Ctrl Pts',(9.74177933372272,0.52681829253995,3.65022934471732));
#45863=CARTESIAN_POINT('Ctrl Pts',(9.78949516978555,0.579126116453474,4.253948746587));
#45864=CARTESIAN_POINT('Ctrl Pts',(9.83721100584839,0.099613516627068,4.62446310696212));
#45865=CARTESIAN_POINT('Ctrl Pts',(9.88492684191123,-0.471375708268938,
4.42152338761395));
#45866=CARTESIAN_POINT('Ctrl Pts',(9.93264267797408,-0.609493367214024,
3.83149225544889));
#45867=CARTESIAN_POINT('Ctrl Pts',(9.9803585140369,-0.187903888785556,3.39620437793004));
#45868=CARTESIAN_POINT('Ctrl Pts',(10.0280743500997,0.406240621987656,3.51539131074786));
#45869=CARTESIAN_POINT('Ctrl Pts',(10.0757901861626,0.627328118774167,4.07960185956908));
#45870=CARTESIAN_POINT('Ctrl Pts',(10.1235060222254,0.27233055140652,4.57071279591595));
#45871=CARTESIAN_POINT('Ctrl Pts',(10.1712218582883,-0.332752351661881,
4.5377293902281));
#45872=CARTESIAN_POINT('Ctrl Pts',(10.2189376943511,-0.632263650146131,
4.01094081146358));
#45873=CARTESIAN_POINT('Ctrl Pts',(10.2666535304139,-0.351157510074434,
3.47410511718603));
#45874=CARTESIAN_POINT('Ctrl Pts',(10.3143693664768,0.252421974751429,3.42020678572945));
#45875=CARTESIAN_POINT('Ctrl Pts',(10.3620852025396,0.624198476151732,3.89874148420283));
#45876=CARTESIAN_POINT('Ctrl Pts',(10.4098010386024,0.422763912373798,4.47026343579529));
#45877=CARTESIAN_POINT('Ctrl Pts',(10.4575168746653,-0.166901257195935,
4.60993523836389));
#45878=CARTESIAN_POINT('Ctrl Pts',(10.5052327107281,-0.603298434176698,
4.18949412648294));
#45879=CARTESIAN_POINT('Ctrl Pts',(10.552948546791,-0.485677376113382,3.5950376425108));
#45880=CARTESIAN_POINT('Ctrl Pts',(10.6006643828538,0.0779486895418537,
3.3724643225678));
#45881=CARTESIAN_POINT('Ctrl Pts',(10.6483802189166,0.569993274196054,3.72616667108832));
#45882=CARTESIAN_POINT('Ctrl Pts',(10.6960960549795,0.538604264682155,4.3313343790158));
#45883=CARTESIAN_POINT('Ctrl Pts',(10.7438118910423,0.0126066714187673,
4.63223262845832));
#45884=CARTESIAN_POINT('Ctrl Pts',(10.7915277271052,-0.524967822187051,
4.35254192703816));
#45885=CARTESIAN_POINT('Ctrl Pts',(10.839243563168,-0.580456287010268,3.74910654946403));
#45886=CARTESIAN_POINT('Ctrl Pts',(10.8869593992308,-0.102902812003948,
3.37607048800905));
#45887=CARTESIAN_POINT('Ctrl Pts',(10.9346752352937,0.469147898628881,3.5759984978049));
#45888=CARTESIAN_POINT('Ctrl Pts',(10.9823910713565,0.610372875182502,4.16529361116822));
#45889=CARTESIAN_POINT('Ctrl Pts',(11.0301069074193,0.191083048662156,4.60279705802663));
#45890=CARTESIAN_POINT('Ctrl Pts',(11.0778227434822,-0.403681281635282,
4.48674269127424));
#45891=CARTESIAN_POINT('Ctrl Pts',(11.125538579545,-0.627738879572117,3.92370502162571));
#45892=CARTESIAN_POINT('Ctrl Pts',(11.1732544156079,-0.275334205393669,
3.43073020456744));
#45893=CARTESIAN_POINT('Ctrl Pts',(11.2209702516707,0.329914106159097,3.46052459999659));
#45894=CARTESIAN_POINT('Ctrl Pts',(11.2686860877335,0.632197217644931,3.98572755614488));
#45895=CARTESIAN_POINT('Ctrl Pts',(11.3164019237964,0.353923896562866,4.52403711709511));
#45896=CARTESIAN_POINT('Ctrl Pts',(11.3641177598592,-0.24936318455202,4.58111533006939));
#45897=CARTESIAN_POINT('Ctrl Pts',(11.411833595922,-0.623656216347001,4.10454639383227));
#45898=CARTESIAN_POINT('Ctrl Pts',(11.4595494319849,-0.425236148486169,
3.53197089548594));
#45899=CARTESIAN_POINT('Ctrl Pts',(11.5072652680477,0.163684817628688,3.3891937253683));
#45900=CARTESIAN_POINT('Ctrl Pts',(11.5549811041106,0.602291497100466,3.80732935570755));
#45901=CARTESIAN_POINT('Ctrl Pts',(11.6026969401734,0.487804627338989,4.40239740331947));
#45902=CARTESIAN_POINT('Ctrl Pts',(11.6504127762363,-0.0746407375468588,
4.62793772378323));
#45903=CARTESIAN_POINT('Ctrl Pts',(11.6981286122991,-0.568542364648052,
4.276833170433));
#45904=CARTESIAN_POINT('Ctrl Pts',(11.7458444483619,-0.540342790144192,
3.67150845704832));
#45905=CARTESIAN_POINT('Ctrl Pts',(11.7935602844247,-0.0159381172083995,
3.36784258204823));
#45906=CARTESIAN_POINT('Ctrl Pts',(11.8412761204876,0.523102773999324,3.64469659094542));
#45907=CARTESIAN_POINT('Ctrl Pts',(11.8889919565504,0.581770338872691,4.24783118742311));
#45908=CARTESIAN_POINT('Ctrl Pts',(11.9367077926133,0.106189249871976,4.62337859111715));
#45909=CARTESIAN_POINT('Ctrl Pts',(11.9844236286761,-0.466907061217805,
4.4264678426758));
#45910=CARTESIAN_POINT('Ctrl Pts',(12.0321394647389,-0.611235433702689,
3.83792511225401));
#45911=CARTESIAN_POINT('Ctrl Pts',(12.0798553008018,-0.19425690235234,3.39821824509208));
#45912=CARTESIAN_POINT('Ctrl Pts',(12.1275711368646,0.401110731454808,3.51113682306459));
#45913=CARTESIAN_POINT('Ctrl Pts',(12.1752869729275,0.628132208685083,4.07298597854376));
#45914=CARTESIAN_POINT('Ctrl Pts',(12.2230028089903,0.27833021362349,4.56781098689255));
#45915=CARTESIAN_POINT('Ctrl Pts',(12.2707186450531,-0.327066699269377,
4.54120642908287));
#45916=CARTESIAN_POINT('Ctrl Pts',(12.3184344811159,-0.632113229655128,
4.01760367991507));
#45917=CARTESIAN_POINT('Ctrl Pts',(12.3661503171788,-0.356680454936339,
3.47783520061383));
#45918=CARTESIAN_POINT('Ctrl Pts',(12.4138661532416,0.246297469784735,3.4175786911271));
#45919=CARTESIAN_POINT('Ctrl Pts',(12.4615819893045,0.623096638228782,3.89216863128209));
#45920=CARTESIAN_POINT('Ctrl Pts',(12.5092978253673,0.427696576213203,4.46578177652963));
#45921=CARTESIAN_POINT('Ctrl Pts',(12.5570136614302,-0.16046383269669,4.61166034941614));
#45922=CARTESIAN_POINT('Ctrl Pts',(12.604729497493,-0.601267834987779,4.1958418118296));
#45923=CARTESIAN_POINT('Ctrl Pts',(12.6524453335558,-0.489918332714758,
3.60017872502631));
#45924=CARTESIAN_POINT('Ctrl Pts',(12.7001611696187,0.0713307128527425,
3.37167766707246));
#45925=CARTESIAN_POINT('Ctrl Pts',(12.7478770056815,0.56707566724347,3.72017467542775));
#45926=CARTESIAN_POINT('Ctrl Pts',(12.7955928417444,0.542066310823814,4.32563958500381));
#45927=CARTESIAN_POINT('Ctrl Pts',(12.8433086778072,0.0192691204123526,
4.63206465306178));
#45928=CARTESIAN_POINT('Ctrl Pts',(12.89102451387,-0.521223199767296,4.35805502464836));
#45929=CARTESIAN_POINT('Ctrl Pts',(12.9387403499329,-0.583068235550835,
3.7552379577156));
#45930=CARTESIAN_POINT('Ctrl Pts',(12.9864561859957,-0.109472738970043,
3.37718964036075));
#45931=CARTESIAN_POINT('Ctrl Pts',(13.0341720220585,0.464653258261548,3.57107765943178));
#45932=CARTESIAN_POINT('Ctrl Pts',(13.0818878581214,0.612081018822183,4.15885166366515));
#45933=CARTESIAN_POINT('Ctrl Pts',(13.1296036941842,0.197425361721354,4.6007497409078));
#45934=CARTESIAN_POINT('Ctrl Pts',(13.177319530247,-0.398529042827853,4.49097008735187));
#45935=CARTESIAN_POINT('Ctrl Pts',(13.2250353663099,-0.628508095190705,
3.93032504803489));
#45936=CARTESIAN_POINT('Ctrl Pts',(13.2727512023727,-0.281318492899819,
3.4336635891944));
#45937=CARTESIAN_POINT('Ctrl Pts',(13.3204670384356,0.324210210062374,3.45707757060249));
#45938=CARTESIAN_POINT('Ctrl Pts',(13.3681828744984,0.632011688508986,3.97906557286167));
#45939=CARTESIAN_POINT('Ctrl Pts',(13.4158987105612,0.359427108647973,4.52027798167956));
#45940=CARTESIAN_POINT('Ctrl Pts',(13.4636145466241,-0.243224915581421,
4.58371111441534));
#45941=CARTESIAN_POINT('Ctrl Pts',(13.5113303826869,-0.622519757336015,
4.11111334923356));
#45942=CARTESIAN_POINT('Ctrl Pts',(13.5590462187498,-0.430145127231255,
3.53647848575196));
#45943=CARTESIAN_POINT('Ctrl Pts',(13.6067620548126,0.157238391843492,3.38750256099959));
#45944=CARTESIAN_POINT('Ctrl Pts',(13.6544778908755,0.600227476264717,3.8009924589658));
#45945=CARTESIAN_POINT('Ctrl Pts',(13.7021937269383,0.492018433545193,4.39723404398833));
#45946=CARTESIAN_POINT('Ctrl Pts',(13.7499095630011,-0.0680187073756014,
4.62868949418496));
#45947=CARTESIAN_POINT('Ctrl Pts',(13.797625399064,-0.565593222711038,4.28280970824024));
#45948=CARTESIAN_POINT('Ctrl Pts',(13.8453412351268,-0.543774778860562,
3.67722141563181));
#45949=CARTESIAN_POINT('Ctrl Pts',(13.8930570711896,-0.0225995885319848,
3.36804566363559));
#45950=CARTESIAN_POINT('Ctrl Pts',(13.9407729072525,0.519329151684885,3.63920330259016));
#45951=CARTESIAN_POINT('Ctrl Pts',(13.9884887433153,0.584349941003394,4.24168610034696));
#45952=CARTESIAN_POINT('Ctrl Pts',(14.0362045793781,0.112753188118911,4.62222483333648));
#45953=CARTESIAN_POINT('Ctrl Pts',(14.083920415441,-0.462386552345973,4.43136492771341));
#45954=CARTESIAN_POINT('Ctrl Pts',(14.1316362515038,-0.612909607059929,
3.84437597156854));
#45955=CARTESIAN_POINT('Ctrl Pts',(14.1793520875667,-0.200588338784227,
3.40029895531576));
#45956=CARTESIAN_POINT('Ctrl Pts',(14.2270679236295,0.395936287445344,3.50693663598317));
#45957=CARTESIAN_POINT('Ctrl Pts',(14.2747837596923,0.628866528650988,4.06636199058228));
#45958=CARTESIAN_POINT('Ctrl Pts',(14.3224995957552,0.284298960241116,4.5648461081192));
#45959=CARTESIAN_POINT('Ctrl Pts',(14.370215431818,-0.321344717859966,4.54462335329573));
#45960=CARTESIAN_POINT('Ctrl Pts',(14.4179312678809,-0.631892597026201,
4.02426459303334));
#45961=CARTESIAN_POINT('Ctrl Pts',(14.4656471039437,-0.362163781425906,
3.48162328362967));
#45962=CARTESIAN_POINT('Ctrl Pts',(14.5133629400065,0.240145607263868,3.41501528911991));
#45963=CARTESIAN_POINT('Ctrl Pts',(14.5610787760693,0.6219255896881,3.8856077557581));
#45964=CARTESIAN_POINT('Ctrl Pts',(14.6087946121322,0.432581733546503,4.46124838043455));
#45965=CARTESIAN_POINT('Ctrl Pts',(14.656510448195,-0.154008584636381,4.61331752013935));
#45966=CARTESIAN_POINT('Ctrl Pts',(14.7042262842579,-0.599170449821005,
4.20216774399712));
#45967=CARTESIAN_POINT('Ctrl Pts',(14.7519421203207,-0.494104871512583,
3.60536421779174));
#45968=CARTESIAN_POINT('Ctrl Pts',(14.7996579563836,0.0647048130865326,
3.37096080264023));
#45969=CARTESIAN_POINT('Ctrl Pts',(14.8473737924464,0.564095072216763,3.71421376143635));
#45970=CARTESIAN_POINT('Ctrl Pts',(14.8950896285093,0.545468146811986,4.319908620492));
#45971=CARTESIAN_POINT('Ctrl Pts',(14.942805464572,0.0259294290834894,4.63182647092298));
#45972=CARTESIAN_POINT('Ctrl Pts',(14.9905213006349,-0.517420682347921,
4.36352835120552));
#45973=CARTESIAN_POINT('Ctrl Pts',(15.0382371366977,-0.585615419638682,
3.76139655297334));
#45974=CARTESIAN_POINT('Ctrl Pts',(15.0859529727606,-0.116030506223773,
3.3783779715317));
#45975=CARTESIAN_POINT('Ctrl Pts',(15.1336688088234,0.460107006415252,3.56620446371685));
#45976=CARTESIAN_POINT('Ctrl Pts',(15.1813846448862,0.613721175406852,4.15239207167311));
#45977=CARTESIAN_POINT('Ctrl Pts',(15.2291004809491,0.203745745708236,4.59863569535852));
#45978=CARTESIAN_POINT('Ctrl Pts',(15.2768163170119,-0.393332537305518,
4.49514294880206));
#45979=CARTESIAN_POINT('Ctrl Pts',(15.3245321530748,-0.629207499112597,
3.93695281360709));
#45980=CARTESIAN_POINT('Ctrl Pts',(15.3722479891376,-0.287271532882751,
3.43665987978239));
#45981=CARTESIAN_POINT('Ctrl Pts',(15.4199638252004,0.318470302234025,3.45369084645546));
#45982=CARTESIAN_POINT('Ctrl Pts',(15.4676796612633,0.631755958513824,3.97240591487529));
#45983=CARTESIAN_POINT('Ctrl Pts',(15.5153954973261,0.364890397275464,4.51646105625472));
#45984=CARTESIAN_POINT('Ctrl Pts',(15.563111333389,-0.237059630341402,4.58624206290064));
#45985=CARTESIAN_POINT('Ctrl Pts',(15.6108271694518,-0.621314151784485,
4.11766796269128));
#45986=CARTESIAN_POINT('Ctrl Pts',(15.6585430055147,-0.435006327496808,
3.54103756178819));
#45987=CARTESIAN_POINT('Ctrl Pts',(15.7062588415774,0.150774500763906,3.38587942993986));
#45988=CARTESIAN_POINT('Ctrl Pts',(15.7539746776403,0.598096785009218,3.79467766703735));
#45989=CARTESIAN_POINT('Ctrl Pts',(15.8016905137032,0.496177588678611,4.39202656178461));
#45990=CARTESIAN_POINT('Ctrl Pts',(15.849406349766,-0.0613891220090978,
4.62937143274106));
#45991=CARTESIAN_POINT('Ctrl Pts',(15.8971221858288,-0.562581257362808,
4.28875483288714));
#45992=CARTESIAN_POINT('Ctrl Pts',(15.9448380218917,-0.547146367654922,
3.68297022692873));
#45993=CARTESIAN_POINT('Ctrl Pts',(15.9925538579545,-0.0292585496004989,
3.36831893971177));
#45994=CARTESIAN_POINT('Ctrl Pts',(16.0402696940173,0.515497844752703,3.63375008981994));
#45995=CARTESIAN_POINT('Ctrl Pts',(16.0879855300802,0.586864636315616,4.23551416792571));
#45996=CARTESIAN_POINT('Ctrl Pts',(16.135701366143,0.119304602276749,4.62100196177401));
#45997=CARTESIAN_POINT('Ctrl Pts',(16.1834172022059,-0.457814683770117,
4.43621409878185));
#45998=CARTESIAN_POINT('Ctrl Pts',(16.2311330382687,-0.614515701326505,
3.85084411686165));
#45999=CARTESIAN_POINT('Ctrl Pts',(16.2788488743316,-0.206897494815317,
3.40244627748567));
#46000=CARTESIAN_POINT('Ctrl Pts',(16.3265647103943,0.390717864711932,3.50279121604045));
#46001=CARTESIAN_POINT('Ctrl Pts',(16.3742805464572,0.629530997107116,4.05973063144581));
#46002=CARTESIAN_POINT('Ctrl Pts',(16.42199638252,0.290236128279341,4.56181848892059));
#46003=CARTESIAN_POINT('Ctrl Pts',(16.4697122185829,-0.315587043004215,
4.54797978333095));
#46004=CARTESIAN_POINT('Ctrl Pts',(16.5174280546457,-0.631601776766168,
4.03092281095576));
#46005=CARTESIAN_POINT('Ctrl Pts',(16.5651438907086,-0.367606880481235,
3.48546894547127));
#46006=CARTESIAN_POINT('Ctrl Pts',(16.6128597267714,0.233967070508539,3.41251686443844));
#46007=CARTESIAN_POINT('Ctrl Pts',(16.6605755628343,0.620685460604191,3.87905958638177));
#46008=CARTESIAN_POINT('Ctrl Pts',(16.7082913988971,0.437418841753611,4.45666375105816));
#46009=CARTESIAN_POINT('Ctrl Pts',(16.7560072349599,-0.147536230033309,
4.61490656646286));
#46010=CARTESIAN_POINT('Ctrl Pts',(16.8037230710227,-0.597006511643959,
4.20847122033102));
#46011=CARTESIAN_POINT('Ctrl Pts',(16.8514389070856,-0.498236527486006,
3.61059354482716));
#46012=CARTESIAN_POINT('Ctrl Pts',(16.8991547431484,0.058071726216741,3.37031380889701));
#46013=CARTESIAN_POINT('Ctrl Pts',(16.9468705792113,0.561051820186282,3.70828459122417));
#46014=CARTESIAN_POINT('Ctrl Pts',(16.9945864152741,0.548809394786867,4.31414212204871));
#46015=CARTESIAN_POINT('Ctrl Pts',(17.0423022513369,0.0325868576366809,
4.63151810849805));
#46016=CARTESIAN_POINT('Ctrl Pts',(17.0900180873998,-0.513560692294518,
4.3689612987585));
#46017=CARTESIAN_POINT('Ctrl Pts',(17.1377339234626,-0.588097556344686,
3.76758165116972));
#46018=CARTESIAN_POINT('Ctrl Pts',(17.1854497595255,-0.122575385359494,
3.37963534952775));
#46019=CARTESIAN_POINT('Ctrl Pts',(17.2331655955883,0.455509648066065,3.56137945195155));
#46020=CARTESIAN_POINT('Ctrl Pts',(17.2808814316511,0.615293162755707,4.14591555269289));
#46021=CARTESIAN_POINT('Ctrl Pts',(17.328597267714,0.210043498584534,4.59645515619697));
#46022=CARTESIAN_POINT('Ctrl Pts',(17.3763131037768,-0.388092342271454,
4.49926081212312));
#46023=CARTESIAN_POINT('Ctrl Pts',(17.4240289398397,-0.629837013651323,
3.94358758216158));
#46024=CARTESIAN_POINT('Ctrl Pts',(17.4717447759025,-0.293192664107019,
3.43971874351766));
#46025=CARTESIAN_POINT('Ctrl Pts',(17.5194606119653,0.312695020235776,3.45036480373676));
#46026=CARTESIAN_POINT('Ctrl Pts',(17.5671764480282,0.631430056064715,3.96574932190893));
#46027=CARTESIAN_POINT('Ctrl Pts',(17.614892284091,0.370313155609181,4.51258676478657));
#46028=CARTESIAN_POINT('Ctrl Pts',(17.6626081201539,-0.230868013642575,
4.58870789439952));
#46029=CARTESIAN_POINT('Ctrl Pts',(17.7103239562166,-0.620039533605355,
4.12420950615009));
#46030=CARTESIAN_POINT('Ctrl Pts',(17.7580397922796,-0.43981920932378,3.54564761719411));
#46031=CARTESIAN_POINT('Ctrl Pts',(17.8057556283423,0.144293862368219,3.38432451247882));
#46032=CARTESIAN_POINT('Ctrl Pts',(17.8534714644052,0.595899660001039,3.78838568133928));
#46033=CARTESIAN_POINT('Ctrl Pts',(17.901187300468,0.500281630760053,4.38677553513073));
#46034=CARTESIAN_POINT('Ctrl Pts',(17.9489031365309,-0.0547527178302441,
4.62998346370502));
#46035=CARTESIAN_POINT('Ctrl Pts',(17.9966189725937,-0.559506803158163,
4.29466788401745));
#46036=CARTESIAN_POINT('Ctrl Pts',(18.0443348086565,-0.550457182027191,
3.68875425238845));
#46037=CARTESIAN_POINT('Ctrl Pts',(18.0920506447194,-0.0359142607682062,
3.36866237992255));
#46038=CARTESIAN_POINT('Ctrl Pts',(18.1397664807822,0.511609278766163,3.62833755835171));
#46039=CARTESIAN_POINT('Ctrl Pts',(18.187482316845,0.589314145488933,4.22931607570827));
#46040=CARTESIAN_POINT('Ctrl Pts',(18.2351981529079,0.12584276464555,4.61971011226051));
#46041=CARTESIAN_POINT('Ctrl Pts',(18.2829139889707,-0.453191963311679,
4.44101481725822));
#46042=CARTESIAN_POINT('Ctrl Pts',(18.3306298250336,-0.616053538105107,
3.85732882968247));
#46043=CARTESIAN_POINT('Ctrl Pts',(18.3783456610964,-0.213183669654489,
3.40465997308746));
#46044=CARTESIAN_POINT('Ctrl Pts',(18.4260614971592,0.385456042892229,3.49870102369));
#46045=CARTESIAN_POINT('Ctrl Pts',(18.4737773332221,0.630125540247444,4.05309263771424));
#46046=CARTESIAN_POINT('Ctrl Pts',(18.5214931692849,0.296141058265729,4.55872846559028));
#46047=CARTESIAN_POINT('Ctrl Pts',(18.5692090053478,-0.309794314237323,
4.55127534637221));
#46048=CARTESIAN_POINT('Ctrl Pts',(18.6169248414106,-0.631240801177943,
4.0375775941191));
#46049=CARTESIAN_POINT('Ctrl Pts',(18.6646406774734,-0.373009147508776,
3.4893717589807));
#46050=CARTESIAN_POINT('Ctrl Pts',(18.7123565135363,0.227762545801372,3.41008369459593));
#46051=CARTESIAN_POINT('Ctrl Pts',(18.7600723495991,0.619376388724522,3.87252485049244));
#46052=CARTESIAN_POINT('Ctrl Pts',(18.8077881856619,0.442207363551868,4.45202839763978));
#46053=CARTESIAN_POINT('Ctrl Pts',(18.8555040217248,-0.141047487806633,
4.61642731188217));
#46054=CARTESIAN_POINT('Ctrl Pts',(18.9032198577876,-0.594776260815313,
4.21475154067248));
#46055=CARTESIAN_POINT('Ctrl Pts',(18.9509356938505,-0.502312841712761,
3.615866125281));
#46056=CARTESIAN_POINT('Ctrl Pts',(18.9986515299133,0.0514321890198641,
3.36973675771293));
#46057=CARTESIAN_POINT('Ctrl Pts',(19.0463673659762,0.557946249173174,3.70238782336559));
#46058=CARTESIAN_POINT('Ctrl Pts',(19.0940832020389,0.552089683635207,4.30834073020757));
#46059=CARTESIAN_POINT('Ctrl Pts',(19.1417990381018,0.0392406665648073,
4.63113960000379));
#46060=CARTESIAN_POINT('Ctrl Pts',(19.1895148741646,-0.509643658296843,
4.3743532639067));
#46061=CARTESIAN_POINT('Ctrl Pts',(19.2372307102275,-0.590514370077448,
3.77379256516987));
#46062=CARTESIAN_POINT('Ctrl Pts',(19.2849465462903,-0.129106649190522,
3.38096163491845));
#46063=CARTESIAN_POINT('Ctrl Pts',(19.3326623823532,0.450861693465423,3.55660315963506));
#46064=CARTESIAN_POINT('Ctrl Pts',(19.380378218416,0.616796807017627,4.1394228269368));
#46065=CARTESIAN_POINT('Ctrl Pts',(19.4280940544789,0.216317919394901,4.59420836405745));
#46066=CARTESIAN_POINT('Ctrl Pts',(19.4758098905416,-0.382809037079938,
4.50332322288615));
#46067=CARTESIAN_POINT('Ctrl Pts',(19.5235257266046,-0.630396573984801,
3.95022861114352));
#46068=CARTESIAN_POINT('Ctrl Pts',(19.5712415626673,-0.299081219248977,
3.44283985120298));
#46069=CARTESIAN_POINT('Ctrl Pts',(19.6189573987302,0.306884987370396,3.44709979193512));
#46070=CARTESIAN_POINT('Ctrl Pts',(19.666673234793,0.631034051704256,3.95909657101937));
#46071=CARTESIAN_POINT('Ctrl Pts',(19.7143890708559,0.375694716468479,4.50865546647685));
#46072=CARTESIAN_POINT('Ctrl Pts',(19.7621049069187,-0.224650630777236,
4.59110846933868));
#46073=CARTESIAN_POINT('Ctrl Pts',(19.8098207429815,-0.618696275574682,
4.13073699938377));
#46074=CARTESIAN_POINT('Ctrl Pts',(19.8575365790444,-0.44458280157215,3.55030861879767));
#46075=CARTESIAN_POINT('Ctrl Pts',(19.9052524151072,0.13779637220375,3.3828370770856));
#46076=CARTESIAN_POINT('Ctrl Pts',(19.9529682511701,0.593637901716091,3.7821189081517));
#46077=CARTESIAN_POINT('Ctrl Pts',(20.0006840872329,0.504327165075627,4.38147832337345));
#46078=CARTESIAN_POINT('Ctrl Pts',(20.0483999232957,-0.0481046828163007,
4.63053160650705));
#46079=CARTESIAN_POINT('Ctrl Pts',(20.0961157593586,-0.556380679578279,
4.30053671048834));
#46080=CARTESIAN_POINT('Ctrl Pts',(20.1438315954214,-0.553687069357429,
3.69459455385474));
#46081=CARTESIAN_POINT('Ctrl Pts',(20.1915474314843,-0.0426033430871586,
3.36903495876776));
#46082=CARTESIAN_POINT('Ctrl Pts',(20.2392632675471,0.507734449822709,3.62304374442814));
#46083=CARTESIAN_POINT('Ctrl Pts',(20.2869791036099,0.591564791291533,4.22294595084339));
#46084=CARTESIAN_POINT('Ctrl Pts',(20.3346949396728,0.132620199007312,4.618629012875));
#46085=CARTESIAN_POINT('Ctrl Pts',(20.3824107757356,-0.449008129734859,
4.44521533979349));
#46086=CARTESIAN_POINT('Ctrl Pts',(20.4221739724547,-0.588594799935545,
3.96175478680276));
#46087=CARTESIAN_POINT('Ctrl Pts',(20.4539845298298,-0.419131055782338,
3.63395025773895));
#46088=CARTESIAN_POINT('Ctrl Pts',(20.4778424478613,-0.194099195253748,
3.47709810398663));
#46089=CARTESIAN_POINT('Ctrl Pts',(20.5017003658927,0.0810471032980313,
3.44846366347126));
#46090=CARTESIAN_POINT('Ctrl Pts',(20.5255582839241,0.334940048200093,3.55449674151986));
#46091=CARTESIAN_POINT('Ctrl Pts',(20.5494162019556,0.507694843328107,3.76957374638464));
#46092=CARTESIAN_POINT('Ctrl Pts',(20.5732741199869,0.555899439471162,4.04093981905292));
#46093=CARTESIAN_POINT('Ctrl Pts',(20.5971320380184,0.468386015874758,4.30232489481291));
#46094=CARTESIAN_POINT('Ctrl Pts',(20.6209899560498,0.266225827016684,4.48976745893774));
#46095=CARTESIAN_POINT('Ctrl Pts',(20.6448478740812,-0.000973650874560818,
4.55745692740964));
#46096=CARTESIAN_POINT('Ctrl Pts',(20.6687057921126,-0.267966914960919,
4.48882854939535));
#46097=CARTESIAN_POINT('Ctrl Pts',(20.6925637101441,-0.469418090387657,
4.30067062862012));
#46098=CARTESIAN_POINT('Ctrl Pts',(20.7164216281755,-0.556092695039732,
4.03898930289119));
#46099=CARTESIAN_POINT('Ctrl Pts',(20.7402795462069,-0.506782753954552,
3.7677746905255));
#46100=CARTESIAN_POINT('Ctrl Pts',(20.7641374642383,-0.333553132261349,
3.55334514249538));
#46101=CARTESIAN_POINT('Ctrl Pts',(20.7879953822697,-0.0787593560922578,
3.44813505886707));
#46102=CARTESIAN_POINT('Ctrl Pts',(20.8118533003012,0.19529252477751,3.47787088781106));
#46103=CARTESIAN_POINT('Ctrl Pts',(20.8357112183325,0.421590436108717,3.63528155911584));
#46104=CARTESIAN_POINT('Ctrl Pts',(20.859569136364,0.544797804677434,3.8818757964511));
#46105=CARTESIAN_POINT('Ctrl Pts',(20.8834270543954,0.534787374467886,4.15735463375504));
#46106=CARTESIAN_POINT('Ctrl Pts',(20.9072849724269,0.394006808563119,4.39435596913946));
#46107=CARTESIAN_POINT('Ctrl Pts',(20.9311428904582,0.156880874733563,4.53492653211281));
#46108=CARTESIAN_POINT('Ctrl Pts',(20.9550008084897,-0.118606721834374,
4.54469298471526));
#46109=CARTESIAN_POINT('Ctrl Pts',(20.9788587265211,-0.365091735913813,
4.42126716656144));
#46110=CARTESIAN_POINT('Ctrl Pts',(21.0027166445525,-0.522301880015273,
4.19483005048941));
#46111=CARTESIAN_POINT('Ctrl Pts',(21.0265745625839,-0.55179498493052,3.92075168033001));
#46112=CARTESIAN_POINT('Ctrl Pts',(21.0504324806153,-0.446359186657349,
3.66605168284066));
#46113=CARTESIAN_POINT('Ctrl Pts',(21.0742903986468,-0.231776408019839,
3.49301114555638));
#46114=CARTESIAN_POINT('Ctrl Pts',(21.0981483166782,0.0394820154987394,
3.44394319323497));
#46115=CARTESIAN_POINT('Ctrl Pts',(21.1220062347096,0.301086010940692,3.5308462768762));
#46116=CARTESIAN_POINT('Ctrl Pts',(21.145864152741,0.489066275193333,3.73247022529863));
#46117=CARTESIAN_POINT('Ctrl Pts',(21.1697220707724,0.557456513314207,3.9995124910074));
#46118=CARTESIAN_POINT('Ctrl Pts',(21.1935799888039,0.489533449092281,4.26667396594056));
#46119=CARTESIAN_POINT('Ctrl Pts',(21.2174379068352,0.30190612195814,4.46862639215028));
#46120=CARTESIAN_POINT('Ctrl Pts',(21.2412958248667,0.0404545242400231,
4.55598690035157));
#46121=CARTESIAN_POINT('Ctrl Pts',(21.2651537428981,-0.230889306609896,
4.50739346663836));
#46122=CARTESIAN_POINT('Ctrl Pts',(21.2890116609295,-0.445774412697373,
4.33472850921124));
#46123=CARTESIAN_POINT('Ctrl Pts',(21.312869578961,-0.551655532228011,4.08021331346062));
#46124=CARTESIAN_POINT('Ctrl Pts',(21.3367274969923,-0.522641847334507,
3.80608377760199));
#46125=CARTESIAN_POINT('Ctrl Pts',(21.3605854150238,-0.365827994289322,
3.57937204029158));
#46126=CARTESIAN_POINT('Ctrl Pts',(21.3844433330552,-0.119559231686077,
3.45551529680541));
#46127=CARTESIAN_POINT('Ctrl Pts',(21.4083012510867,0.155945019792583,3.46479989471587));
#46128=CARTESIAN_POINT('Ctrl Pts',(21.432159169118,0.393316466074861,3.60495549692644));
#46129=CARTESIAN_POINT('Ctrl Pts',(21.4560170871495,0.534511322676435,3.84171024093472));
#46130=CARTESIAN_POINT('Ctrl Pts',(21.4798750051809,0.545003601087511,4.11717114276091));
#46131=CARTESIAN_POINT('Ctrl Pts',(21.5037329232123,0.422227653432673,4.36398050850424));
#46132=CARTESIAN_POINT('Ctrl Pts',(21.5275908412437,0.196205543263173,4.52178672528827));
#46133=CARTESIAN_POINT('Ctrl Pts',(21.5514487592751,-0.0777941667658609,
4.5520018745543));
#46134=CARTESIAN_POINT('Ctrl Pts',(21.5753066773066,-0.332771083950078,
4.44723752926263));
#46135=CARTESIAN_POINT('Ctrl Pts',(21.5991645953379,-0.506376406606172,
4.23311142556056));
#46136=CARTESIAN_POINT('Ctrl Pts',(21.6230225133694,-0.556158904430687,
3.96198322848119));
#46137=CARTESIAN_POINT('Ctrl Pts',(21.6468804314008,-0.469945400657515,
3.70015116759423));
#46138=CARTESIAN_POINT('Ctrl Pts',(21.6707383494323,-0.268817445367881,
3.51164031394868));
#46139=CARTESIAN_POINT('Ctrl Pts',(21.6945962674636,-0.00195630224560004,
3.44254670619344));
#46140=CARTESIAN_POINT('Ctrl Pts',(21.7184541854951,0.26538321006433,3.50976561349676));
#46141=CARTESIAN_POINT('Ctrl Pts',(21.7423121035264,0.467829298620023,3.6968601820167));
#46142=CARTESIAN_POINT('Ctrl Pts',(21.766170021558,0.555878380248887,3.95808069339639));
#46143=CARTESIAN_POINT('Ctrl Pts',(21.7900279395893,0.508000056083844,4.22955161709966));
#46144=CARTESIAN_POINT('Ctrl Pts',(21.8138858576208,0.335901880562604,4.44489091756156));
#46145=CARTESIAN_POINT('Ctrl Pts',(21.8377437756521,0.0816665454602928,
4.55144227009437));
#46146=CARTESIAN_POINT('Ctrl Pts',(21.8616016936836,-0.192538484559094,
4.52315096660328));
#46147=CARTESIAN_POINT('Ctrl Pts',(21.885459611715,-0.419662610460766,4.36693500143146));
#46148=CARTESIAN_POINT('Ctrl Pts',(21.9093175297464,-0.544167796724789,
4.12099343330092));
#46149=CARTESIAN_POINT('Ctrl Pts',(21.9331754477779,-0.535609133856441,
3.84546567493331));
#46150=CARTESIAN_POINT('Ctrl Pts',(21.9570333658092,-0.396079448060293,
3.60772576847503));
#46151=CARTESIAN_POINT('Ctrl Pts',(21.9808912838407,-0.159697548225882,
3.46590759696012));
#46152=CARTESIAN_POINT('Ctrl Pts',(22.0047492018721,0.115734752223676,3.45468956637345));
#46153=CARTESIAN_POINT('Ctrl Pts',(22.0286071199035,0.362866753203085,3.5768147907664));
#46154=CARTESIAN_POINT('Ctrl Pts',(22.0524650379349,0.521267948732644,3.80242032615069));
#46155=CARTESIAN_POINT('Ctrl Pts',(22.0763229559664,0.552204931742854,4.07633947375325));
#46156=CARTESIAN_POINT('Ctrl Pts',(22.1001808739978,0.448112767182329,4.33159154057792));
#46157=CARTESIAN_POINT('Ctrl Pts',(22.1240387920292,0.23444482469764,4.5057604433585));
#46158=CARTESIAN_POINT('Ctrl Pts',(22.1478967100606,-0.0365512635718279,
4.55625714110116));
#46159=CARTESIAN_POINT('Ctrl Pts',(22.171754628092,-0.298609572266455,4.47073381570218));
#46160=CARTESIAN_POINT('Ctrl Pts',(22.1956125461234,-0.487649706571227,
4.2701032498363));
#46161=CARTESIAN_POINT('Ctrl Pts',(22.2194704641549,-0.557446204325542,
4.00342508191314));
#46162=CARTESIAN_POINT('Ctrl Pts',(22.2433283821863,-0.490931920559466,
3.73590938817905));
#46163=CARTESIAN_POINT('Ctrl Pts',(22.2671863002177,-0.304371409562025,
3.53297104269219));
#46164=CARTESIAN_POINT('Ctrl Pts',(22.2910442182491,-0.0433837978980346,
3.44423399893113));
#46165=CARTESIAN_POINT('Ctrl Pts',(22.3149021362806,0.228212333880327,3.49139688109763));
#46166=CARTESIAN_POINT('Ctrl Pts',(22.3387600543119,0.444004334066149,3.66292708008725));
#46167=CARTESIAN_POINT('Ctrl Pts',(22.3626179723434,0.551225179343846,3.91688078933633));
#46168=CARTESIAN_POINT('Ctrl Pts',(22.3864758903748,0.523656454698273,4.19115941035881));
#46169=CARTESIAN_POINT('Ctrl Pts',(22.4103338084062,0.368039459933637,4.41869434725418));
#46170=CARTESIAN_POINT('Ctrl Pts',(22.4341917264376,0.122426797365049,4.54384711353805));
#46171=CARTESIAN_POINT('Ctrl Pts',(22.458049644469,-0.153122562087755,4.53601444212637));
#46172=CARTESIAN_POINT('Ctrl Pts',(22.4819075625005,-0.391229265084309,
4.39711164706476));
#46173=CARTESIAN_POINT('Ctrl Pts',(22.5057654805319,-0.533669791868601,
4.16110422172694));
#46174=CARTESIAN_POINT('Ctrl Pts',(22.5296233985633,-0.545613449745194,
3.88570245498666));
#46175=CARTESIAN_POINT('Ctrl Pts',(22.5534813165947,-0.424139885198736,
3.63824949626794));
#46176=CARTESIAN_POINT('Ctrl Pts',(22.5773392346261,-0.198952323217499,
3.47925449370713));
#46177=CARTESIAN_POINT('Ctrl Pts',(22.6011971526576,0.0748840438856019,
3.44759575567767));
#46178=CARTESIAN_POINT('Ctrl Pts',(22.625055070689,0.330410085854462,3.55101527375816));
#46179=CARTESIAN_POINT('Ctrl Pts',(22.6489129887204,0.505140231362423,3.7642230866287));
#46180=CARTESIAN_POINT('Ctrl Pts',(22.6727709067518,0.556352908954721,4.03508610068096));
#46181=CARTESIAN_POINT('Ctrl Pts',(22.6966288247833,0.471516332128332,4.29736710820476));
#46182=CARTESIAN_POINT('Ctrl Pts',(22.7204867428146,0.27139215166714,4.48693847894857));
#46183=CARTESIAN_POINT('Ctrl Pts',(22.7443446608461,0.00488440565515616,
4.55743119390072));
#46184=CARTESIAN_POINT('Ctrl Pts',(22.7682025788775,-0.262778018495442,
4.49163382183027));
#46185=CARTESIAN_POINT('Ctrl Pts',(22.7920604969089,-0.466262514422727,
4.30558517247789));
#46186=CARTESIAN_POINT('Ctrl Pts',(22.8079657755965,-0.525793678117208,
4.1317859159904));
#46187=CARTESIAN_POINT('Ctrl Pts',(22.8159184149403,-0.532958495437544,
4.04301651477895));
#46188=CARTESIAN_POINT('Ctrl Pts',(3.98408158505965,-0.251304309929533,
3.59658905474035));
#46189=CARTESIAN_POINT('Ctrl Pts',(3.99203422440346,-0.184112308377066,
3.5547318870523));
#46190=CARTESIAN_POINT('Ctrl Pts',(4.00793950309107,-0.0284797076443847,
3.50528009766423));
#46191=CARTESIAN_POINT('Ctrl Pts',(4.03179742112249,0.212077873916637,3.55216010213054));
#46192=CARTESIAN_POINT('Ctrl Pts',(4.05565533915392,0.400711255741927,3.70851080938071));
#46193=CARTESIAN_POINT('Ctrl Pts',(4.07951325718533,0.49139298320592,3.93615790384083));
#46194=CARTESIAN_POINT('Ctrl Pts',(4.10337117521676,0.461898357851897,4.17940600742409));
#46195=CARTESIAN_POINT('Ctrl Pts',(4.12722909324816,0.319466186301668,4.37878980142624));
#46196=CARTESIAN_POINT('Ctrl Pts',(4.15108701127959,0.0989109688445654,
4.48554634140719));
#46197=CARTESIAN_POINT('Ctrl Pts',(4.174944929311,-0.145828100556353,4.47357507321567));
#46198=CARTESIAN_POINT('Ctrl Pts',(4.19880284734243,-0.354909590370033,
4.34580100620849));
#46199=CARTESIAN_POINT('Ctrl Pts',(4.22266076537384,-0.477205295803391,
4.13346959398438));
#46200=CARTESIAN_POINT('Ctrl Pts',(4.24651868340526,-0.482811689970624,
3.88850100783657));
#46201=CARTESIAN_POINT('Ctrl Pts',(4.27037660143669,-0.370357271909554,
3.67079708031066));
#46202=CARTESIAN_POINT('Ctrl Pts',(4.2942345194681,-0.167340519784032,3.53359217153378));
#46203=CARTESIAN_POINT('Ctrl Pts',(4.31809243749953,0.0765956044913427,
3.51043671457025));
#46204=CARTESIAN_POINT('Ctrl Pts',(4.34195035553093,0.301801986965541,3.60699279882218));
#46205=CARTESIAN_POINT('Ctrl Pts',(4.36580827356237,0.453209578636439,3.79964985833574));
#46206=CARTESIAN_POINT('Ctrl Pts',(4.38966619159377,0.493795074712635,4.04129798000377));
#46207=CARTESIAN_POINT('Ctrl Pts',(4.4135241096252,0.413634228782107,4.27284762322724));
#46208=CARTESIAN_POINT('Ctrl Pts',(4.43738202765661,0.23232854437776,4.43767858897425));
#46209=CARTESIAN_POINT('Ctrl Pts',(4.46123994568804,-0.00578779637616802,
4.49548521832112));
#46210=CARTESIAN_POINT('Ctrl Pts',(4.48509786371945,-0.242488863923451,
4.43213221465579));
#46211=CARTESIAN_POINT('Ctrl Pts',(4.50895578175088,-0.419894798625899,
4.26311111366653));
#46212=CARTESIAN_POINT('Ctrl Pts',(4.53281369978229,-0.494625017545811,
4.02975217827461));
#46213=CARTESIAN_POINT('Ctrl Pts',(4.55667161781372,-0.448405946262215,
3.78911802491887));
#46214=CARTESIAN_POINT('Ctrl Pts',(4.58052953584513,-0.292539406836986,
3.60005025874973));
#46215=CARTESIAN_POINT('Ctrl Pts',(4.60438745387655,-0.0651390137990107,
3.50878109874461));
#46216=CARTESIAN_POINT('Ctrl Pts',(4.62824537190797,0.178189642449287,3.53762834062211));
#46217=CARTESIAN_POINT('Ctrl Pts',(4.65210328993938,0.377946077338085,3.67953804797316));
#46218=CARTESIAN_POINT('Ctrl Pts',(4.67596120797081,0.485284401269169,3.89980943180067));
#46219=CARTESIAN_POINT('Ctrl Pts',(4.69981912600222,0.473957470210434,4.14458013869048));
#46220=CARTESIAN_POINT('Ctrl Pts',(4.72367704403364,0.34673502734182,4.35399706338589));
#46221=CARTESIAN_POINT('Ctrl Pts',(4.74753496206506,0.134726425416229,4.47685206339739));
#46222=CARTESIAN_POINT('Ctrl Pts',(4.77139288009648,-0.110226457398098,
4.48310374471865));
#46223=CARTESIAN_POINT('Ctrl Pts',(4.7952507981279,-0.328225968870003,4.37122340097448));
#46224=CARTESIAN_POINT('Ctrl Pts',(4.81910871615932,-0.465965290257402,
4.16856882376961));
#46225=CARTESIAN_POINT('Ctrl Pts',(4.84296663419074,-0.489763405537152,
3.92469457743051));
#46226=CARTESIAN_POINT('Ctrl Pts',(4.86682455222216,-0.393801027275785,
3.69923455818817));
#46227=CARTESIAN_POINT('Ctrl Pts',(4.89068247025357,-0.201543570920867,
3.54731988215497));
#46228=CARTESIAN_POINT('Ctrl Pts',(4.914540388285,0.039996778460842,3.50609782569371));
#46229=CARTESIAN_POINT('Ctrl Pts',(4.93839830631641,0.271756826018508,3.58564830447545));
#46230=CARTESIAN_POINT('Ctrl Pts',(4.96225622434784,0.437064927107334,3.76651905952651));
#46231=CARTESIAN_POINT('Ctrl Pts',(4.98611414237925,0.495498748108838,4.00448226441646));
#46232=CARTESIAN_POINT('Ctrl Pts',(5.00997206041068,0.432769628082826,4.24134943356216));
#46233=CARTESIAN_POINT('Ctrl Pts',(5.03382997844209,0.26421654558258,4.41920009197534));
#46234=CARTESIAN_POINT('Ctrl Pts',(5.05768789647352,0.031055320573195,4.49454490911931));
#46235=CARTESIAN_POINT('Ctrl Pts',(5.08154581450493,-0.209699776246285,
4.44896002485074));
#46236=CARTESIAN_POINT('Ctrl Pts',(5.10540373253635,-0.399177565666329,
4.29359218508065));
#46237=CARTESIAN_POINT('Ctrl Pts',(5.12926165056777,-0.491045566902382,
4.06643305876778));
#46238=CARTESIAN_POINT('Ctrl Pts',(5.15311956859918,-0.462839551218119,
3.823029239986));
#46239=CARTESIAN_POINT('Ctrl Pts',(5.17697748663061,-0.321456657764784,
3.62289959261435));
#46240=CARTESIAN_POINT('Ctrl Pts',(5.20083540466202,-0.101468855184408,
3.51498126685736));
#46241=CARTESIAN_POINT('Ctrl Pts',(5.22469332269345,0.143330846444675,3.52566323299877));
#46242=CARTESIAN_POINT('Ctrl Pts',(5.24855124072486,0.353082251864168,3.6523334593461));
#46243=CARTESIAN_POINT('Ctrl Pts',(5.27240915875629,0.476495428935435,3.86401762512973));
#46244=CARTESIAN_POINT('Ctrl Pts',(5.2962670767877,0.483392494157105,4.10895318565465));
#46245=CARTESIAN_POINT('Ctrl Pts',(5.32012499481913,0.372086927210194,4.32724672446184));
#46246=CARTESIAN_POINT('Ctrl Pts',(5.34398291285054,0.169795971115995,4.46551952511629));
#46247=CARTESIAN_POINT('Ctrl Pts',(5.36784083088196,-0.0740147250654609,
4.48996012138256));
#46248=CARTESIAN_POINT('Ctrl Pts',(5.39169874891337,-0.299726804847767,
4.39459212172504));
#46249=CARTESIAN_POINT('Ctrl Pts',(5.4155566669448,-0.452147516450583,4.20273559983216));
#46250=CARTESIAN_POINT('Ctrl Pts',(5.43941458497621,-0.494005844030112,
3.96130470137348));
#46251=CARTESIAN_POINT('Ctrl Pts',(5.46327250300764,-0.415066286295368,
3.72933585746768));
#46252=CARTESIAN_POINT('Ctrl Pts',(5.48713042103905,-0.234631715382576,
3.56355176915442));
#46253=CARTESIAN_POINT('Ctrl Pts',(5.51098833907048,0.00317670118048804,
3.50449116189365));
#46254=CARTESIAN_POINT('Ctrl Pts',(5.53484625710188,0.240208327774024,3.56659596294035));
#46255=CARTESIAN_POINT('Ctrl Pts',(5.55870417513332,0.418502475082003,3.73467985673571));
#46256=CARTESIAN_POINT('Ctrl Pts',(5.58256209316472,0.494461367456411,3.96764175273735));
#46257=CARTESIAN_POINT('Ctrl Pts',(5.60642001119615,0.449510986625754,4.20851612161082));
#46258=CARTESIAN_POINT('Ctrl Pts',(5.63027792922757,0.294642925140636,4.39840261889448));
#46259=CARTESIAN_POINT('Ctrl Pts',(5.65413584725899,0.0677266425295592,
4.49086882357174));
#46260=CARTESIAN_POINT('Ctrl Pts',(5.6779937652904,-0.17575064898472,4.46330422991997));
#46261=CARTESIAN_POINT('Ctrl Pts',(5.70185168332183,-0.376252119531055,
4.32244913183746));
#46262=CARTESIAN_POINT('Ctrl Pts',(5.72570960135325,-0.48474969783608,4.10274643779879));
#46263=CARTESIAN_POINT('Ctrl Pts',(5.74956751938466,-0.474712770918799,
3.85791944074229));
#46264=CARTESIAN_POINT('Ctrl Pts',(5.77342543741608,-0.348595640189148,
3.64783501103505));
#46265=CARTESIAN_POINT('Ctrl Pts',(5.7972833554475,-0.13723738064616,3.52386451312966));
#46266=CARTESIAN_POINT('Ctrl Pts',(5.82114127347893,0.1076791581852,3.5163221129105));
#46267=CARTESIAN_POINT('Ctrl Pts',(5.84499919151033,0.326265206982528,3.62705212841851));
#46268=CARTESIAN_POINT('Ctrl Pts',(5.86885710954176,0.465070530553655,3.82897806268729));
#46269=CARTESIAN_POINT('Ctrl Pts',(5.89271502757317,0.490153431381492,4.07272350923538));
#46270=CARTESIAN_POINT('Ctrl Pts',(5.9165729456046,0.395380485146506,4.29868609559117));
#46271=CARTESIAN_POINT('Ctrl Pts',(5.94043086363601,0.203926205561759,4.45161176009809));
#46272=CARTESIAN_POINT('Ctrl Pts',(5.96428878166744,-0.0373935204432717,
4.49410611450448));
#46273=CARTESIAN_POINT('Ctrl Pts',(5.98814669969885,-0.26956963613406,4.41577793841189));
#46274=CARTESIAN_POINT('Ctrl Pts',(6.01200461773027,-0.435828398698505,
4.23578096933615));
#46275=CARTESIAN_POINT('Ctrl Pts',(6.0358625357617,-0.495515688199628,3.99812868033461));
#46276=CARTESIAN_POINT('Ctrl Pts',(6.0597204537931,-0.434035059498629,3.76093483037113));
#46277=CARTESIAN_POINT('Ctrl Pts',(6.08357837182454,-0.266422612259865,
3.58219732064663));
#46278=CARTESIAN_POINT('Ctrl Pts',(6.10743628985594,-0.0336596025775484,
3.50562697870369));
#46279=CARTESIAN_POINT('Ctrl Pts',(6.13129420788738,0.207328476491996,3.54993858195554));
#46280=CARTESIAN_POINT('Ctrl Pts',(6.15515212591877,0.397629707835022,3.70431327123879));
#46281=CARTESIAN_POINT('Ctrl Pts',(6.17901004395022,0.490679606253205,3.93097100878581));
#46282=CARTESIAN_POINT('Ctrl Pts',(6.20286796198161,0.463782811036945,4.17454675550933));
#46283=CARTESIAN_POINT('Ctrl Pts',(6.22672588001306,0.323407044622774,4.3753682944706));
#46284=CARTESIAN_POINT('Ctrl Pts',(6.25058379804445,0.104084330837213,4.48453946106473));
#46285=CARTESIAN_POINT('Ctrl Pts',(6.27444171607588,-0.140944443623038,
4.4749681472433));
#46286=CARTESIAN_POINT('Ctrl Pts',(6.29829963410731,-0.351028389709017,
4.349743491311));
#46287=CARTESIAN_POINT('Ctrl Pts',(6.32215755213872,-0.476177279109797,
4.13807688197341));
#46288=CARTESIAN_POINT('Ctrl Pts',(6.34601547017014,-0.483231738207782,
3.89435343878414));
#46289=CARTESIAN_POINT('Ctrl Pts',(6.37782602754537,-0.338784024988664,
3.5998542259592));
#46290=CARTESIAN_POINT('Ctrl Pts',(6.41758922426439,0.0803770223010952,
3.44371490521648));
#46291=CARTESIAN_POINT('Ctrl Pts',(6.46530506032724,0.512014121509362,3.7673575683149));
#46292=CARTESIAN_POINT('Ctrl Pts',(6.51302089639006,0.472271980317209,4.30452828893312));
#46293=CARTESIAN_POINT('Ctrl Pts',(6.56073673245292,-0.000548856210248058,
4.56210751581942));
#46294=CARTESIAN_POINT('Ctrl Pts',(6.60845256851575,-0.473190198344468,
4.30346185287483));
#46295=CARTESIAN_POINT('Ctrl Pts',(6.65616840457859,-0.511122033036262,
3.76615996983968));
#46296=CARTESIAN_POINT('Ctrl Pts',(6.70388424064142,-0.0797735308749388,
3.44358772816382));
#46297=CARTESIAN_POINT('Ctrl Pts',(6.75160007670426,0.424880365184703,3.63198234005898));
#46298=CARTESIAN_POINT('Ctrl Pts',(6.7993159127671,0.539334593204737,4.15833063512042));
#46299=CARTESIAN_POINT('Ctrl Pts',(6.84703174882994,0.158523065679302,4.53928284691909));
#46300=CARTESIAN_POINT('Ctrl Pts',(6.89474758489278,-0.367869781963911,
4.42500259414721));
#46301=CARTESIAN_POINT('Ctrl Pts',(6.94246342095561,-0.556438361909488,
3.92043630538129));
#46302=CARTESIAN_POINT('Ctrl Pts',(6.99017925701846,-0.234023037562683,
3.48893437735136));
#46303=CARTESIAN_POINT('Ctrl Pts',(7.03789509308128,0.303300305128555,3.52675198254107));
#46304=CARTESIAN_POINT('Ctrl Pts',(7.08561092914413,0.562097748282813,3.99916046672433));
#46305=CARTESIAN_POINT('Ctrl Pts',(7.13332676520696,0.304712478085684,4.47233993757656));
#46306=CARTESIAN_POINT('Ctrl Pts',(7.18104260126981,-0.232495107101315,
4.51176235979777));
#46307=CARTESIAN_POINT('Ctrl Pts',(7.22875843733264,-0.556198774489988,
4.08122554105153));
#46308=CARTESIAN_POINT('Ctrl Pts',(7.27647427339549,-0.369136593294786,
3.57609805363465));
#46309=CARTESIAN_POINT('Ctrl Pts',(7.32419010945832,0.156909424853758,3.46024624852207));
#46310=CARTESIAN_POINT('Ctrl Pts',(7.37190594552116,0.538863091386428,3.84005861730642));
#46311=CARTESIAN_POINT('Ctrl Pts',(7.41962178158399,0.425970496197337,4.36674761950234));
#46312=CARTESIAN_POINT('Ctrl Pts',(7.46733761764684,-0.0780973635293338,
4.55664663921719));
#46313=CARTESIAN_POINT('Ctrl Pts',(7.51505345370967,-0.510447210801067,
4.2353684852172));
#46314=CARTESIAN_POINT('Ctrl Pts',(7.56276928977251,-0.474045531130633,
3.69794782953315));
#46315=CARTESIAN_POINT('Ctrl Pts',(7.61048512583535,-0.00232054557778912,
3.43790632971152));
#46316=CARTESIAN_POINT('Ctrl Pts',(7.65820096189818,0.471535432411473,3.69404409621074));
#46317=CARTESIAN_POINT('Ctrl Pts',(7.70591679796103,0.512373167457076,4.23114587691112));
#46318=CARTESIAN_POINT('Ctrl Pts',(7.75363263402387,0.0826907388754792,
4.55598284219971));
#46319=CARTESIAN_POINT('Ctrl Pts',(7.80134847008669,-0.422927867535356,
4.3702522086048));
#46320=CARTESIAN_POINT('Ctrl Pts',(7.84906430614955,-0.540165305628305,
3.84451327478339));
#46321=CARTESIAN_POINT('Ctrl Pts',(7.89678014221237,-0.161360632039799,
3.46156019320034));
#46322=CARTESIAN_POINT('Ctrl Pts',(7.94449597827521,0.365623992797271,3.57306467116217));
#46323=CARTESIAN_POINT('Ctrl Pts',(7.99221181433806,0.556850479203549,4.07663043084052));
#46324=CARTESIAN_POINT('Ctrl Pts',(8.03992765040089,0.236712602309549,4.50982528676712));
#46325=CARTESIAN_POINT('Ctrl Pts',(8.08764348646373,-0.300802099575971,
4.47483973718518));
#46326=CARTESIAN_POINT('Ctrl Pts',(8.13535932252656,-0.562085604986122,
4.00380155059756));
#46327=CARTESIAN_POINT('Ctrl Pts',(8.18307515858941,-0.307197250538534,
3.52927234160183));
#46328=CARTESIAN_POINT('Ctrl Pts',(8.23079099465223,0.229795065915734,3.48701958438918));
#46329=CARTESIAN_POINT('Ctrl Pts',(8.27850683071509,0.555763037488074,3.91584463605021));
#46330=CARTESIAN_POINT('Ctrl Pts',(8.32622266677791,0.371365260221553,4.42195085332305));
#46331=CARTESIAN_POINT('Ctrl Pts',(8.37393850284076,-0.154062949695418,
4.54057310944092));
#46332=CARTESIAN_POINT('Ctrl Pts',(8.4216543389036,-0.538012782343907,4.16277876137275));
#46333=CARTESIAN_POINT('Ctrl Pts',(8.46937017496643,-0.427897198575242,
3.6355021720628));
#46334=CARTESIAN_POINT('Ctrl Pts',(8.51708601102927,0.0751629666897603,
3.44294954666756));
#46335=CARTESIAN_POINT('Ctrl Pts',(8.56480184709211,0.50919982311266,3.76194492389047));
#46336=CARTESIAN_POINT('Ctrl Pts',(8.61251768315494,0.475630646924824,4.29954994045293));
#46337=CARTESIAN_POINT('Ctrl Pts',(8.66023351921779,0.00528252914771292,
4.56207363752918));
#46338=CARTESIAN_POINT('Ctrl Pts',(8.70794935528062,-0.469916616427902,
4.30843646464781));
#46339=CARTESIAN_POINT('Ctrl Pts',(8.75566519134346,-0.513584102541225,
3.7715573403753));
#46340=CARTESIAN_POINT('Ctrl Pts',(8.8033810274063,-0.0856194047837525,
3.44446062547832));
#46341=CARTESIAN_POINT('Ctrl Pts',(8.85109686346913,0.420970909810523,3.6275242662766));
#46342=CARTESIAN_POINT('Ctrl Pts',(8.89881269953199,0.540977160455745,4.15263810462895));
#46343=CARTESIAN_POINT('Ctrl Pts',(8.9465285355948,0.1641957606509,4.5375820228614));
#46344=CARTESIAN_POINT('Ctrl Pts',(8.99424437165766,-0.363369132636193,
4.42885609773758));
#46345=CARTESIAN_POINT('Ctrl Pts',(9.04196020772048,-0.557246560270691,
3.92630501926208));
#46346=CARTESIAN_POINT('Ctrl Pts',(9.08967604378333,-0.239395897268157,
3.49142917554125));
#46347=CARTESIAN_POINT('Ctrl Pts',(9.13739187984617,0.298295701775085,3.52358174528888));
#46348=CARTESIAN_POINT('Ctrl Pts',(9.18510771590899,0.562057768008922,3.99323652897485));
#46349=CARTESIAN_POINT('Ctrl Pts',(9.23282355197185,0.309673537509763,4.46910231217259));
#46350=CARTESIAN_POINT('Ctrl Pts',(9.28053938803466,-0.227088667424462,
4.51418422403538));
#46351=CARTESIAN_POINT('Ctrl Pts',(9.32825522409753,-0.555311854854516,
4.08708285122523));
#46352=CARTESIAN_POINT('Ctrl Pts',(9.37597106016035,-0.373583621400482,
3.58001195619306));
#46353=CARTESIAN_POINT('Ctrl Pts',(9.4236868962232,0.151212199908504,3.45862254413551));
#46354=CARTESIAN_POINT('Ctrl Pts',(9.47140273228603,0.537147531342748,3.83438837996121));
#46355=CARTESIAN_POINT('Ctrl Pts',(9.51911856834887,0.429812019667804,4.36223791473086));
#46356=CARTESIAN_POINT('Ctrl Pts',(9.5668344044117,-0.0722264831760907,
4.5574387986564));
#46357=CARTESIAN_POINT('Ctrl Pts',(9.61455024047456,-0.507938295172089,
4.24073505647735));
#46358=CARTESIAN_POINT('Ctrl Pts',(9.66226607653738,-0.477202555076283,
3.70296060775017));
#46359=CARTESIAN_POINT('Ctrl Pts',(9.70998191260023,-0.00824436594879979,
3.43796200346455));
#46360=CARTESIAN_POINT('Ctrl Pts',(9.75769774866306,0.46828475128534,3.68909153946361));
#46361=CARTESIAN_POINT('Ctrl Pts',(9.80541358472589,0.514780775927077,4.22573309871483));
#46362=CARTESIAN_POINT('Ctrl Pts',(9.85312942078874,0.0885456931146035,
4.55508048006603));
#46363=CARTESIAN_POINT('Ctrl Pts',(9.90084525685159,-0.419002262135622,
4.37468891556157));
#46364=CARTESIAN_POINT('Ctrl Pts',(9.9485610929144,-0.541773992888202,3.8502147545669));
#46365=CARTESIAN_POINT('Ctrl Pts',(9.99627692897727,-0.167026329707142,
3.46329068919569));
#46366=CARTESIAN_POINT('Ctrl Pts',(10.0439927650401,0.361104182074418,3.56923504227033));
#46367=CARTESIAN_POINT('Ctrl Pts',(10.0917086011029,0.557627167155001,4.07075748419897));
#46368=CARTESIAN_POINT('Ctrl Pts',(10.1394244371657,0.242072544440304,4.50730223964386));
#46369=CARTESIAN_POINT('Ctrl Pts',(10.1871402732286,-0.295781020598791,
4.47798354257549));
#46370=CARTESIAN_POINT('Ctrl Pts',(10.2348561092914,-0.56201432324602,4.00972520363789));
#46371=CARTESIAN_POINT('Ctrl Pts',(10.2825719453543,-0.312141225154507,
3.53253606055812));
#46372=CARTESIAN_POINT('Ctrl Pts',(10.3302877814171,0.224375962906492,3.48462624592509));
#46373=CARTESIAN_POINT('Ctrl Pts',(10.37800361748,0.554845251762499,3.90999207970357));
#46374=CARTESIAN_POINT('Ctrl Pts',(10.4257194535428,0.375791608533427,4.41801357164013));
#46375=CARTESIAN_POINT('Ctrl Pts',(10.4734352896056,-0.148357251109035,
4.54216676877402));
#46376=CARTESIAN_POINT('Ctrl Pts',(10.5211511256685,-0.536267364288337,
4.16843987983467));
#46377=CARTESIAN_POINT('Ctrl Pts',(10.5688669617313,-0.431714905307627,
3.64003205746247));
#46378=CARTESIAN_POINT('Ctrl Pts',(10.6165827977942,0.0692879940047382,
3.44218833554121));
#46379=CARTESIAN_POINT('Ctrl Pts',(10.664298633857,0.50666266228973,3.75659164812817));
#46380=CARTESIAN_POINT('Ctrl Pts',(10.7120144699198,0.478761211786921,4.29452059555793));
#46381=CARTESIAN_POINT('Ctrl Pts',(10.7597303059827,0.0112059738120427,
4.56198674830498));
#46382=CARTESIAN_POINT('Ctrl Pts',(10.8074461420455,-0.466639882340508,
4.31337182280594));
#46383=CARTESIAN_POINT('Ctrl Pts',(10.8551619781083,-0.515963154362253,
3.77698273057893));
#46384=CARTESIAN_POINT('Ctrl Pts',(10.9028778141712,-0.0914695226195351,
3.44539382842306));
#46385=CARTESIAN_POINT('Ctrl Pts',(10.950593650234,0.417021979184216,3.62310830733915));
#46386=CARTESIAN_POINT('Ctrl Pts',(10.9983094862969,0.542555780795161,4.14692822684982));
#46387=CARTESIAN_POINT('Ctrl Pts',(11.0460253223597,0.169852260608159,4.53582169486292));
#46388=CARTESIAN_POINT('Ctrl Pts',(11.0937411584225,-0.358829204008283,
4.43266185580689));
#46389=CARTESIAN_POINT('Ctrl Pts',(11.1414569944853,-0.55799228928692,3.93218197720501));
#46390=CARTESIAN_POINT('Ctrl Pts',(11.1891728305482,-0.244742469498405,
3.49398043245019));
#46391=CARTESIAN_POINT('Ctrl Pts',(11.236888666611,0.293258125877444,3.5204644426882));
#46392=CARTESIAN_POINT('Ctrl Pts',(11.2846045026739,0.561955271903759,3.98731333380864));
#46393=CARTESIAN_POINT('Ctrl Pts',(11.3323203387367,0.314600244947554,4.46581258570203));
#46394=CARTESIAN_POINT('Ctrl Pts',(11.3800361747996,-0.221657027690976,
4.51654897269734));
#46395=CARTESIAN_POINT('Ctrl Pts',(11.4277520108624,-0.554363241169119,
4.0929304899371));
#46396=CARTESIAN_POINT('Ctrl Pts',(11.4754678469252,-0.377989160306769,
3.58397250834823));
#46397=CARTESIAN_POINT('Ctrl Pts',(11.5231836829881,0.145498182576105,3.45705897374896));
#46398=CARTESIAN_POINT('Ctrl Pts',(11.5708995190509,0.535372305622036,3.82873653777755));
#46399=CARTESIAN_POINT('Ctrl Pts',(11.6186153551137,0.43360580265347,4.35768797439208));
#46400=CARTESIAN_POINT('Ctrl Pts',(11.6663311911766,-0.0663475807746441,
4.55816904038548));
#46401=CARTESIAN_POINT('Ctrl Pts',(11.7140470272394,-0.505372959888646,
4.24607488805821));
#46402=CARTESIAN_POINT('Ctrl Pts',(11.7617628633023,-0.480306573774387,
3.70800637967828));
#46403=CARTESIAN_POINT('Ctrl Pts',(11.8094786993651,-0.0141672704965164,
3.43808010573911));
#46404=CARTESIAN_POINT('Ctrl Pts',(11.8571945354279,0.464982055269784,3.68417351694868));
#46405=CARTESIAN_POINT('Ctrl Pts',(11.9049103714908,0.517131205013274,4.22029524715934));
#46406=CARTESIAN_POINT('Ctrl Pts',(11.9526262075536,0.0943908121067024,
4.55411646222552));
#46407=CARTESIAN_POINT('Ctrl Pts',(12.0003420436165,-0.415030115946784,
4.37908400385228));
#46408=CARTESIAN_POINT('Ctrl Pts',(12.0480578796793,-0.543322502467158,
3.85593287178435));
#46409=CARTESIAN_POINT('Ctrl Pts',(12.0957737157421,-0.172673474880652,
3.46508080031456));
#46410=CARTESIAN_POINT('Ctrl Pts',(12.143489551805,0.356544261611682,3.56545326070575));
#46411=CARTESIAN_POINT('Ctrl Pts',(12.1912053878678,0.558341916527368,4.06487667815191));
#46412=CARTESIAN_POINT('Ctrl Pts',(12.2389212239306,0.247405598301292,4.50472284379514));
#46413=CARTESIAN_POINT('Ctrl Pts',(12.2866370599935,-0.290727087669313,
4.48107425582212));
#46414=CARTESIAN_POINT('Ctrl Pts',(12.3343528960563,-0.56188061562194,4.01564777644873));
#46415=CARTESIAN_POINT('Ctrl Pts',(12.3820687321191,-0.317050528604376,
3.5358517031905));
#46416=CARTESIAN_POINT('Ctrl Pts',(12.429784568182,0.218931937280033,3.48229015273196));
#46417=CARTESIAN_POINT('Ctrl Pts',(12.4775004042448,0.553865836459325,3.90414952100961));
#46418=CARTESIAN_POINT('Ctrl Pts',(12.5252162403077,0.380176215696692,4.4140298589933));
#46419=CARTESIAN_POINT('Ctrl Pts',(12.5729320763705,-0.142635073703209,
4.54370020679522));
#46420=CARTESIAN_POINT('Ctrl Pts',(12.6206479124333,-0.53446238019874,4.17408228879405));
#46421=CARTESIAN_POINT('Ctrl Pts',(12.6683637484962,-0.435484659196984,
3.644601926393));
#46422=CARTESIAN_POINT('Ctrl Pts',(12.716079584559,0.0634053251381518,3.44148908348752));
#46423=CARTESIAN_POINT('Ctrl Pts',(12.7637954206219,0.504069223782589,3.75126540901054));
#46424=CARTESIAN_POINT('Ctrl Pts',(12.8115112566847,0.481838598125516,4.2894585367128));
#46425=CARTESIAN_POINT('Ctrl Pts',(12.8592270927475,0.0171281737699642,
4.56183743625962));
#46426=CARTESIAN_POINT('Ctrl Pts',(12.9069429288104,-0.463311316109371,
4.31827237310907));
#46427=CARTESIAN_POINT('Ctrl Pts',(12.9546587648732,-0.518284895444539,
3.78243289248252));
#46428=CARTESIAN_POINT('Ctrl Pts',(13.0023746009361,-0.0973094804548018,
3.44638863438952));
#46429=CARTESIAN_POINT('Ctrl Pts',(13.0500904369989,0.413026727735397,3.61873421174243));
#46430=CARTESIAN_POINT('Ctrl Pts',(13.0978062730617,0.544074136613086,4.14120202898048));
#46431=CARTESIAN_POINT('Ctrl Pts',(13.1455221091246,0.17548989418231,4.53400185033327));
#46432=CARTESIAN_POINT('Ctrl Pts',(13.1932379451874,-0.354249418335187,
4.4364195558504));
#46433=CARTESIAN_POINT('Ctrl Pts',(13.2409537812502,-0.558676039167545,
3.93806646805208));
#46434=CARTESIAN_POINT('Ctrl Pts',(13.2886696173131,-0.250061856896528,
3.49658789561142));
#46435=CARTESIAN_POINT('Ctrl Pts',(13.3363854533759,0.288187976258808,3.51740040462167));
#46436=CARTESIAN_POINT('Ctrl Pts',(13.3841012894388,0.56179035647369,3.9813915478171));
#46437=CARTESIAN_POINT('Ctrl Pts',(13.4318171255016,0.319492008083037,4.46247111897993));
#46438=CARTESIAN_POINT('Ctrl Pts',(13.4795329615644,-0.21620076734671,4.51885634555065));
#46439=CARTESIAN_POINT('Ctrl Pts',(13.5272487976273,-0.553353051445561,
4.09876780637113));
#46440=CARTESIAN_POINT('Ctrl Pts',(13.5749646336901,-0.382352713970831,
3.58797927086295));
#46441=CARTESIAN_POINT('Ctrl Pts',(13.6226804697529,0.139768003996038,3.45555571067516));
#46442=CARTESIAN_POINT('Ctrl Pts',(13.6703963058158,0.53353761328617,3.82310371872654));
#46443=CARTESIAN_POINT('Ctrl Pts',(13.7181121418786,0.437351422764197,4.35309830377052));
#46444=CARTESIAN_POINT('Ctrl Pts',(13.7658279779415,-0.0604613087987784,
4.55883728334624));
#46445=CARTESIAN_POINT('Ctrl Pts',(13.8135438140043,-0.502751490175015,
4.25138738680826));
#46446=CARTESIAN_POINT('Ctrl Pts',(13.8612596500671,-0.483357242297515,
3.71308458487209));
#46447=CARTESIAN_POINT('Ctrl Pts',(13.90897548613,-0.0200886014110514,3.43826062340902));
#46448=CARTESIAN_POINT('Ctrl Pts',(13.9566913221928,0.461627711254046,3.67929057494076));
#46449=CARTESIAN_POINT('Ctrl Pts',(14.0044071582557,0.519424193619207,4.21483292625321));
#46450=CARTESIAN_POINT('Ctrl Pts',(14.0521229943185,0.100225446615308,4.55309089575788));
#46451=CARTESIAN_POINT('Ctrl Pts',(14.0998388303813,-0.411011870182152,
4.38343698529073));
#46452=CARTESIAN_POINT('Ctrl Pts',(14.1475546664441,-0.544810662360815,
3.86166699129474));
#46453=CARTESIAN_POINT('Ctrl Pts',(14.195270502507,-0.178301440303968,3.46693032771971));
#46454=CARTESIAN_POINT('Ctrl Pts',(14.2429863385698,0.351944737904315,3.5617197465309));
#46455=CARTESIAN_POINT('Ctrl Pts',(14.2907021746327,0.558994647929194,4.05898866591129));
#46456=CARTESIAN_POINT('Ctrl Pts',(14.3384180106955,0.252711171522458,4.50208738572805));
#46457=CARTESIAN_POINT('Ctrl Pts',(14.3861338467583,-0.28564086215454,4.48411153362329));
#46458=CARTESIAN_POINT('Ctrl Pts',(14.4338496828212,-0.561684496965419,
4.02156861117883));
#46459=CARTESIAN_POINT('Ctrl Pts',(14.481565518884,-0.321924615586062,3.53921890121312));
#46460=CARTESIAN_POINT('Ctrl Pts',(14.5292813549469,0.213463593732893,3.48001156429194));
#46461=CARTESIAN_POINT('Ctrl Pts',(14.5769971910097,0.552824900367352,3.89831760893199));
#46462=CARTESIAN_POINT('Ctrl Pts',(14.6247130270725,0.384518594689996,4.4100001578745));
#46463=CARTESIAN_POINT('Ctrl Pts',(14.6724288631354,-0.136897053070264,
4.54517325317752));
#46464=CARTESIAN_POINT('Ctrl Pts',(14.7201446991982,-0.532598030564186,
4.17970536151887));
#46465=CARTESIAN_POINT('Ctrl Pts',(14.7678605352611,-0.439206041516937,
3.64921127125505));
#46466=CARTESIAN_POINT('Ctrl Pts',(14.8155763713239,0.0575156135089261,
3.44085186817608));
#46467=CARTESIAN_POINT('Ctrl Pts',(14.8632922073868,0.501419795658073,3.74596679815093));
#46468=CARTESIAN_POINT('Ctrl Pts',(14.9110080434496,0.484862464119148,4.284364326187));
#46469=CARTESIAN_POINT('Ctrl Pts',(14.9587238795124,0.0230484712116303,
4.56162571797798));
#46470=CARTESIAN_POINT('Ctrl Pts',(15.0064397155752,-0.459931287455839,
4.32313757122732));
#46471=CARTESIAN_POINT('Ctrl Pts',(15.0541555516381,-0.5205490679001,3.78790722070797));
#46472=CARTESIAN_POINT('Ctrl Pts',(15.1018713877009,-0.103138629614742,
3.44744493287938));
#46473=CARTESIAN_POINT('Ctrl Pts',(15.1495872237638,0.40898559923764,3.61440246534021));
#46474=CARTESIAN_POINT('Ctrl Pts',(15.1973030598266,0.545532059257757,4.13546014705983));
#46475=CARTESIAN_POINT('Ctrl Pts',(15.2450188958894,0.181108035171788,4.53212269141213));
#46476=CARTESIAN_POINT('Ctrl Pts',(15.2927347319523,-0.349630284317748,
4.44012878048063));
#46477=CARTESIAN_POINT('Ctrl Pts',(15.3404505680151,-0.559297733964875,
3.94395783818199));
#46478=CARTESIAN_POINT('Ctrl Pts',(15.3881664040779,-0.255353468610234,
3.49925127540033));
#46479=CARTESIAN_POINT('Ctrl Pts',(15.4358822401408,0.283085816087337,3.51438997142805));
#46480=CARTESIAN_POINT('Ctrl Pts',(15.4835980762036,0.561563040036739,3.97547182876414));
#46481=CARTESIAN_POINT('Ctrl Pts',(15.5313139122665,0.324348283562367,4.45907828316053));
#46482=CARTESIAN_POINT('Ctrl Pts',(15.5790297483293,-0.210720492447169,
4.52110608630326));
#46483=CARTESIAN_POINT('Ctrl Pts',(15.6267455843921,-0.552281397890927,
4.10459415214592));
#46484=CARTESIAN_POINT('Ctrl Pts',(15.674461420455,-0.386673797709831,3.59203179868507));
#46485=CARTESIAN_POINT('Ctrl Pts',(15.7221772565178,0.134022300649356,3.45411292188939));
#46486=CARTESIAN_POINT('Ctrl Pts',(15.7698930925807,0.531643658124066,3.81749054847505));
#46487=CARTESIAN_POINT('Ctrl Pts',(15.8176089286435,0.441048463954279,4.34846941266494));
#46488=CARTESIAN_POINT('Ctrl Pts',(15.8653247647064,-0.054568321067637,
4.5594434533135));
#46489=CARTESIAN_POINT('Ctrl Pts',(15.9130406007692,-0.500074177211609,
4.25667196264028));
#46490=CARTESIAN_POINT('Ctrl Pts',(15.960756436832,-0.486354221791887,3.71819465926869));
#46491=CARTESIAN_POINT('Ctrl Pts',(16.0084722728949,-0.0260077009790528,
3.4385035364232));
#46492=CARTESIAN_POINT('Ctrl Pts',(16.0561881089577,0.458222091822753,3.6744432558139));
#46493=CARTESIAN_POINT('Ctrl Pts',(16.1039039450206,0.52165948705058,4.2093467427251));
#46494=CARTESIAN_POINT('Ctrl Pts',(16.1516197810833,0.106048948556897,4.55200389457816));
#46495=CARTESIAN_POINT('Ctrl Pts',(16.1993356171462,-0.406947971169398,
4.38774737636841));
#46496=CARTESIAN_POINT('Ctrl Pts',(16.247051453209,-0.546238307271431,3.86741647617928));
#46497=CARTESIAN_POINT('Ctrl Pts',(16.2947672892719,-0.183909600849411,
3.46883906597446));
#46498=CARTESIAN_POINT('Ctrl Pts',(16.3424831253347,0.347306121845567,3.55803491444678));
#46499=CARTESIAN_POINT('Ctrl Pts',(16.3901989613975,0.559585288858183,4.05309410148958));
#46500=CARTESIAN_POINT('Ctrl Pts',(16.4379147974604,0.257988674785898,4.49939615817675));
#46501=CARTESIAN_POINT('Ctrl Pts',(16.4856306335232,-0.280522909008289,
4.4870950386126));
#46502=CARTESIAN_POINT('Ctrl Pts',(16.5333464695861,-0.561425989060384,
4.02748705016995));
#46503=CARTESIAN_POINT('Ctrl Pts',(16.5810623056489,-0.326762944709103,
3.54263728061361));
#46504=CARTESIAN_POINT('Ctrl Pts',(16.6287781417117,0.207971539662738,3.4777907336998));
#46505=CARTESIAN_POINT('Ctrl Pts',(16.6764939777746,0.551722559108811,3.89249699125187));
#46506=CARTESIAN_POINT('Ctrl Pts',(16.7242098138374,0.388818263182495,4.40592491588375));
#46507=CARTESIAN_POINT('Ctrl Pts',(16.7719256499003,-0.131143826562283,
4.54658574430191));
#46508=CARTESIAN_POINT('Ctrl Pts',(16.8196414859631,-0.53067452246778,4.18530847342493));
#46509=CARTESIAN_POINT('Ctrl Pts',(16.8673573220259,-0.442878638914007,
3.65385958006445));
#46510=CARTESIAN_POINT('Ctrl Pts',(16.9150731580888,0.0516195133182915,
3.44027676038576));
#46511=CARTESIAN_POINT('Ctrl Pts',(16.9627889941516,0.498714672202087,3.74069640409388));
#46512=CARTESIAN_POINT('Ctrl Pts',(17.0105048302145,0.487832473891125,4.27923852982128));
#46513=CARTESIAN_POINT('Ctrl Pts',(17.0582206662773,0.0289662085384809,
4.56135161697672));
#46514=CARTESIAN_POINT('Ctrl Pts',(17.1059365023401,-0.456500171817451,
4.32796687675757));
#46515=CARTESIAN_POINT('Ctrl Pts',(17.1536523384029,-0.522755420235406,
3.79340510719289));
#46516=CARTESIAN_POINT('Ctrl Pts',(17.2013681744658,-0.108956322625149,
3.44856260656401));
#46517=CARTESIAN_POINT('Ctrl Pts',(17.2490840105286,0.404899042560309,3.61011354928233));
#46518=CARTESIAN_POINT('Ctrl Pts',(17.2967998465915,0.54692938679005,4.12970321886885));
#46519=CARTESIAN_POINT('Ctrl Pts',(17.3445156826543,0.186706059540143,4.53018442682757));
#46520=CARTESIAN_POINT('Ctrl Pts',(17.3922315187172,-0.344972315027459,
4.4437891176945));
#46521=CARTESIAN_POINT('Ctrl Pts',(17.43994735478,-0.559857304624004,3.94985543320929));
#46522=CARTESIAN_POINT('Ctrl Pts',(17.4876631908428,-0.260616716872392,
3.5019702759813));
#46523=CARTESIAN_POINT('Ctrl Pts',(17.5353790269057,0.277952212086773,3.51143347749201));
#46524=CARTESIAN_POINT('Ctrl Pts',(17.5830948629685,0.561273347842132,3.96955483418404));
#46525=CARTESIAN_POINT('Ctrl Pts',(17.6308106990313,0.329168531973526,4.45563445510394));
#46526=CARTESIAN_POINT('Ctrl Pts',(17.6785265350942,-0.205216811715269,
4.52329794506467));
#46527=CARTESIAN_POINT('Ctrl Pts',(17.726242371157,-0.551148399539408,4.11040888009862));
#46528=CARTESIAN_POINT('Ctrl Pts',(17.7739582072198,-0.390951931558304,
3.59612964167903));
#46529=CARTESIAN_POINT('Ctrl Pts',(17.8216740432827,0.128261710741471,3.45273076764982));
#46530=CARTESIAN_POINT('Ctrl Pts',(17.8693898793456,0.529690650507269,3.81189765050732));
#46531=CARTESIAN_POINT('Ctrl Pts',(17.9171057154083,0.44469651557395,4.34380181523062));
#46532=CARTESIAN_POINT('Ctrl Pts',(17.9648215514712,-0.0486692721463468,
4.55998748295674));
#46533=CARTESIAN_POINT('Ctrl Pts',(18.012537387534,-0.497341318381634,4.26192802856871));
#46534=CARTESIAN_POINT('Ctrl Pts',(18.0602532235969,-0.489297179367249,
3.72333603526529));
#46535=CARTESIAN_POINT('Ctrl Pts',(18.1079690596597,-0.0319239117350811,
3.43880881780002));
#46536=CARTESIAN_POINT('Ctrl Pts',(18.1556848957225,0.454765575255941,3.66963209798526));
#46537=CARTESIAN_POINT('Ctrl Pts',(18.2034007317854,0.523836837021606,4.20383730595423));
#46538=CARTESIAN_POINT('Ctrl Pts',(18.2511165678483,0.111860671084556,4.5508555794253));
#46539=CARTESIAN_POINT('Ctrl Pts',(18.298832403911,-0.402838870307115,4.39201469830757));
#46540=CARTESIAN_POINT('Ctrl Pts',(18.346548239974,-0.547605278623001,3.87318068781251));
#46541=CARTESIAN_POINT('Ctrl Pts',(18.3942640760367,-0.189497333589109,
3.47080680306518));
#46542=CARTESIAN_POINT('Ctrl Pts',(18.4419799120997,0.342628928670919,3.55439917374707));
#46543=CARTESIAN_POINT('Ctrl Pts',(18.4896957481624,0.560113773708727,4.04719363962704));
#46544=CARTESIAN_POINT('Ctrl Pts',(18.5374115842253,0.263237521891608,4.49664946007004));
#46545=CARTESIAN_POINT('Ctrl Pts',(18.5851274202881,-0.275373796708506,
4.49002443939646));
#46546=CARTESIAN_POINT('Ctrl Pts',(18.632843256351,-0.561105120620647,4.03340243603));
#46547=CARTESIAN_POINT('Ctrl Pts',(18.6805590924138,-0.331564978554912,
3.54610646169455));
#46548=CARTESIAN_POINT('Ctrl Pts',(18.7282749284766,0.202456385100939,3.47562790763498));
#46549=CARTESIAN_POINT('Ctrl Pts',(18.7759907645394,0.550558935126376,3.8866883144956));
#46550=CARTESIAN_POINT('Ctrl Pts',(18.8237066006023,0.393074743587739,4.40180458567998));
#46551=CARTESIAN_POINT('Ctrl Pts',(18.8714224366651,-0.125376033221007,
4.54793752327491));
#46552=CARTESIAN_POINT('Ctrl Pts',(18.919138272728,-0.528692069562509,4.19089100214638));
#46553=CARTESIAN_POINT('Ctrl Pts',(18.9668541087908,-0.4465020434557,3.6585463365067));
#46554=CARTESIAN_POINT('Ctrl Pts',(19.0145699448537,0.0457176794812401,
3.43976382400136));
#46555=CARTESIAN_POINT('Ctrl Pts',(19.0622857809165,0.495954153879041,3.73545481224116));
#46556=CARTESIAN_POINT('Ctrl Pts',(19.1100016169793,0.490748297561716,4.27408171698104));
#46557=CARTESIAN_POINT('Ctrl Pts',(19.1577174530421,0.0348807284082936,
4.5610151636709));
#46558=CARTESIAN_POINT('Ctrl Pts',(19.205433289105,-0.453018350253257,4.33275975334162));
#46559=CARTESIAN_POINT('Ctrl Pts',(19.2531491251678,-0.524903707479367,
3.79892594114836));
#46560=CARTESIAN_POINT('Ctrl Pts',(19.3008649612307,-0.11476191309534,3.44974153150476));
#46561=CARTESIAN_POINT('Ctrl Pts',(19.3485807972935,0.400767511262006,3.60586793956989));
#46562=CARTESIAN_POINT('Ctrl Pts',(19.3962966333564,0.548265964675035,4.12393188459875));
#46563=CARTESIAN_POINT('Ctrl Pts',(19.4440124694192,0.192283344213529,4.52818727047755));
#46564=CARTESIAN_POINT('Ctrl Pts',(19.491728305482,-0.340276025447905,4.44740016355363));
#46565=CARTESIAN_POINT('Ctrl Pts',(19.5394441415448,-0.560354693525076,
3.95575859308266));
#46566=CARTESIAN_POINT('Ctrl Pts',(19.5871599776077,-0.265851008504119,
3.50474460473346));
#46567=CARTESIAN_POINT('Ctrl Pts',(19.6348758136705,0.272787718306182,3.5085312334714));
#46568=CARTESIAN_POINT('Ctrl Pts',(19.6825916497334,0.560921342594646,3.96364125479661));
#46569=CARTESIAN_POINT('Ctrl Pts',(19.7303074857962,0.33395216026474,4.45213995410186));
#46570=CARTESIAN_POINT('Ctrl Pts',(19.7780233218591,-0.199690227635008,
4.52543179776919));
#46571=CARTESIAN_POINT('Ctrl Pts',(19.8257391579219,-0.549954387748789,
4.11621111891367));
#46572=CARTESIAN_POINT('Ctrl Pts',(19.8734549939848,-0.395186252277308,
3.60027277035845));
#46573=CARTESIAN_POINT('Ctrl Pts',(19.9211708300475,0.122486141425193,3.45140859770427));
#46574=CARTESIAN_POINT('Ctrl Pts',(19.9688866661104,0.527680190865048,3.80632716374734));
#46575=CARTESIAN_POINT('Ctrl Pts',(20.0166025021732,0.448292560087992,4.33909316421112));
#46576=CARTESIAN_POINT('Ctrl Pts',(20.0643183382361,-0.0427598846646947,
4.56047472290141));
#46577=CARTESIAN_POINT('Ctrl Pts',(20.1120341742989,-0.49456253103916,4.26714478353561));
#46578=CARTESIAN_POINT('Ctrl Pts',(20.1597500103618,-0.492168201513856,
3.72852743457374));
#46579=CARTESIAN_POINT('Ctrl Pts',(20.2074658464246,-0.0378697858522375,
3.43914000028616));
#46580=CARTESIAN_POINT('Ctrl Pts',(20.2551816824874,0.451321269441671,3.66492646727415));
#46581=CARTESIAN_POINT('Ctrl Pts',(20.3028975185503,0.52583741886325,4.1981749506787));
#46582=CARTESIAN_POINT('Ctrl Pts',(20.3506133546131,0.117885080656874,4.54989459844945));
#46583=CARTESIAN_POINT('Ctrl Pts',(20.398329190676,-0.399119892637424,4.39574851066478));
#46584=CARTESIAN_POINT('Ctrl Pts',(20.438092387395,-0.523197416260526,3.96600412247733));
#46585=CARTESIAN_POINT('Ctrl Pts',(20.4699029447702,-0.3725623900923,3.67462118354637));
#46586=CARTESIAN_POINT('Ctrl Pts',(20.4937608628016,-0.172533290246804,
3.53519650363565));
#46587=CARTESIAN_POINT('Ctrl Pts',(20.5176187808331,0.0720421502968434,
3.50974356844941));
#46588=CARTESIAN_POINT('Ctrl Pts',(20.5414766988645,0.297725647320748,3.60399556061657));
#46589=CARTESIAN_POINT('Ctrl Pts',(20.5653346168959,0.451286063531533,3.79517586539437));
#46590=CARTESIAN_POINT('Ctrl Pts',(20.5891925349273,0.494134760388362,4.03639109206021));
#46591=CARTESIAN_POINT('Ctrl Pts',(20.6130504529587,0.416344747430809,4.26873428690612));
#46592=CARTESIAN_POINT('Ctrl Pts',(20.6369083709901,0.23664610161733,4.43535054865035));
#46593=CARTESIAN_POINT('Ctrl Pts',(20.6607662890216,-0.000865470816140784,
4.49551919950567));
#46594=CARTESIAN_POINT('Ctrl Pts',(20.684624207053,-0.238193741375527,4.43451595913869));
#46595=CARTESIAN_POINT('Ctrl Pts',(20.7084821250844,-0.417262150572256,
4.26726382233879));
#46596=CARTESIAN_POINT('Ctrl Pts',(20.7323400431158,-0.494306543785295,
4.03465729316116));
#46597=CARTESIAN_POINT('Ctrl Pts',(20.7561979611472,-0.45047531426282,3.79357669839993));
#46598=CARTESIAN_POINT('Ctrl Pts',(20.7800558791787,-0.296492828349621,
3.60297191305088));
#46599=CARTESIAN_POINT('Ctrl Pts',(20.80391379721,-0.0700085893017688,3.50945147432983));
#46600=CARTESIAN_POINT('Ctrl Pts',(20.8277717152415,0.173594031734132,3.53588342526713));
#46601=CARTESIAN_POINT('Ctrl Pts',(20.8516296332729,0.374748514455718,3.6758045671588));
#46602=CARTESIAN_POINT('Ctrl Pts',(20.8754875513043,0.484266602122282,3.89500029884494));
#46603=CARTESIAN_POINT('Ctrl Pts',(20.8993454693358,0.475368407265908,4.13987133054223));
#46604=CARTESIAN_POINT('Ctrl Pts',(20.9232033873671,0.350229638882089,4.35054000504804));
#46605=CARTESIAN_POINT('Ctrl Pts',(20.9470613053986,0.139450209771325,4.47549210343221));
#46606=CARTESIAN_POINT('Ctrl Pts',(20.97091922343,-0.105428607968738,4.48417342845956));
#46607=CARTESIAN_POINT('Ctrl Pts',(20.9947771414615,-0.324527251938122,
4.37446116262749));
#46608=CARTESIAN_POINT('Ctrl Pts',(21.0186350594928,-0.464270146732381,
4.17318294187641));
#46609=CARTESIAN_POINT('Ctrl Pts',(21.0424929775243,-0.490486342136868,
3.92955677471355));
#46610=CARTESIAN_POINT('Ctrl Pts',(21.0663508955557,-0.396765267394252,
3.7031558948169));
#46611=CARTESIAN_POINT('Ctrl Pts',(21.0902088135871,-0.206024276530194,
3.54934148458869));
#46612=CARTESIAN_POINT('Ctrl Pts',(21.1140667316185,0.0350952616297792,
3.50572535702762));
#46613=CARTESIAN_POINT('Ctrl Pts',(21.1379246496499,0.267633052506714,3.58297284346672));
#46614=CARTESIAN_POINT('Ctrl Pts',(21.1617825676814,0.434727271782411,3.76219482925797));
#46615=CARTESIAN_POINT('Ctrl Pts',(21.1856404857128,0.495518831419392,3.99956665698474));
#46616=CARTESIAN_POINT('Ctrl Pts',(21.2094984037442,0.43514253908843,4.23704444887943));
#46617=CARTESIAN_POINT('Ctrl Pts',(21.2333563217756,0.268362042918248,4.41655841606373));
#46618=CARTESIAN_POINT('Ctrl Pts',(21.257214239807,0.0359597172125542,4.49421250369607));
#46619=CARTESIAN_POINT('Ctrl Pts',(21.2810721578384,-0.205235738871087,
4.45101817209691));
#46620=CARTESIAN_POINT('Ctrl Pts',(21.3049300758699,-0.396245466293343,
4.29753761193144));
#46621=CARTESIAN_POINT('Ctrl Pts',(21.3287879939013,-0.490362383696085,
4.07130100088706));
#46622=CARTESIAN_POINT('Ctrl Pts',(21.3526459119327,-0.464572341082516,
3.82762935292545));
#46623=CARTESIAN_POINT('Ctrl Pts',(21.3765038299641,-0.325181706377507,
3.62610702345576));
#46624=CARTESIAN_POINT('Ctrl Pts',(21.4003617479955,-0.106275286691508,
3.51601171139131));
#46625=CARTESIAN_POINT('Ctrl Pts',(21.424219666027,0.138618335471326,3.52426471946798));
#46626=CARTESIAN_POINT('Ctrl Pts',(21.4480775840584,0.349615998723735,3.64884796240357));
#46627=CARTESIAN_POINT('Ctrl Pts',(21.4719355020898,0.475123026939619,3.85929744372095));
#46628=CARTESIAN_POINT('Ctrl Pts',(21.4957934201212,0.484449532977353,4.10415253270923));
#46629=CARTESIAN_POINT('Ctrl Pts',(21.5196513381527,0.375314932061802,4.32353949039209));
#46630=CARTESIAN_POINT('Ctrl Pts',(21.543509256184,0.174405606883644,4.4638122296353));
#46631=CARTESIAN_POINT('Ctrl Pts',(21.5673671742155,-0.069150639890911,
4.49067024474121));
#46632=CARTESIAN_POINT('Ctrl Pts',(21.5912250922469,-0.29579767158652,4.39754601941878));
#46633=CARTESIAN_POINT('Ctrl Pts',(21.6150830102783,-0.450114115212426,
4.20721096341231));
#46634=CARTESIAN_POINT('Ctrl Pts',(21.6389409283097,-0.494365396806572,
3.96620718253823));
#46635=CARTESIAN_POINT('Ctrl Pts',(21.6627988463412,-0.417730872638478,
3.73346666603139));
#46636=CARTESIAN_POINT('Ctrl Pts',(21.6866567643726,-0.238949771349764,
3.56590080990214));
#46637=CARTESIAN_POINT('Ctrl Pts',(21.710514682404,-0.00173894210493873,
3.50448403037633));
#46638=CARTESIAN_POINT('Ctrl Pts',(21.7343726004354,0.235897105852373,3.56423440300754));
#46639=CARTESIAN_POINT('Ctrl Pts',(21.7582305184669,0.415849885720624,3.73054133411992));
#46640=CARTESIAN_POINT('Ctrl Pts',(21.7820884364982,0.49411604100673,3.96273824894669));
#46641=CARTESIAN_POINT('Ctrl Pts',(21.8059463545297,0.451557364815975,4.20404667689569));
#46642=CARTESIAN_POINT('Ctrl Pts',(21.8298042725611,0.29858061275206,4.39546013422383));
#46643=CARTESIAN_POINT('Ctrl Pts',(21.8536621905925,0.0725927676976751,
4.49017281661646));
#46644=CARTESIAN_POINT('Ctrl Pts',(21.8775201086239,-0.171145986446082,
4.46502489330693));
#46645=CARTESIAN_POINT('Ctrl Pts',(21.9013780266554,-0.373034884980705,
4.32616571656009));
#46646=CARTESIAN_POINT('Ctrl Pts',(21.9252359446868,-0.483706592871294,
4.10755013753858));
#46647=CARTESIAN_POINT('Ctrl Pts',(21.9490938627182,-0.476098862901817,
3.86263562028194));
#46648=CARTESIAN_POINT('Ctrl Pts',(21.9729517807496,-0.352071992280181,
3.65131043559696));
#46649=CARTESIAN_POINT('Ctrl Pts',(21.996809698781,-0.141953929297546,3.52524934752154));
#46650=CARTESIAN_POINT('Ctrl Pts',(22.0206676168125,0.102875736145779,3.51527772592526));
#46651=CARTESIAN_POINT('Ctrl Pts',(22.0445255348438,0.322549481822576,3.62383390390986));
#46652=CARTESIAN_POINT('Ctrl Pts',(22.0683834528753,0.46335109312246,3.82437293894729));
#46653=CARTESIAN_POINT('Ctrl Pts',(22.0922413709067,0.490850740723195,4.06785757439707));
#46654=CARTESIAN_POINT('Ctrl Pts',(22.1160992889381,0.398324011712033,4.29474918450382));
#46655=CARTESIAN_POINT('Ctrl Pts',(22.1399572069695,0.208396211707814,4.44956659019228));
#46656=CARTESIAN_POINT('Ctrl Pts',(22.163815125001,-0.0324901386554863,
4.49445271863166));
#46657=CARTESIAN_POINT('Ctrl Pts',(22.1876730430324,-0.265431765108271,
4.41843168874211));
#46658=CARTESIAN_POINT('Ctrl Pts',(22.2115309610638,-0.433468094767725,
4.24009271310828));
#46659=CARTESIAN_POINT('Ctrl Pts',(22.2353888790952,-0.495509667838209,
4.00304452911861));
#46660=CARTESIAN_POINT('Ctrl Pts',(22.2592467971266,-0.436385629680506,
3.76525187484075));
#46661=CARTESIAN_POINT('Ctrl Pts',(22.2831047151581,-0.270553418215538,
3.58486153155103));
#46662=CARTESIAN_POINT('Ctrl Pts',(22.3069626331895,-0.0385635261649252,
3.50598385198694));
#46663=CARTESIAN_POINT('Ctrl Pts',(22.3308205512209,0.202856198284482,3.54790657725669));
#46664=CARTESIAN_POINT('Ctrl Pts',(22.3546784692523,0.394672056935096,3.70037845932536));
#46665=CARTESIAN_POINT('Ctrl Pts',(22.3785363872837,0.489979846308564,3.9261159693126));
#46666=CARTESIAN_POINT('Ctrl Pts',(22.4023943053151,0.465474217808745,4.1699201379362));
#46667=CARTESIAN_POINT('Ctrl Pts',(22.4262522233466,0.327147461276091,4.37217420322137));
#46668=CARTESIAN_POINT('Ctrl Pts',(22.450110141378,0.108824243893236,4.4834215400391));
#46669=CARTESIAN_POINT('Ctrl Pts',(22.4739680594094,-0.136109474402841,
4.47645913832327));
#46670=CARTESIAN_POINT('Ctrl Pts',(22.4978259774408,-0.347760701725541,
4.3529895060813));
#46671=CARTESIAN_POINT('Ctrl Pts',(22.5216838954723,-0.474374996640319,
4.1432043106148));
#46672=CARTESIAN_POINT('Ctrl Pts',(22.5455418135036,-0.484991622785221,
3.89840178635216));
#46673=CARTESIAN_POINT('Ctrl Pts',(22.5693997315351,-0.377014700254462,
3.67844274379546));
#46674=CARTESIAN_POINT('Ctrl Pts',(22.5932576495665,-0.176847198578467,
3.53711330196678));
#46675=CARTESIAN_POINT('Ctrl Pts',(22.6171155675979,0.0665638539184235,
3.50897209184919));
#46676=CARTESIAN_POINT('Ctrl Pts',(22.6409734856293,0.293698998435555,3.60090091054846));
#46677=CARTESIAN_POINT('Ctrl Pts',(22.6648314036608,0.449015288492166,3.79041970485759));
#46678=CARTESIAN_POINT('Ctrl Pts',(22.6886893216922,0.494537845944295,4.03118776656693));
#46679=CARTESIAN_POINT('Ctrl Pts',(22.7125472397236,0.419127261608858,4.26432734830583));
#46680=CARTESIAN_POINT('Ctrl Pts',(22.736405157755,0.241238408088568,4.43283588997321));
#46681=CARTESIAN_POINT('Ctrl Pts',(22.7602630757865,0.00434171083240793,
4.49549632518638));
#46682=CARTESIAN_POINT('Ctrl Pts',(22.7841209938178,-0.233581370990537,
4.43700954435219));
#46683=CARTESIAN_POINT('Ctrl Pts',(22.8079789118493,-0.414457183229959,
4.27163232278894));
#46684=CARTESIAN_POINT('Ctrl Pts',(22.8238841905369,-0.46737397936094,4.11714349286348));
#46685=CARTESIAN_POINT('Ctrl Pts',(22.8318368298807,-0.473742730682552,
4.03823705100924));
#46686=CARTESIAN_POINT('Ctrl Pts',(4.,-0.219892372743211,3.64701365460636));
#46687=CARTESIAN_POINT('Ctrl Pts',(4.00795263934381,-0.161099076858729,
3.61038844940468));
#46688=CARTESIAN_POINT('Ctrl Pts',(4.02385791803142,-0.0249198690254346,
3.56711791692558));
#46689=CARTESIAN_POINT('Ctrl Pts',(4.04771583606284,0.185569069288609,3.60813812632505));
#46690=CARTESIAN_POINT('Ctrl Pts',(4.07157375409426,0.350624105231944,3.74494568050885));
#46691=CARTESIAN_POINT('Ctrl Pts',(4.09543167212568,0.429971014252744,3.94413788601839));
#46692=CARTESIAN_POINT('Ctrl Pts',(4.1192895901571,0.40416308778273,4.15698104289539));
#46693=CARTESIAN_POINT('Ctrl Pts',(4.14314750818851,0.279534313346206,4.3314427366163));
#46694=CARTESIAN_POINT('Ctrl Pts',(4.16700542621994,0.0865475313004802,
4.42485517705098));
#46695=CARTESIAN_POINT('Ctrl Pts',(4.19086334425134,-0.127600227202394,
4.41438026490915));
#46696=CARTESIAN_POINT('Ctrl Pts',(4.21472126228278,-0.310547447266788,
4.30257739619942));
#46697=CARTESIAN_POINT('Ctrl Pts',(4.23857918031418,-0.417556725585918,
4.11678647978038));
#46698=CARTESIAN_POINT('Ctrl Pts',(4.26243709834561,-0.422462345057068,
3.90243789311793));
#46699=CARTESIAN_POINT('Ctrl Pts',(4.28629501637703,-0.324064236326554,
3.71194600226016));
#46700=CARTESIAN_POINT('Ctrl Pts',(4.31015293440845,-0.146423688323203,
3.59189110566319));
#46701=CARTESIAN_POINT('Ctrl Pts',(4.33401085243986,0.0670214896752265,
3.5716299793216));
#46702=CARTESIAN_POINT('Ctrl Pts',(4.35786877047129,0.264078061498623,3.65611697628114));
#46703=CARTESIAN_POINT('Ctrl Pts',(4.38172668850271,0.396560367883193,3.82469274783887));
#46704=CARTESIAN_POINT('Ctrl Pts',(4.40558460653412,0.432072854850341,4.03613591352675));
#46705=CARTESIAN_POINT('Ctrl Pts',(4.42944252456555,0.361931763288092,4.23874286631049));
#46706=CARTESIAN_POINT('Ctrl Pts',(4.45330044259696,0.203288494707987,4.382970683851));
#46707=CARTESIAN_POINT('Ctrl Pts',(4.47715836062838,-0.00506434719902249,
4.43355173791626));
#46708=CARTESIAN_POINT('Ctrl Pts',(4.5010162786598,-0.212178818846594,4.37811758201071));
#46709=CARTESIAN_POINT('Ctrl Pts',(4.52487419669122,-0.367409789343613,
4.23022337776645));
#46710=CARTESIAN_POINT('Ctrl Pts',(4.54873211472264,-0.432799058467291,
4.02603328640456));
#46711=CARTESIAN_POINT('Ctrl Pts',(4.57259003275406,-0.392357168499796,
3.8154773474345));
#46712=CARTESIAN_POINT('Ctrl Pts',(4.59644795078547,-0.255973263285106,
3.65004222328625));
#46713=CARTESIAN_POINT('Ctrl Pts',(4.6203058688169,-0.0569969226013119,
3.57018130821703));
#46714=CARTESIAN_POINT('Ctrl Pts',(4.64416378684831,0.155916718210686,3.59542277130738));
#46715=CARTESIAN_POINT('Ctrl Pts',(4.66802170487973,0.330704474340828,3.71959438727947));
#46716=CARTESIAN_POINT('Ctrl Pts',(4.69187962291115,0.424625978282027,3.91233281365517));
#46717=CARTESIAN_POINT('Ctrl Pts',(4.71573754094257,0.41471486395576,4.1265082550995));
#46718=CARTESIAN_POINT('Ctrl Pts',(4.73959545897399,0.303394668785218,4.30974898215573));
#46719=CARTESIAN_POINT('Ctrl Pts',(4.76345337700541,0.117886212792376,4.41724764568232));
#46720=CARTESIAN_POINT('Ctrl Pts',(4.78731129503683,-0.0964486333844469,
4.42271789424177));
#46721=CARTESIAN_POINT('Ctrl Pts',(4.81116921306824,-0.287199161490599,
4.32482210305491));
#46722=CARTESIAN_POINT('Ctrl Pts',(4.83502713109967,-0.407721671464292,
4.14749845969467));
#46723=CARTESIAN_POINT('Ctrl Pts',(4.85888504913109,-0.42854512664958,3.93410742516172));
#46724=CARTESIAN_POINT('Ctrl Pts',(4.8827429671625,-0.344577625034195,3.73682892005441));
#46725=CARTESIAN_POINT('Ctrl Pts',(4.90660088519393,-0.176351507991885,
3.60390291263011));
#46726=CARTESIAN_POINT('Ctrl Pts',(4.93045880322534,0.0349973564730633,
3.56783343253575));
#46727=CARTESIAN_POINT('Ctrl Pts',(4.95431672125677,0.237788413971502,3.63744045016736));
#46728=CARTESIAN_POINT('Ctrl Pts',(4.97817463928818,0.382433727027559,3.79570315365689));
#46729=CARTESIAN_POINT('Ctrl Pts',(5.0020325573196,0.433563576539811,4.00392200101168));
#46730=CARTESIAN_POINT('Ctrl Pts',(5.02589047535102,0.378675321553375,4.21118181228595));
#46731=CARTESIAN_POINT('Ctrl Pts',(5.04974839338244,0.231190635538481,4.36680191797922));
#46732=CARTESIAN_POINT('Ctrl Pts',(5.07360631141386,0.0271735416279573,
4.43272896324296));
#46733=CARTESIAN_POINT('Ctrl Pts',(5.09746422944527,-0.183488223403015,
4.39284198969348));
#46734=CARTESIAN_POINT('Ctrl Pts',(5.1213221474767,-0.349282119693095,4.256894448863));
#46735=CARTESIAN_POINT('Ctrl Pts',(5.1451800655081,-0.4296670234643,4.05812921762123));
#46736=CARTESIAN_POINT('Ctrl Pts',(5.16903798353954,-0.404986636103755,
3.84514980926298));
#46737=CARTESIAN_POINT('Ctrl Pts',(5.19289590157095,-0.281275984601366,
3.67003549057442));
#46738=CARTESIAN_POINT('Ctrl Pts',(5.21675381960238,-0.0887856930599551,
3.5756064824932));
#46739=CARTESIAN_POINT('Ctrl Pts',(5.24061173763379,0.125415118908336,3.58495324968971));
#46740=CARTESIAN_POINT('Ctrl Pts',(5.26446965566521,0.308948518064291,3.69579025298356));
#46741=CARTESIAN_POINT('Ctrl Pts',(5.28832757369662,0.416935588964862,3.88101482593007));
#46742=CARTESIAN_POINT('Ctrl Pts',(5.31218549172805,0.422970551266107,4.09533451502773));
#46743=CARTESIAN_POINT('Ctrl Pts',(5.33604340975946,0.325577692296299,4.28634231834109));
#46744=CARTESIAN_POINT('Ctrl Pts',(5.35990132779089,0.148572219001774,4.40733162501188));
#46745=CARTESIAN_POINT('Ctrl Pts',(5.3837592458223,-0.0647632088646815,
4.42871725387658));
#46746=CARTESIAN_POINT('Ctrl Pts',(5.40761716385372,-0.26226226804932,4.34526983614494));
#46747=CARTESIAN_POINT('Ctrl Pts',(5.43147508188515,-0.395631058815178,
4.17739453851434));
#46748=CARTESIAN_POINT('Ctrl Pts',(5.45533299991656,-0.432257278927009,
3.96614144408682));
#46749=CARTESIAN_POINT('Ctrl Pts',(5.47919091794798,-0.363184819889405,
3.76316768886851));
#46750=CARTESIAN_POINT('Ctrl Pts',(5.5030488359794,-0.205303779432806,3.61810588490468));
#46751=CARTESIAN_POINT('Ctrl Pts',(5.52690675401082,0.00277962745745752,
3.56642759466814));
#46752=CARTESIAN_POINT('Ctrl Pts',(5.55076467204224,0.210183339719457,3.62076956781107));
#46753=CARTESIAN_POINT('Ctrl Pts',(5.57462259007365,0.36619150013966,3.76784371165257));
#46754=CARTESIAN_POINT('Ctrl Pts',(5.59848050810508,0.432655863921731,3.97168639180759));
#46755=CARTESIAN_POINT('Ctrl Pts',(5.62233842613649,0.393324083661671,4.18245252040861));
#46756=CARTESIAN_POINT('Ctrl Pts',(5.64619634416792,0.257813851021257,4.34860403787086));
#46757=CARTESIAN_POINT('Ctrl Pts',(5.67005426219933,0.0592611090830247,
4.42951237227525));
#46758=CARTESIAN_POINT('Ctrl Pts',(5.69391218023075,-0.153782588238227,
4.40539323200473));
#46759=CARTESIAN_POINT('Ctrl Pts',(5.71777009826218,-0.329222253834466,
4.28214440376531));
#46760=CARTESIAN_POINT('Ctrl Pts',(5.74162801629359,-0.424158110434281,
4.08990358344764));
#46761=CARTESIAN_POINT('Ctrl Pts',(5.76548593432501,-0.415375755386326,
3.8756788878607));
#46762=CARTESIAN_POINT('Ctrl Pts',(5.78934385235642,-0.305022713182347,
3.69185409099321));
#46763=CARTESIAN_POINT('Ctrl Pts',(5.81320177038785,-0.120083309624962,
3.58337936191985));
#46764=CARTESIAN_POINT('Ctrl Pts',(5.83705968841926,0.0942197354074567,
3.57677972866706));
#46765=CARTESIAN_POINT('Ctrl Pts',(5.86091760645069,0.285483486244351,3.673668977605));
#46766=CARTESIAN_POINT('Ctrl Pts',(5.8847755244821,0.406938752801468,3.85035505520226));
#46767=CARTESIAN_POINT('Ctrl Pts',(5.90863344251353,0.428886400972996,4.06363338935351));
#46768=CARTESIAN_POINT('Ctrl Pts',(5.93249136054494,0.345959657594393,4.261351642888));
#46769=CARTESIAN_POINT('Ctrl Pts',(5.95634927857636,0.178436323746589,4.39516226965834));
#46770=CARTESIAN_POINT('Ctrl Pts',(5.98020719660778,-0.0327194942966983,
4.4323450160316));
#46771=CARTESIAN_POINT('Ctrl Pts',(6.0040651146392,-0.23587461323539,4.36380751861078));
#46772=CARTESIAN_POINT('Ctrl Pts',(6.02792303267061,-0.381351759249696,
4.20630938167977));
#46773=CARTESIAN_POINT('Ctrl Pts',(6.05178095070204,-0.433578399193506,
3.9983625870902));
#46774=CARTESIAN_POINT('Ctrl Pts',(6.07563886873346,-0.379782579589031,
3.79081692866841));
#46775=CARTESIAN_POINT('Ctrl Pts',(6.09949678676487,-0.233120953551068,
3.63442082419035));
#46776=CARTESIAN_POINT('Ctrl Pts',(6.12335470479629,-0.0294522997972467,
3.5674214393556));
#46777=CARTESIAN_POINT('Ctrl Pts',(6.14721262282771,0.181413325723775,3.60619428643423));
#46778=CARTESIAN_POINT('Ctrl Pts',(6.17107054085913,0.347927737305898,3.74127281623538));
#46779=CARTESIAN_POINT('Ctrl Pts',(6.19492845889055,0.429346806292137,3.93959933010928));
#46780=CARTESIAN_POINT('Ctrl Pts',(6.21878637692197,0.405811992579865,4.15272917617017));
#46781=CARTESIAN_POINT('Ctrl Pts',(6.24264429495339,0.282982581651336,4.32844890303245));
#46782=CARTESIAN_POINT('Ctrl Pts',(6.26650221298481,0.0910742457207041,
4.42397415233781));
#46783=CARTESIAN_POINT('Ctrl Pts',(6.29036013101623,-0.123327005978964,
4.41559921078967));
#46784=CARTESIAN_POINT('Ctrl Pts',(6.31421804904765,-0.307151379675736,
4.3060270879454));
#46785=CARTESIAN_POINT('Ctrl Pts',(6.33807596707907,-0.416657206472865,
4.12081787696614));
#46786=CARTESIAN_POINT('Ctrl Pts',(6.36193388511048,-0.422829889105799,
3.9075587958503));
#46787=CARTESIAN_POINT('Ctrl Pts',(6.39374444248571,-0.296437506874183,
3.64987069373525));
#46788=CARTESIAN_POINT('Ctrl Pts',(6.43350763920474,0.0703302468340302,
3.51324810367198));
#46789=CARTESIAN_POINT('Ctrl Pts',(6.48122347526758,0.448014600657906,3.7964368525222));
#46790=CARTESIAN_POINT('Ctrl Pts',(6.52893931133042,0.413240052911115,4.26646358767058));
#46791=CARTESIAN_POINT('Ctrl Pts',(6.57665514739325,-0.000480251589724132,
4.49184654025612));
#46792=CARTESIAN_POINT('Ctrl Pts',(6.62437098345609,-0.41404349770976,4.26553045144514));
#46793=CARTESIAN_POINT('Ctrl Pts',(6.67208681951894,-0.447234019333667,
3.79538894860702));
#46794=CARTESIAN_POINT('Ctrl Pts',(6.71980265558177,-0.0698021891909718,
3.51313682319347));
#46795=CARTESIAN_POINT('Ctrl Pts',(6.76751849164461,0.371772181936036,3.67798293440124));
#46796=CARTESIAN_POINT('Ctrl Pts',(6.81523432770745,0.471920133146607,4.13853999974893));
#46797=CARTESIAN_POINT('Ctrl Pts',(6.86295016377028,0.138708377331583,4.4718748549198));
#46798=CARTESIAN_POINT('Ctrl Pts',(6.91066599983312,-0.32188767172048,4.37187913281409));
#46799=CARTESIAN_POINT('Ctrl Pts',(6.95838183589596,-0.486886005735063,
3.93038141845316));
#46800=CARTESIAN_POINT('Ctrl Pts',(7.0060976719588,-0.204771183672361,3.55281534000283));
#46801=CARTESIAN_POINT('Ctrl Pts',(7.05381350802163,0.265389096458903,3.58590591031157));
#46802=CARTESIAN_POINT('Ctrl Pts',(7.10152934408448,0.491837993618785,3.99926540470374));
#46803=CARTESIAN_POINT('Ctrl Pts',(7.14924518014731,0.266624753986561,4.41329951581085));
#46804=CARTESIAN_POINT('Ctrl Pts',(7.19696101621015,-0.203434237821079,
4.44779430805676));
#46805=CARTESIAN_POINT('Ctrl Pts',(7.24467685227299,-0.486676365692783,
4.07107270446015));
#46806=CARTESIAN_POINT('Ctrl Pts',(7.29239268833582,-0.322996137187983,
3.62908393881966));
#46807=CARTESIAN_POINT('Ctrl Pts',(7.34010852439867,0.137296434535941,3.52771310152703));
#46808=CARTESIAN_POINT('Ctrl Pts',(7.3878243604615,0.471507566988788,3.86005058906394));
#46809=CARTESIAN_POINT('Ctrl Pts',(7.43554019652434,0.372726051350611,4.32090577464778));
#46810=CARTESIAN_POINT('Ctrl Pts',(7.48325603258718,-0.0683355354161961,
4.48706824929225));
#46811=CARTESIAN_POINT('Ctrl Pts',(7.53097186865002,-0.44664354691983,4.20594845626764));
#46812=CARTESIAN_POINT('Ctrl Pts',(7.57868770471286,-0.414791917646955,
3.73570302684109));
#46813=CARTESIAN_POINT('Ctrl Pts',(7.62640354077569,-0.00203048755240202,
3.50816557464413));
#46814=CARTESIAN_POINT('Ctrl Pts',(7.67411937683853,0.412595570264971,3.73228724307244));
#46815=CARTESIAN_POINT('Ctrl Pts',(7.72183521290137,0.448328767436039,4.20225365549051));
#46816=CARTESIAN_POINT('Ctrl Pts',(7.7695510489642,0.0723547589785895,4.48648742399228));
#46817=CARTESIAN_POINT('Ctrl Pts',(7.81726688502705,-0.370063737934377,
4.32397230547438));
#46818=CARTESIAN_POINT('Ctrl Pts',(7.86498272108989,-0.472647010158531,
3.86394843388276));
#46819=CARTESIAN_POINT('Ctrl Pts',(7.91269855715272,-0.141191260335066,
3.52886280888004));
#46820=CARTESIAN_POINT('Ctrl Pts',(7.96041439321556,0.31992259635559,3.62642971585976));
#46821=CARTESIAN_POINT('Ctrl Pts',(8.0081302292784,0.48724661017382,4.0670519628834));
#46822=CARTESIAN_POINT('Ctrl Pts',(8.05584606534124,0.207124564615173,4.44609936066402));
#46823=CARTESIAN_POINT('Ctrl Pts',(8.10356190140407,-0.263203155649882,
4.41548685142597));
#46824=CARTESIAN_POINT('Ctrl Pts',(8.15127773746691,-0.491827368180951,
4.00332637343646));
#46825=CARTESIAN_POINT('Ctrl Pts',(8.19899357352975,-0.268798940774433,
3.58811123553743));
#46826=CARTESIAN_POINT('Ctrl Pts',(8.24670940959259,0.201071689948468,3.55113988776764));
#46827=CARTESIAN_POINT('Ctrl Pts',(8.29442524565542,0.486295093906121,3.92636368766143));
#46828=CARTESIAN_POINT('Ctrl Pts',(8.34214108171827,0.324946230517931,4.36920884621601));
#46829=CARTESIAN_POINT('Ctrl Pts',(8.3898569177811,-0.134805756295296,4.47300384028212));
#46830=CARTESIAN_POINT('Ctrl Pts',(8.43757275384394,-0.470763542849379,
4.14243212971755));
#46831=CARTESIAN_POINT('Ctrl Pts',(8.48528858990678,-0.37441192437669,3.68106280283335));
#46832=CARTESIAN_POINT('Ctrl Pts',(8.53300442596962,0.0657679253190804,
3.51257841158684));
#46833=CARTESIAN_POINT('Ctrl Pts',(8.58072026203246,0.445552077224736,3.79170076492532));
#46834=CARTESIAN_POINT('Ctrl Pts',(8.62843609809529,0.41617890091499,4.26210751092856));
#46835=CARTESIAN_POINT('Ctrl Pts',(8.67615193415813,0.0046222361594965,
4.49181689660367));
#46836=CARTESIAN_POINT('Ctrl Pts',(8.72386777022097,-0.411179099183508,
4.26988325855195));
#46837=CARTESIAN_POINT('Ctrl Pts',(8.7715836062838,-0.449388340942622,3.80011167148426));
#46838=CARTESIAN_POINT('Ctrl Pts',(8.81929944234665,-0.0749173544856965,
3.51390061216986));
#46839=CARTESIAN_POINT('Ctrl Pts',(8.86701527840948,0.368351391347115,3.67408210030036));
#46840=CARTESIAN_POINT('Ctrl Pts',(8.91473111447233,0.473357386691186,4.13355901061654));
#46841=CARTESIAN_POINT('Ctrl Pts',(8.96244695053515,0.14367201029714,4.47038662641401));
#46842=CARTESIAN_POINT('Ctrl Pts',(9.01016278659801,-0.317949583830803,
4.37525096534692));
#46843=CARTESIAN_POINT('Ctrl Pts',(9.05787862266083,-0.487593182843731,
3.93551656882348));
#46844=CARTESIAN_POINT('Ctrl Pts',(9.10559445872368,-0.209472459465777,
3.55499829935456));
#46845=CARTESIAN_POINT('Ctrl Pts',(9.15331029478651,0.261010046587687,3.58313193881964));
#46846=CARTESIAN_POINT('Ctrl Pts',(9.20102613084934,0.491803010703882,3.99408193320625));
#46847=CARTESIAN_POINT('Ctrl Pts',(9.2487419669122,0.270965702728691,4.41046657939073));
#46848=CARTESIAN_POINT('Ctrl Pts',(9.29645780297501,-0.198703579405513,
4.44991344988054));
#46849=CARTESIAN_POINT('Ctrl Pts',(9.34417363903789,-0.485900307124067,
4.07619787653679));
#46850=CARTESIAN_POINT('Ctrl Pts',(9.39188947510068,-0.326887306273347,
3.63250862071426));
#46851=CARTESIAN_POINT('Ctrl Pts',(9.43960531116356,0.13231133773591,3.52629235307153));
#46852=CARTESIAN_POINT('Ctrl Pts',(9.48732114722637,0.470006444430667,3.85508910653225));
#46853=CARTESIAN_POINT('Ctrl Pts',(9.53503698328922,0.376087401226012,4.31695976320512));
#46854=CARTESIAN_POINT('Ctrl Pts',(9.58275281935206,-0.0631984893729827,
4.48776139227388));
#46855=CARTESIAN_POINT('Ctrl Pts',(9.63046865541489,-0.444448234747017,
4.21064422964382));
#46856=CARTESIAN_POINT('Ctrl Pts',(9.67818449147773,-0.41755432743774,3.74008922975375));
#46857=CARTESIAN_POINT('Ctrl Pts',(9.72590032754057,-0.00721385634321597,
3.50821428942208));
#46858=CARTESIAN_POINT('Ctrl Pts',(9.77361616360341,0.40975121003073,3.72795373420991));
#46859=CARTESIAN_POINT('Ctrl Pts',(9.82133199966624,0.450435435400681,4.19751745084266));
#46860=CARTESIAN_POINT('Ctrl Pts',(9.86904783572909,0.077477869602138,4.48569785316993));
#46861=CARTESIAN_POINT('Ctrl Pts',(9.91676367179192,-0.366628816002305,
4.3278544435092));
#46862=CARTESIAN_POINT('Ctrl Pts',(9.96447950785476,-0.474054618562381,
3.8689372536849));
#46863=CARTESIAN_POINT('Ctrl Pts',(10.0121953439176,-0.146148770628728,
3.53037700046135));
#46864=CARTESIAN_POINT('Ctrl Pts',(10.0599111799804,0.315967742161179,3.62307877379278));
#46865=CARTESIAN_POINT('Ctrl Pts',(10.1076270160433,0.487926215535836,4.06191310882887));
#46866=CARTESIAN_POINT('Ctrl Pts',(10.1553428521061,0.211814537474087,4.44389168337175));
#46867=CARTESIAN_POINT('Ctrl Pts',(10.203058688169,-0.258809689535701,4.4182376949229));
#46868=CARTESIAN_POINT('Ctrl Pts',(10.2507745242318,-0.491764996345908,
4.00850959581219));
#46869=CARTESIAN_POINT('Ctrl Pts',(10.2984903602946,-0.273124940234581,
3.59096700393021));
#46870=CARTESIAN_POINT('Ctrl Pts',(10.3462061963575,0.196329951061554,3.54904570612073));
#46871=CARTESIAN_POINT('Ctrl Pts',(10.3939220324203,0.485492027373267,3.92124267520431));
#46872=CARTESIAN_POINT('Ctrl Pts',(10.4416378684831,0.328819304693055,4.36576370748498));
#46873=CARTESIAN_POINT('Ctrl Pts',(10.489353704546,-0.129813245022134,4.47439829918413));
#46874=CARTESIAN_POINT('Ctrl Pts',(10.5370695406088,-0.469236294399976,
4.14738563318641));
#46875=CARTESIAN_POINT('Ctrl Pts',(10.5847853766716,-0.377752434501872,
3.68502647241413));
#46876=CARTESIAN_POINT('Ctrl Pts',(10.6325012127345,0.0606272984676223,
3.51191234851464));
#46877=CARTESIAN_POINT('Ctrl Pts',(10.6802170487973,0.443332050383407,3.78701662516801));
#46878=CARTESIAN_POINT('Ctrl Pts',(10.7279328848602,0.418918158891686,4.25770681210006));
#46879=CARTESIAN_POINT('Ctrl Pts',(10.775648720923,0.00980527620531799,
4.49174086815163));
#46880=CARTESIAN_POINT('Ctrl Pts',(10.8233645569858,-0.408311942493964,
4.27420171857372));
#46881=CARTESIAN_POINT('Ctrl Pts',(10.8710803930487,-0.451470021714238,
3.80485891169382));
#46882=CARTESIAN_POINT('Ctrl Pts',(10.9187962291115,-0.080036233235122,
3.51471716883706));
#46883=CARTESIAN_POINT('Ctrl Pts',(10.9665120651743,0.364896059739551,3.6702181168734));
#46884=CARTESIAN_POINT('Ctrl Pts',(11.0142279012372,0.47473868640782,4.1285628425314));
#46885=CARTESIAN_POINT('Ctrl Pts',(11.0619437373,0.148621472554162,4.46884633169921));
#46886=CARTESIAN_POINT('Ctrl Pts',(11.1096595733629,-0.313977126381285,
4.37858102033954));
#46887=CARTESIAN_POINT('Ctrl Pts',(11.1573754094257,-0.488245699001722,
3.94065893278431));
#46888=CARTESIAN_POINT('Ctrl Pts',(11.2050912454886,-0.214150733603143,
3.55723066033293));
#46889=CARTESIAN_POINT('Ctrl Pts',(11.2528070815514,0.256602145595791,3.58040428537983));
#46890=CARTESIAN_POINT('Ctrl Pts',(11.3005229176142,0.491713326162588,3.98889911147238));
#46891=CARTESIAN_POINT('Ctrl Pts',(11.3482387536771,0.275276593332242,4.40758805430897));
#46892=CARTESIAN_POINT('Ctrl Pts',(11.3959545897399,-0.193950870829933,
4.45198261532529));
#46893=CARTESIAN_POINT('Ctrl Pts',(11.4436704258028,-0.485070265991237,
4.08131458604192));
#46894=CARTESIAN_POINT('Ctrl Pts',(11.4913862618656,-0.330742172127369,
3.63597412121053));
#46895=CARTESIAN_POINT('Ctrl Pts',(11.5391020979284,0.127311547523522,3.52492422212962));
#46896=CARTESIAN_POINT('Ctrl Pts',(11.5868179339912,0.468453114143607,3.85014371984754));
#46897=CARTESIAN_POINT('Ctrl Pts',(11.6345337700541,0.379406977967949,4.31297854546471));
#46898=CARTESIAN_POINT('Ctrl Pts',(11.6822496061169,-0.0580544240024287,
4.48840035698771));
#46899=CARTESIAN_POINT('Ctrl Pts',(11.7299654421798,-0.44220355512924,4.21531660568344));
#46900=CARTESIAN_POINT('Ctrl Pts',(11.7776812782426,-0.420270357404582,
3.74450430230823));
#46901=CARTESIAN_POINT('Ctrl Pts',(11.8253971143054,-0.0123964237846327,
3.50831762943));
#46902=CARTESIAN_POINT('Ctrl Pts',(11.8731129503683,0.406861336540243,3.72365044295193));
#46903=CARTESIAN_POINT('Ctrl Pts',(11.9208287864311,0.452492071153857,4.1927593068956));
#46904=CARTESIAN_POINT('Ctrl Pts',(11.968544622494,0.0825923743414284,4.48485433333386));
#46905=CARTESIAN_POINT('Ctrl Pts',(12.0162604585568,-0.363153170675764,
4.33170016502878));
#46906=CARTESIAN_POINT('Ctrl Pts',(12.0639762946196,-0.475409571231627,
3.87394063131468));
#46907=CARTESIAN_POINT('Ctrl Pts',(12.1116921306825,-0.151090047408964,
3.53194335553704));
#46908=CARTESIAN_POINT('Ctrl Pts',(12.1594079667453,0.311977791768556,3.61976969834691));
#46909=CARTESIAN_POINT('Ctrl Pts',(12.2071238028081,0.488551624369653,4.05676737776005));
#46910=CARTESIAN_POINT('Ctrl Pts',(12.254839638871,0.216480982979095,4.44163470069774));
#46911=CARTESIAN_POINT('Ctrl Pts',(12.3025554749338,-0.254387476069249,
4.42094208256136));
#46912=CARTESIAN_POINT('Ctrl Pts',(12.3502713109967,-0.49164800158875,4.0136918729824));
#46913=CARTESIAN_POINT('Ctrl Pts',(12.3979871470595,-0.277420602272412,
3.59386820576715));
#46914=CARTESIAN_POINT('Ctrl Pts',(12.4457029831224,0.191566404775332,3.54700161433684));
#46915=CARTESIAN_POINT('Ctrl Pts',(12.4934188191852,0.484635034689867,3.91613041073711));
#46916=CARTESIAN_POINT('Ctrl Pts',(12.541134655248,0.332655855180181,4.362277941457));
#46917=CARTESIAN_POINT('Ctrl Pts',(12.5888504913109,-0.124806314709729,
4.47574006417428));
#46918=CARTESIAN_POINT('Ctrl Pts',(12.6365663273737,-0.4676569254097,4.15232276575852));
#46919=CARTESIAN_POINT('Ctrl Pts',(12.6842821634365,-0.381050985679211,
3.68902512775968));
#46920=CARTESIAN_POINT('Ctrl Pts',(12.7319979994994,0.0554799374235607,
3.5113004999026));
#46921=CARTESIAN_POINT('Ctrl Pts',(12.7797138355622,0.441062780321708,3.78235614259331));
#46922=CARTESIAN_POINT('Ctrl Pts',(12.8274296716251,0.421610885427219,4.2532774884218));
#46923=CARTESIAN_POINT('Ctrl Pts',(12.8751455076879,0.0149872271275763,
4.49161021945745));
#46924=CARTESIAN_POINT('Ctrl Pts',(12.9228613437507,-0.405399432451448,
4.27848972156979));
#46925=CARTESIAN_POINT('Ctrl Pts',(12.9705771798136,-0.453501555338242,
3.80962782724943));
#46926=CARTESIAN_POINT('Ctrl Pts',(13.0182930158764,-0.0851462219395619,
3.51558762841831));
#46927=CARTESIAN_POINT('Ctrl Pts',(13.0660088519392,0.361400197209248,3.66639076405307));
#46928=CARTESIAN_POINT('Ctrl Pts',(13.1137246880021,0.476067254403989,4.1235523942958));
#46929=CARTESIAN_POINT('Ctrl Pts',(13.1614405240649,0.153554426643267,4.46725395975876));
#46930=CARTESIAN_POINT('Ctrl Pts',(13.2091563601278,-0.30996979384252,4.38186902434892));
#46931=CARTESIAN_POINT('Ctrl Pts',(13.2568721961906,-0.488843983144383,
3.94580788806928));
#46932=CARTESIAN_POINT('Ctrl Pts',(13.3045880322534,-0.218805220893238,
3.55951220202843));
#46933=CARTESIAN_POINT('Ctrl Pts',(13.3523038683163,0.252165742455243,3.57772323864086));
#46934=CARTESIAN_POINT('Ctrl Pts',(13.4000197043791,0.491569024438394,3.98371752277252));
#46935=CARTESIAN_POINT('Ctrl Pts',(13.447735540442,0.279556907518101,4.40466425628032));
#46936=CARTESIAN_POINT('Ctrl Pts',(13.4954513765048,-0.189176619112,4.45400157668594));
#46937=CARTESIAN_POINT('Ctrl Pts',(13.5431672125676,-0.484186345555107,
4.08642226350871));
#46938=CARTESIAN_POINT('Ctrl Pts',(13.5908830486304,-0.334560300710407,
3.63948005597396));
#46939=CARTESIAN_POINT('Ctrl Pts',(13.6385988846933,0.122297616148583,3.52360886035071));
#46940=CARTESIAN_POINT('Ctrl Pts',(13.6863147207561,0.466847750307624,3.8452149784873));
#46941=CARTESIAN_POINT('Ctrl Pts',(13.734030556819,0.3826844119832,4.30896256355269));
#46942=CARTESIAN_POINT('Ctrl Pts',(13.7817463928818,-0.0529039102219543,
4.48898507250754));
#46943=CARTESIAN_POINT('Ctrl Pts',(13.8294622289446,-0.439909757638992,
4.21996506537626));
#46944=CARTESIAN_POINT('Ctrl Pts',(13.8771780650075,-0.422939705734467,
3.74894775411238));
#46945=CARTESIAN_POINT('Ctrl Pts',(13.9248939010703,-0.0175776142901187,
3.50847558318244));
#46946=CARTESIAN_POINT('Ctrl Pts',(13.9726097371332,0.403926270823208,3.71937784729135));
#46947=CARTESIAN_POINT('Ctrl Pts',(14.020325573196,0.454498446235019,4.18797975215946));
#46948=CARTESIAN_POINT('Ctrl Pts',(14.0680414092588,0.0876977051117048,
4.48395695817926));
#46949=CARTESIAN_POINT('Ctrl Pts',(14.1157572453217,-0.359637188018331,
4.33550904286807));
#46950=CARTESIAN_POINT('Ctrl Pts',(14.1634730813845,-0.476711717661702,
3.87895801102093));
#46951=CARTESIAN_POINT('Ctrl Pts',(14.2111889174473,-0.156014541823709,
3.53356170012368));
#46952=CARTESIAN_POINT('Ctrl Pts',(14.2589047535102,0.307953188363286,3.61650285707861));
#46953=CARTESIAN_POINT('Ctrl Pts',(14.306620589573,0.4891227672074,4.05161534124029));
#46954=CARTESIAN_POINT('Ctrl Pts',(14.3543364256359,0.2211233828038,4.4393286633369));
#46955=CARTESIAN_POINT('Ctrl Pts',(14.4020522616987,-0.249937006449114,
4.42359971395084));
#46956=CARTESIAN_POINT('Ctrl Pts',(14.4497680977616,-0.491476396904638,
4.01887262932433));
#46957=CARTESIAN_POINT('Ctrl Pts',(14.4974839338244,-0.281685449746218,
3.59681451879656));
#46958=CARTESIAN_POINT('Ctrl Pts',(14.5451997698872,0.186781580201919,3.54500783946397));
#46959=CARTESIAN_POINT('Ctrl Pts',(14.59291560595,0.483724211046603,3.91102746210588));
#46960=CARTESIAN_POINT('Ctrl Pts',(14.6406314420129,0.33645545583349,4.35875193531444));
#46961=CARTESIAN_POINT('Ctrl Pts',(14.6883472780757,-0.119785521504147,
4.47702898621568));
#46962=CARTESIAN_POINT('Ctrl Pts',(14.7360631141386,-0.466025611307368,
4.15724297904063));
#46963=CARTESIAN_POINT('Ctrl Pts',(14.7837789502014,-0.38430721152129,3.69305832471834));
#46964=CARTESIAN_POINT('Ctrl Pts',(14.8314947862642,0.0503264139313189,
3.51074293371195));
#46965=CARTESIAN_POINT('Ctrl Pts',(14.8792106223271,0.438744519099385,3.77771983486548));
#46966=CARTESIAN_POINT('Ctrl Pts',(14.9269264583899,0.42425678142631,4.24882003188202));
#46967=CARTESIAN_POINT('Ctrl Pts',(14.9746422944528,0.0201675133397715,
4.49142496503298));
#46968=CARTESIAN_POINT('Ctrl Pts',(15.0223581305156,-0.402441892563756,
4.28274679124913));
#46969=CARTESIAN_POINT('Ctrl Pts',(15.0700739665785,-0.455482716161518,
3.8144178884426));
#46970=CARTESIAN_POINT('Ctrl Pts',(15.1177898026413,-0.0902467530057116,
3.51651189422706));
#46971=CARTESIAN_POINT('Ctrl Pts',(15.1655056387041,0.357864192060027,3.66260046696357));
#46972=CARTESIAN_POINT('Ctrl Pts',(15.2132214747669,0.47734294310866,4.11852822244656));
#46973=CARTESIAN_POINT('Ctrl Pts',(15.2609373108298,0.15847032463534,4.46560968746574));
#46974=CARTESIAN_POINT('Ctrl Pts',(15.3086531468926,-0.305928031329979,
4.38511461215921));
#46975=CARTESIAN_POINT('Ctrl Pts',(15.3563689829555,-0.489387968817152,
3.95096286275689));
#46976=CARTESIAN_POINT('Ctrl Pts',(15.4040848190183,-0.223435404337718,
3.56184267101825));
#46977=CARTESIAN_POINT('Ctrl Pts',(15.4518006550811,0.24770132994065,3.57508909640066));
#46978=CARTESIAN_POINT('Ctrl Pts',(15.499516491144,0.491370121559653,3.97853774265298));
#46979=CARTESIAN_POINT('Ctrl Pts',(15.5472323272068,0.283806169849271,4.40169551006635));
#46980=CARTESIAN_POINT('Ctrl Pts',(15.5949481632697,-0.184381354552937,
4.4559701097059));
#46981=CARTESIAN_POINT('Ctrl Pts',(15.6426639993325,-0.483248643997369,
4.09152034160055));
#46982=CARTESIAN_POINT('Ctrl Pts',(15.6903798353953,-0.338341267922855,
3.64302603558196));
#46983=CARTESIAN_POINT('Ctrl Pts',(15.7380956714582,0.117270100534806,3.52234641383892));
#46984=CARTESIAN_POINT('Ctrl Pts',(15.785811507521,0.465190531238913,3.84030342991275));
#46985=CARTESIAN_POINT('Ctrl Pts',(15.8335273435838,0.385919339229949,4.30491226354526));
#46986=CARTESIAN_POINT('Ctrl Pts',(15.8812431796467,-0.0477475201261761,
4.48951547388594));
#46987=CARTESIAN_POINT('Ctrl Pts',(15.9289590157095,-0.437567097060412,
4.22458909239344));
#46988=CARTESIAN_POINT('Ctrl Pts',(15.9766748517724,-0.425562075928853,
3.75341909160864));
#46989=CARTESIAN_POINT('Ctrl Pts',(16.0243906878352,-0.0227568523576073,
3.50868813313462));
#46990=CARTESIAN_POINT('Ctrl Pts',(16.072106523898,0.400946338892803,3.71513642180785));
#46991=CARTESIAN_POINT('Ctrl Pts',(16.1198223599609,0.456454337785543,4.1831793175245));
#46992=CARTESIAN_POINT('Ctrl Pts',(16.1675381960237,0.0927932948370443,
4.4830058273823));
#46993=CARTESIAN_POINT('Ctrl Pts',(16.2152540320865,-0.356081258568678,
4.33928065395499));
#46994=CARTESIAN_POINT('Ctrl Pts',(16.2629698681494,-0.477960913216358,
3.88398883549692));
#46995=CARTESIAN_POINT('Ctrl Pts',(16.3106857042122,-0.160921706883503,
3.53523185446324));
#46996=CARTESIAN_POINT('Ctrl Pts',(16.358401540275,0.303894378979202,3.6132786128531));
#46997=CARTESIAN_POINT('Ctrl Pts',(16.4061173763379,0.489639580609251,4.04645757153336));
#46998=CARTESIAN_POINT('Ctrl Pts',(16.4538332124007,0.225741221292456,4.43697382743292));
#46999=CARTESIAN_POINT('Ctrl Pts',(16.5015490484636,-0.245458775012363,
4.42621029389423));
#47000=CARTESIAN_POINT('Ctrl Pts',(16.5492648845264,-0.4912502013546,4.02405128938415));
#47001=CARTESIAN_POINT('Ctrl Pts',(16.5969807205893,-0.285919008936969,
3.59980561575594));
#47002=CARTESIAN_POINT('Ctrl Pts',(16.6446965566521,0.181976008816936,3.54306460296116));
#47003=CARTESIAN_POINT('Ctrl Pts',(16.6924123927149,0.482759657613431,3.90593439612197));
#47004=CARTESIAN_POINT('Ctrl Pts',(16.7401282287778,0.340217684611379,4.35518608070932));
#47005=CARTESIAN_POINT('Ctrl Pts',(16.7878440648406,-0.114751423091257,
4.47826492214097));
#47006=CARTESIAN_POINT('Ctrl Pts',(16.8355599009034,-0.464342533291602,
4.16214572651883));
#47007=CARTESIAN_POINT('Ctrl Pts',(16.8832757369663,-0.387520750342007,
3.69712561530174));
#47008=CARTESIAN_POINT('Ctrl Pts',(16.9309915730291,0.0451673004198413,
3.51023971187451));
#47009=CARTESIAN_POINT('Ctrl Pts',(16.978707409092,0.436377524217892,3.7731082169636));
#47010=CARTESIAN_POINT('Ctrl Pts',(17.0264232451548,0.426855552995382,4.24433493759383));
#47011=CARTESIAN_POINT('Ctrl Pts',(17.0741390812176,0.0253455594402812,
4.49118512545541));
#47012=CARTESIAN_POINT('Ctrl Pts',(17.1218549172805,-0.399439651340385,
4.28697245475663));
#47013=CARTESIAN_POINT('Ctrl Pts',(17.1695707533433,-0.457413284126125,
3.81922856321607));
#47014=CARTESIAN_POINT('Ctrl Pts',(17.2172865894061,-0.0953372598908034,
3.51748986360026));
#47015=CARTESIAN_POINT('Ctrl Pts',(17.265002425469,0.354288437054553,3.6588476466131));
#47016=CARTESIAN_POINT('Ctrl Pts',(17.3127182615318,0.478565610824392,4.11349088504481));
#47017=CARTESIAN_POINT('Ctrl Pts',(17.3604340975947,0.163368620495752,4.46391369745815));
#47018=CARTESIAN_POINT('Ctrl Pts',(17.4081499336575,-0.301852287783465,
4.38831742326589));
#47019=CARTESIAN_POINT('Ctrl Pts',(17.4558657697204,-0.489877595596684,
3.956123284257));
#47020=CARTESIAN_POINT('Ctrl Pts',(17.5035816057832,-0.228040769637767,
3.56422180844494));
#47021=CARTESIAN_POINT('Ctrl Pts',(17.551297441846,0.243209403937772,3.57250215124727));
#47022=CARTESIAN_POINT('Ctrl Pts',(17.5990132779089,0.491116639619549,3.97336034645914));
#47023=CARTESIAN_POINT('Ctrl Pts',(17.6467291139717,0.288023908337871,4.39868214542132));
#47024=CARTESIAN_POINT('Ctrl Pts',(17.6944449500345,-0.179565609787963,
4.45788799572981));
#47025=CARTESIAN_POINT('Ctrl Pts',(17.7421607860973,-0.48225726547346,4.09660825404716));
#47026=CARTESIAN_POINT('Ctrl Pts',(17.7898766221602,-0.342084653792828,
3.64661166616396));
#47027=CARTESIAN_POINT('Ctrl Pts',(17.837592458223,0.112229559114723,3.52113702282083));
#47028=CARTESIAN_POINT('Ctrl Pts',(17.8853082942859,0.463481641013499,3.83540961967535));
#47029=CARTESIAN_POINT('Ctrl Pts',(17.9330241303487,0.389111400387848,4.30082809533052));
#47030=CARTESIAN_POINT('Ctrl Pts',(17.9807399664116,-0.0425858264624495,
4.48999150220845));
#47031=CARTESIAN_POINT('Ctrl Pts',(18.0284558024744,-0.435175833605105,
4.22918817311999));
#47032=CARTESIAN_POINT('Ctrl Pts',(18.0761716385373,-0.428137176707308,
3.75791781814212));
#47033=CARTESIAN_POINT('Ctrl Pts',(18.1238874746,-0.0279335627019553,3.5089552556775));
#47034=CARTESIAN_POINT('Ctrl Pts',(18.1716033106629,0.397921871745719,3.71092663761881));
#47035=CARTESIAN_POINT('Ctrl Pts',(18.2193191467257,0.458359528554279,4.17835853620019));
#47036=CARTESIAN_POINT('Ctrl Pts',(18.2670349827886,0.097878577523561,4.48200104659009));
#47037=CARTESIAN_POINT('Ctrl Pts',(18.3147508188514,-0.352485777302551,
4.34301457935691));
#47038=CARTESIAN_POINT('Ctrl Pts',(18.3624666549143,-0.479157019140895,
3.88903254594255));
#47039=CARTESIAN_POINT('Ctrl Pts',(18.4101824909771,-0.165810997523729,
3.5369536330429));
#47040=CARTESIAN_POINT('Ctrl Pts',(18.4578983270399,0.299801814449608,3.61009732380414));
#47041=CARTESIAN_POINT('Ctrl Pts',(18.5056141631028,0.49010200717001,4.04129464153984));
#47042=CARTESIAN_POINT('Ctrl Pts',(18.5533299991656,0.230333985517487,4.43457045454981));
#47043=CARTESIAN_POINT('Ctrl Pts',(18.6010458352284,-0.24095327917969,4.42877353242069));
#47044=CARTESIAN_POINT('Ctrl Pts',(18.6487616712913,-0.49096944006335,4.0292272779409));
#47045=CARTESIAN_POINT('Ctrl Pts',(18.6964775073541,-0.290120809601049,
3.60284116440841));
#47046=CARTESIAN_POINT('Ctrl Pts',(18.744193343417,0.177150224400508,3.54117212067402));
#47047=CARTESIAN_POINT('Ctrl Pts',(18.7919091794797,0.481741481528227,3.90085177849878));
#47048=CARTESIAN_POINT('Ctrl Pts',(18.8396250155427,0.343942123623612,4.35158077372017));
#47049=CARTESIAN_POINT('Ctrl Pts',(18.8873408516054,-0.109704578635382,
4.47944773466767));
#47050=CARTESIAN_POINT('Ctrl Pts',(18.9350566876684,-0.462607878309702,
4.16703046362027));
#47051=CARTESIAN_POINT('Ctrl Pts',(18.9827725237311,-0.39069124519864,3.70122654773242));
#47052=CARTESIAN_POINT('Ctrl Pts',(19.030488359794,0.0400031699426168,3.50979089028978));
#47053=CARTESIAN_POINT('Ctrl Pts',(19.0782041958568,0.433962058584907,3.76852180111673));
#47054=CARTESIAN_POINT('Ctrl Pts',(19.1259200319197,0.429406911488226,4.23982270375453));
#47055=CARTESIAN_POINT('Ctrl Pts',(19.1736358679825,0.0305207902517796,
4.49089072733801));
#47056=CARTESIAN_POINT('Ctrl Pts',(19.2213517040454,-0.396393042209671,
4.29116624277653));
#47057=CARTESIAN_POINT('Ctrl Pts',(19.2690675401082,-0.459293044881286,
3.82405931712685));
#47058=CARTESIAN_POINT('Ctrl Pts',(19.316783376171,-0.100417177000157,3.51852142809106));
#47059=CARTESIAN_POINT('Ctrl Pts',(19.3644992122339,0.350673329058588,3.65513271950473));
#47060=CARTESIAN_POINT('Ctrl Pts',(19.4122150482967,0.479735122332443,4.10844094226069));
#47061=CARTESIAN_POINT('Ctrl Pts',(19.4599308843596,0.168248769032157,4.46216617689766));
#47062=CARTESIAN_POINT('Ctrl Pts',(19.5076467204224,-0.297743013815871,
4.39147710422109));
#47063=CARTESIAN_POINT('Ctrl Pts',(19.5553625564852,-0.490312813065352,
3.96128857502183));
#47064=CARTESIAN_POINT('Ctrl Pts',(19.603078392548,-0.232620797759261,3.56664935826393));
#47065=CARTESIAN_POINT('Ctrl Pts',(19.6507942286109,0.238690449241969,3.56996267500769));
#47066=CARTESIAN_POINT('Ctrl Pts',(19.6985100646737,0.490808633485035,3.96818593857384));
#47067=CARTESIAN_POINT('Ctrl Pts',(19.7462259007366,0.292209604061002,4.39562444172689));
#47068=CARTESIAN_POINT('Ctrl Pts',(19.7939417367994,-0.174729824492781,
4.45975512619968));
#47069=CARTESIAN_POINT('Ctrl Pts',(19.8416575728622,-0.481212499922896,
4.10168523844358));
#47070=CARTESIAN_POINT('Ctrl Pts',(19.8893734089251,-0.345789702982467,
3.65023692191923));
#47071=CARTESIAN_POINT('Ctrl Pts',(19.9370892449879,0.107175910646637,3.51998011832295));
#47072=CARTESIAN_POINT('Ctrl Pts',(19.9848050810508,0.461722480014006,3.83053541934297));
#47073=CARTESIAN_POINT('Ctrl Pts',(20.0325209171136,0.392257955100357,4.29670800504879));
#47074=CARTESIAN_POINT('Ctrl Pts',(20.0802367531764,-0.0374150865130887,
4.49041783929577));
#47075=CARTESIAN_POINT('Ctrl Pts',(20.1279525892393,-0.432744382500041,
4.23375285658289));
#47076=CARTESIAN_POINT('Ctrl Pts',(20.1756684253021,-0.430649333670284,
3.76246031529274));
#47077=CARTESIAN_POINT('Ctrl Pts',(20.223384261365,-0.033136228617316,3.50924504180455));
#47078=CARTESIAN_POINT('Ctrl Pts',(20.2711000974278,0.394908089060633,3.70680919012016));
#47079=CARTESIAN_POINT('Ctrl Pts',(20.3188159334906,0.460110046434968,4.17340395051402));
#47080=CARTESIAN_POINT('Ctrl Pts',(20.3665317695535,0.103149962306437,4.48116018402389));
#47081=CARTESIAN_POINT('Ctrl Pts',(20.4142476056163,-0.34923165553999,4.34628168153608));
#47082=CARTESIAN_POINT('Ctrl Pts',(20.4540108023354,-0.457800032585507,
3.97025345815189));
#47083=CARTESIAN_POINT('Ctrl Pts',(20.4858213597105,-0.325993724402262,
3.71529210935379));
#47084=CARTESIAN_POINT('Ctrl Pts',(20.509679277742,-0.15096738523986,3.59329490328468));
#47085=CARTESIAN_POINT('Ctrl Pts',(20.5335371957734,0.0630371972956549,
3.57102347342756));
#47086=CARTESIAN_POINT('Ctrl Pts',(20.5573951138048,0.260511246441404,3.65349437971329));
#47087=CARTESIAN_POINT('Ctrl Pts',(20.5812530318362,0.394877283734959,3.82077798440408));
#47088=CARTESIAN_POINT('Ctrl Pts',(20.6051109498677,0.432370081305563,4.03184236506754));
#47089=CARTESIAN_POINT('Ctrl Pts',(20.6289688678991,0.364303478986858,4.23514367899931));
#47090=CARTESIAN_POINT('Ctrl Pts',(20.6528267859305,0.207066376217976,4.38093363836299));
#47091=CARTESIAN_POINT('Ctrl Pts',(20.6766847039619,-0.000757290757721993,
4.43358147160167));
#47092=CARTESIAN_POINT('Ctrl Pts',(20.7005426219933,-0.208420567790133,
4.38020336888205));
#47093=CARTESIAN_POINT('Ctrl Pts',(20.7244005400248,-0.365106210756856,
4.23385701605743));
#47094=CARTESIAN_POINT('Ctrl Pts',(20.7482584580562,-0.432520392530856,
4.03032528343114));
#47095=CARTESIAN_POINT('Ctrl Pts',(20.7721163760876,-0.394167874571092,
3.81937870627435));
#47096=CARTESIAN_POINT('Ctrl Pts',(20.795974294119,-0.259432524437891,3.65259868360638));
#47097=CARTESIAN_POINT('Ctrl Pts',(20.8198322121504,-0.0612578225112809,
3.57076788979259));
#47098=CARTESIAN_POINT('Ctrl Pts',(20.8436901301819,0.151895538690754,3.5938959627232));
#47099=CARTESIAN_POINT('Ctrl Pts',(20.8675480482132,0.327906592802717,3.71632757520176));
#47100=CARTESIAN_POINT('Ctrl Pts',(20.8914059662447,0.423735399567132,3.90812480123879));
#47101=CARTESIAN_POINT('Ctrl Pts',(20.9152638842761,0.415949440063929,4.12238802732943));
#47102=CARTESIAN_POINT('Ctrl Pts',(20.9391218023075,0.30645246920106,4.30672404095661));
#47103=CARTESIAN_POINT('Ctrl Pts',(20.962979720339,0.122019544809087,4.41605767475162));
#47104=CARTESIAN_POINT('Ctrl Pts',(20.9868376383703,-0.0922504941031022,
4.42365387220386));
#47105=CARTESIAN_POINT('Ctrl Pts',(21.0106955564018,-0.28396276796243,4.32765515869354));
#47106=CARTESIAN_POINT('Ctrl Pts',(21.0345534744332,-0.40623841344949,4.15153583326342));
#47107=CARTESIAN_POINT('Ctrl Pts',(21.0584113924646,-0.429177699343215,
3.93836186909709));
#47108=CARTESIAN_POINT('Ctrl Pts',(21.082269310496,-0.347171348131155,3.74026010679315));
#47109=CARTESIAN_POINT('Ctrl Pts',(21.1061272285274,-0.180272145040548,
3.605671823621));
#47110=CARTESIAN_POINT('Ctrl Pts',(21.1299851465589,0.0307085077608185,
3.56750752082027));
#47111=CARTESIAN_POINT('Ctrl Pts',(21.1538430645903,0.234180094072738,3.63509941005724));
#47112=CARTESIAN_POINT('Ctrl Pts',(21.1777009826217,0.380388268371489,3.79191943321731));
#47113=CARTESIAN_POINT('Ctrl Pts',(21.2015589006531,0.433581149524578,3.99962082296209));
#47114=CARTESIAN_POINT('Ctrl Pts',(21.2254168186846,0.380751629084578,4.2074149318183));
#47115=CARTESIAN_POINT('Ctrl Pts',(21.2492747367159,0.234817963878357,4.36449043997717));
#47116=CARTESIAN_POINT('Ctrl Pts',(21.2731326547474,0.0314649101850846,
4.43243810704058));
#47117=CARTESIAN_POINT('Ctrl Pts',(21.2969905727788,-0.179582171132277,
4.39464287755545));
#47118=CARTESIAN_POINT('Ctrl Pts',(21.3208484908102,-0.346716519889314,
4.26034671465164));
#47119=CARTESIAN_POINT('Ctrl Pts',(21.3447064088417,-0.429069235164158,
4.0623886883135));
#47120=CARTESIAN_POINT('Ctrl Pts',(21.368564326873,-0.406502834830527,3.8491749282489));
#47121=CARTESIAN_POINT('Ctrl Pts',(21.3924222449045,-0.284535418465691,
3.67284200661995));
#47122=CARTESIAN_POINT('Ctrl Pts',(21.4162801629359,-0.0929913416969399,
3.5765081259772));
#47123=CARTESIAN_POINT('Ctrl Pts',(21.4401380809674,0.121291651150069,3.58372954422009));
#47124=CARTESIAN_POINT('Ctrl Pts',(21.4639959989987,0.305915531372611,3.69274042788069));
#47125=CARTESIAN_POINT('Ctrl Pts',(21.4878539170302,0.415734731202803,3.87688464650718));
#47126=CARTESIAN_POINT('Ctrl Pts',(21.5117118350615,0.423895464867194,4.09113392265755));
#47127=CARTESIAN_POINT('Ctrl Pts',(21.535569753093,0.328402210690932,4.28309847227994));
#47128=CARTESIAN_POINT('Ctrl Pts',(21.5594276711244,0.152605670504114,4.40583773398234));
#47129=CARTESIAN_POINT('Ctrl Pts',(21.5832855891559,-0.0605071130159612,
4.42933861492812));
#47130=CARTESIAN_POINT('Ctrl Pts',(21.6071435071872,-0.258824259222961,
4.34785450957493));
#47131=CARTESIAN_POINT('Ctrl Pts',(21.6310014252187,-0.39385182381868,4.18131050126406));
#47132=CARTESIAN_POINT('Ctrl Pts',(21.6548593432501,-0.432571889182456,
3.97043113659525));
#47133=CARTESIAN_POINT('Ctrl Pts',(21.6787172612815,-0.365516344619441,
3.76678216446856));
#47134=CARTESIAN_POINT('Ctrl Pts',(21.702575179313,-0.209082097331647,3.62016130585559));
#47135=CARTESIAN_POINT('Ctrl Pts',(21.7264330973443,-0.00152158196427748,
3.56642135455923));
#47136=CARTESIAN_POINT('Ctrl Pts',(21.7502910153758,0.206411001640417,3.61870319251831));
#47137=CARTESIAN_POINT('Ctrl Pts',(21.7741489334072,0.363870472821225,3.76422248622317));
#47138=CARTESIAN_POINT('Ctrl Pts',(21.7980068514386,0.432353701764573,3.96739580449697));
#47139=CARTESIAN_POINT('Ctrl Pts',(21.82186476947,0.395114673548107,4.17854173669174));
#47140=CARTESIAN_POINT('Ctrl Pts',(21.8457226875014,0.261259344941517,4.3460293508861));
#47141=CARTESIAN_POINT('Ctrl Pts',(21.8695806055329,0.0635189899350569,
4.42890336313855));
#47142=CARTESIAN_POINT('Ctrl Pts',(21.8934385235643,-0.14975348833307,4.40689882001058));
#47143=CARTESIAN_POINT('Ctrl Pts',(21.9172964415957,-0.326407159500644,
4.28539643168872));
#47144=CARTESIAN_POINT('Ctrl Pts',(21.9411543596271,-0.423245389017799,
4.09410684177624));
#47145=CARTESIAN_POINT('Ctrl Pts',(21.9650122776585,-0.416588591947193,
3.87980556563057));
#47146=CARTESIAN_POINT('Ctrl Pts',(21.98887019569,-0.30806453650007,3.69489510271888));
#47147=CARTESIAN_POINT('Ctrl Pts',(22.0127281137213,-0.12421031036921,3.58459109808296));
#47148=CARTESIAN_POINT('Ctrl Pts',(22.0365860317528,0.0900167200678817,
3.57586588547707));
#47149=CARTESIAN_POINT('Ctrl Pts',(22.0604439497842,0.282232210442068,3.67085301705332));
#47150=CARTESIAN_POINT('Ctrl Pts',(22.0843018678157,0.405434237512275,3.8463255517439));
#47151=CARTESIAN_POINT('Ctrl Pts',(22.108159785847,0.429496549703537,4.05937567504088));
#47152=CARTESIAN_POINT('Ctrl Pts',(22.1320177038785,0.348535256241736,4.25790682842971));
#47153=CARTESIAN_POINT('Ctrl Pts',(22.1558756219099,0.182347598717988,4.39337273702606));
#47154=CARTESIAN_POINT('Ctrl Pts',(22.1797335399413,-0.0284290137391457,
4.43264829616218));
#47155=CARTESIAN_POINT('Ctrl Pts',(22.2035914579727,-0.232253957950086,
4.36612956178204));
#47156=CARTESIAN_POINT('Ctrl Pts',(22.2274493760041,-0.379286482964224,
4.21008217638027));
#47157=CARTESIAN_POINT('Ctrl Pts',(22.2513072940356,-0.433573131350875,
4.00266397632408));
#47158=CARTESIAN_POINT('Ctrl Pts',(22.275165212067,-0.381839338801546,3.79459436150246));
#47159=CARTESIAN_POINT('Ctrl Pts',(22.2990231300984,-0.236735426869051,
3.63675202040985));
#47160=CARTESIAN_POINT('Ctrl Pts',(22.3228810481298,-0.0337432544318164,
3.56773370504276));
#47161=CARTESIAN_POINT('Ctrl Pts',(22.3467389661613,0.177500062688638,3.60441627341574));
#47162=CARTESIAN_POINT('Ctrl Pts',(22.3705968841926,0.345339779804043,3.73782983856348));
#47163=CARTESIAN_POINT('Ctrl Pts',(22.3944548022241,0.428734513273282,3.93535114928888));
#47164=CARTESIAN_POINT('Ctrl Pts',(22.4183127202555,0.407291980919218,4.1486808655136));
#47165=CARTESIAN_POINT('Ctrl Pts',(22.4421706382869,0.286255462618544,4.32565405918856));
#47166=CARTESIAN_POINT('Ctrl Pts',(22.4660285563183,0.0952216904214238,
4.42299596654013));
#47167=CARTESIAN_POINT('Ctrl Pts',(22.4898864743497,-0.119096386717928,
4.41690383452019));
#47168=CARTESIAN_POINT('Ctrl Pts',(22.5137443923812,-0.304292138366774,
4.30886736509782));
#47169=CARTESIAN_POINT('Ctrl Pts',(22.5376023104126,-0.415080201412036,
4.12530439950267));
#47170=CARTESIAN_POINT('Ctrl Pts',(22.561460228444,-0.424369795825249,3.91110111771763));
#47171=CARTESIAN_POINT('Ctrl Pts',(22.5853181464754,-0.329889515310188,
3.71863599132299));
#47172=CARTESIAN_POINT('Ctrl Pts',(22.6091760645068,-0.154742073939436,
3.59497211022641));
#47173=CARTESIAN_POINT('Ctrl Pts',(22.6330339825383,0.0582436639512456,
3.57034842802071));
#47174=CARTESIAN_POINT('Ctrl Pts',(22.6568919005697,0.256987911016647,3.65078654733876));
#47175=CARTESIAN_POINT('Ctrl Pts',(22.6807498186011,0.39289034562191,3.81661632308649));
#47176=CARTESIAN_POINT('Ctrl Pts',(22.7046077366325,0.432722782933869,4.02728943245291));
#47177=CARTESIAN_POINT('Ctrl Pts',(22.7284656546639,0.366738191089385,4.2312875884069));
#47178=CARTESIAN_POINT('Ctrl Pts',(22.7523235726953,0.211084664509997,4.37873330099785));
#47179=CARTESIAN_POINT('Ctrl Pts',(22.7761814907268,0.00379901600965994,
4.43356145647204));
#47180=CARTESIAN_POINT('Ctrl Pts',(22.8000394087582,-0.204384723485633,
4.3823852668741));
#47181=CARTESIAN_POINT('Ctrl Pts',(22.8238973267896,-0.36265185203719,4.2376794731));
#47182=CARTESIAN_POINT('Ctrl Pts',(22.8398026054772,-0.408954280604672,
4.10250106973657));
#47183=CARTESIAN_POINT('Ctrl Pts',(22.847755244821,-0.414526965927561,4.03345758723954));
#47184=CARTESIAN_POINT('',(22.8,-0.592174260192535,4.04779597854866));
#47185=CARTESIAN_POINT('Ctrl Pts',(22.8,-0.19576256658266,4.36695865185836));
#47186=CARTESIAN_POINT('Ctrl Pts',(22.8,-0.195886593570853,4.36694806728808));
#47187=CARTESIAN_POINT('Ctrl Pts',(22.8,-0.196010613870461,4.36693742279878));
#47188=CARTESIAN_POINT('Ctrl Pts',(22.8,-0.196134627427637,4.36692671841166));
#47189=CARTESIAN_POINT('Ctrl Pts',(22.8,-0.216622178843513,4.36515830948628));
#47190=CARTESIAN_POINT('Ctrl Pts',(22.8,-0.236921239981942,4.36175743074964));
#47191=CARTESIAN_POINT('Ctrl Pts',(22.8,-0.256857422940798,4.35688458679081));
#47192=CARTESIAN_POINT('Ctrl Pts',(22.8,-0.271809560159941,4.35322995382169));
#47193=CARTESIAN_POINT('Ctrl Pts',(22.8,-0.286558947067823,4.34874691155445));
#47194=CARTESIAN_POINT('Ctrl Pts',(22.8,-0.301048271828705,4.34349077646485));
#47195=CARTESIAN_POINT('Ctrl Pts',(22.8,-0.310003423377303,4.3402422133286));
#47196=CARTESIAN_POINT('Ctrl Pts',(22.8,-0.318859482942331,4.33669811041118));
#47197=CARTESIAN_POINT('Ctrl Pts',(22.8,-0.327604744452034,4.33286912874946));
#47198=CARTESIAN_POINT('Ctrl Pts',(22.8,-0.333457186121174,4.33030672489195));
#47199=CARTESIAN_POINT('Ctrl Pts',(22.8,-0.33926207870774,4.32761569029118));
#47200=CARTESIAN_POINT('Ctrl Pts',(22.8,-0.345009487597299,4.32480202294401));
#47201=CARTESIAN_POINT('Ctrl Pts',(22.8,-0.365309066997251,4.31486428146495));
#47202=CARTESIAN_POINT('Ctrl Pts',(22.8,-0.384828901796994,4.30343044333042));
#47203=CARTESIAN_POINT('Ctrl Pts',(22.8,-0.403416958856431,4.29067119823496));
#47204=CARTESIAN_POINT('Ctrl Pts',(22.8,-0.409874425773003,4.28623865303559));
#47205=CARTESIAN_POINT('Ctrl Pts',(22.8,-0.416219739836017,4.28164578247975));
#47206=CARTESIAN_POINT('Ctrl Pts',(22.8,-0.422447327171508,4.27689854297234));
#47207=CARTESIAN_POINT('Ctrl Pts',(22.8,-0.43500295340691,4.2673274905416));
#47208=CARTESIAN_POINT('Ctrl Pts',(22.8,-0.447079966647781,4.25712966465555));
#47209=CARTESIAN_POINT('Ctrl Pts',(22.8,-0.458660056443695,4.24636133358853));
#47210=CARTESIAN_POINT('Ctrl Pts',(22.8,-0.465333929961841,4.24015529539631));
#47211=CARTESIAN_POINT('Ctrl Pts',(22.8,-0.471842796551704,4.23375955955572));
#47212=CARTESIAN_POINT('Ctrl Pts',(22.8,-0.478183280583292,4.22718326898633));
#47213=CARTESIAN_POINT('Ctrl Pts',(22.8,-0.48330469601013,4.22187138494));
#47214=CARTESIAN_POINT('Ctrl Pts',(22.8,-0.488310096860405,4.21644792156372));
#47215=CARTESIAN_POINT('Ctrl Pts',(22.8,-0.49319389770791,4.21092357737429));
#47216=CARTESIAN_POINT('Ctrl Pts',(22.8,-0.509882204568999,4.19204648678071));
#47217=CARTESIAN_POINT('Ctrl Pts',(22.8,-0.525164669297395,4.17198027236651));
#47218=CARTESIAN_POINT('Ctrl Pts',(22.8,-0.538985569877159,4.15095378743758));
#47219=CARTESIAN_POINT('Ctrl Pts',(22.8,-0.553292287721507,4.12918820238033));
#47220=CARTESIAN_POINT('Ctrl Pts',(22.8,-0.566034197593199,4.10639346234103));
#47221=CARTESIAN_POINT('Ctrl Pts',(22.8,-0.577149101532509,4.08276767497818));
#47222=CARTESIAN_POINT('Ctrl Pts',(22.8,-0.582543745751794,4.07130084468266));
#47223=CARTESIAN_POINT('Ctrl Pts',(22.8,-0.587554988912119,4.05963744408228));
#47224=CARTESIAN_POINT('Ctrl Pts',(22.8,-0.592174260192535,4.04779597854866));
#47225=CARTESIAN_POINT('Ctrl Pts',(22.8,-0.592174260192532,4.04779597854869));
#47226=CARTESIAN_POINT('Ctrl Pts',(22.7920473606562,-0.584213376873468,
4.14642833911734));
#47227=CARTESIAN_POINT('Ctrl Pts',(22.7840947213124,-0.551140611244481,
4.24298318064208));
#47228=CARTESIAN_POINT('Ctrl Pts',(22.7761420819686,-0.496922031827459,
4.32571394759471));
#47229=CARTESIAN_POINT('Ctrl Pts',(22.7681894426248,-0.442703452410443,
4.40844471454734));
#47230=CARTESIAN_POINT('Ctrl Pts',(22.760236803281,-0.367339059205388,4.47735140692785));
#47231=CARTESIAN_POINT('Ctrl Pts',(22.7522841639372,-0.280089901523161,
4.52398941366922));
#47232=CARTESIAN_POINT('Ctrl Pts',(22.7444712463773,-0.194373644734646,
4.56980802634291));
#47233=CARTESIAN_POINT('Ctrl Pts',(22.7366583288174,-0.0971865673270821,
4.59413356703531));
#47234=CARTESIAN_POINT('Ctrl Pts',(22.7288454112575,-7.11440487624268E-7,
4.59414971000239));
#47235=CARTESIAN_POINT('Origin',(27.2,0.3,2.9));
#47236=CARTESIAN_POINT('',(29.2,0.3,3.04606079858305));
#47237=CARTESIAN_POINT('',(27.2,0.3,3.04606079858305));
#47238=CARTESIAN_POINT('',(23.3,0.3,3.04606079858305));
#47239=CARTESIAN_POINT('',(29.2,0.3,3.35));
#47240=CARTESIAN_POINT('',(29.2,0.3,2.9));
#47241=CARTESIAN_POINT('',(27.2,0.3,3.35));
#47242=CARTESIAN_POINT('',(27.2,0.3,3.35));
#47243=CARTESIAN_POINT('',(27.2,0.3,2.9));
#47244=CARTESIAN_POINT('Origin',(27.2,0.,3.125));
#47245=CARTESIAN_POINT('',(27.2,-0.3,3.04606079858305));
#47246=CARTESIAN_POINT('Origin',(27.2,0.,4.));
#47247=CARTESIAN_POINT('',(27.2,-0.3,3.35));
#47248=CARTESIAN_POINT('',(27.2,0.3,3.35));
#47249=CARTESIAN_POINT('',(27.2,-0.3,3.35));
#47250=CARTESIAN_POINT('Origin',(27.2,0.3,3.35));
#47251=CARTESIAN_POINT('',(29.2,-0.3,3.35));
#47252=CARTESIAN_POINT('',(29.2,0.3,3.35));
#47253=CARTESIAN_POINT('',(27.2,-0.3,3.35));
#47254=CARTESIAN_POINT('Origin',(27.2,-0.3,3.35));
#47255=CARTESIAN_POINT('',(29.2,-0.3,3.04606079858305));
#47256=CARTESIAN_POINT('',(23.3,-0.3,3.04606079858305));
#47257=CARTESIAN_POINT('',(29.2,-0.3,3.35));
#47258=CARTESIAN_POINT('Origin',(29.2,0.,3.125));
#47259=CARTESIAN_POINT('Origin',(29.2,0.,4.));
#47260=CARTESIAN_POINT('Origin',(23.3,0.,4.));
#47261=CARTESIAN_POINT('',(29.4,-1.22464679914735E-16,5.));
#47262=CARTESIAN_POINT('Origin',(29.4,0.,4.));
#47263=CARTESIAN_POINT('',(23.3,-1.22464679914735E-16,5.));
#47264=CARTESIAN_POINT('',(23.3,-1.22464679914735E-16,5.));
#47265=CARTESIAN_POINT('Origin',(23.3,0.,4.));
#47266=CARTESIAN_POINT('Origin',(29.4,0.,4.));
#47267=CARTESIAN_POINT('Origin',(22.8,0.,4.));
#47268=CARTESIAN_POINT('',(22.8,-1.65327317884893E-16,5.35));
#47269=CARTESIAN_POINT('Origin',(22.8,0.,4.));
#47270=CARTESIAN_POINT('Origin',(22.8,0.,4.));
#47271=CARTESIAN_POINT('Origin',(22.8,0.,4.));
#47272=CARTESIAN_POINT('',(23.3,-1.65327317884893E-16,5.35));
#47273=CARTESIAN_POINT('Origin',(23.3,0.,4.));
#47274=CARTESIAN_POINT('',(22.8,-1.65327317884893E-16,5.35));
#47275=CARTESIAN_POINT('Origin',(23.3,0.,4.));
#47276=CARTESIAN_POINT('Origin',(4.,0.,4.));
#47277=CARTESIAN_POINT('',(0.,0.,0.));
#47278=CARTESIAN_POINT('Origin',(24.7,0.,4.));
#47279=CARTESIAN_POINT('',(25.4,-1.23689326713883E-16,5.01));
#47280=CARTESIAN_POINT('Origin',(25.4,0.,4.));
#47281=CARTESIAN_POINT('',(24.7,-1.23689326713883E-16,5.01));
#47282=CARTESIAN_POINT('',(24.7,-1.23689326713883E-16,5.01));
#47283=CARTESIAN_POINT('Origin',(24.7,0.,4.));
#47284=CARTESIAN_POINT('Origin',(24.7,0.,4.));
#47285=CARTESIAN_POINT('',(25.4,-1.65327317884893E-16,5.35));
#47286=CARTESIAN_POINT('Origin',(25.4,0.,4.));
#47287=CARTESIAN_POINT('',(24.7,-1.65327317884893E-16,5.35));
#47288=CARTESIAN_POINT('',(24.7,-1.65327317884893E-16,5.35));
#47289=CARTESIAN_POINT('Origin',(24.7,0.,4.));
#47290=CARTESIAN_POINT('Origin',(25.4,0.,4.));
#47291=CARTESIAN_POINT('Origin',(24.7,0.,4.));
#47292=CARTESIAN_POINT('',(0.,0.,0.));
#47293=CARTESIAN_POINT('Origin',(25.8,0.99,4.));
#47294=CARTESIAN_POINT('',(25.6809411910021,0.99,4.17298843892006));
#47295=CARTESIAN_POINT('',(25.9190588089979,0.99,4.17298843892006));
#47296=CARTESIAN_POINT('',(25.4,0.99,4.17298843892006));
#47297=CARTESIAN_POINT('Origin',(25.8,0.99,4.));
#47298=CARTESIAN_POINT('Origin',(25.8,0.99,4.));
#47299=CARTESIAN_POINT('',(25.6809411910021,0.99,3.82701156107994));
#47300=CARTESIAN_POINT('',(25.59,1.005,4.));
#47301=CARTESIAN_POINT('Ctrl Pts',(25.6809411910021,0.989999999999999,3.82701156107994));
#47302=CARTESIAN_POINT('Ctrl Pts',(25.6701985776047,0.99129192197638,3.83440513468868));
#47303=CARTESIAN_POINT('Ctrl Pts',(25.6603122906273,0.992653949439047,3.84270286127439));
#47304=CARTESIAN_POINT('Ctrl Pts',(25.6329072257467,0.996748084390898,3.87010792615492));
#47305=CARTESIAN_POINT('Ctrl Pts',(25.6167579436671,0.999695893276376,3.89366983224072));
#47306=CARTESIAN_POINT('Ctrl Pts',(25.5953022060351,1.00385029472357,3.94538709536759));
#47307=CARTESIAN_POINT('Ctrl Pts',(25.59,1.005,3.97354876917015));
#47308=CARTESIAN_POINT('Ctrl Pts',(25.59,1.005,4.));
#47309=CARTESIAN_POINT('',(25.9190588089979,0.99,3.82701156107994));
#47310=CARTESIAN_POINT('Origin',(25.8,0.99,4.));
#47311=CARTESIAN_POINT('Ctrl Pts',(25.9190588089979,0.99,4.17298843892006));
#47312=CARTESIAN_POINT('Ctrl Pts',(25.9298014223953,0.991291921976381,4.16559486531132));
#47313=CARTESIAN_POINT('Ctrl Pts',(25.9396877093727,0.992653949439047,4.15729713872561));
#47314=CARTESIAN_POINT('Ctrl Pts',(25.9670927742533,0.996748084390898,4.12989207384508));
#47315=CARTESIAN_POINT('Ctrl Pts',(25.9832420563329,0.999695893276376,4.10633016775929));
#47316=CARTESIAN_POINT('Ctrl Pts',(26.0046977939649,1.00385029472357,4.05461290463241));
#47317=CARTESIAN_POINT('Ctrl Pts',(26.01,1.005,4.02645123082985));
#47318=CARTESIAN_POINT('Ctrl Pts',(26.01,1.005,3.97354876917015));
#47319=CARTESIAN_POINT('Ctrl Pts',(26.0046977939649,1.00385029472357,3.94538709536759));
#47320=CARTESIAN_POINT('Ctrl Pts',(25.9832420563329,0.999695893276376,3.89366983224072));
#47321=CARTESIAN_POINT('Ctrl Pts',(25.9670927742533,0.996748084390898,3.87010792615492));
#47322=CARTESIAN_POINT('Ctrl Pts',(25.9396877093727,0.992653949439047,3.84270286127439));
#47323=CARTESIAN_POINT('Ctrl Pts',(25.9298014223953,0.991291921976381,3.83440513468868));
#47324=CARTESIAN_POINT('Ctrl Pts',(25.9190588089979,0.99,3.82701156107994));
#47325=CARTESIAN_POINT('Ctrl Pts',(25.59,1.005,4.));
#47326=CARTESIAN_POINT('Ctrl Pts',(25.59,1.005,4.02645123082985));
#47327=CARTESIAN_POINT('Ctrl Pts',(25.5953022060351,1.00385029472357,4.05461290463241));
#47328=CARTESIAN_POINT('Ctrl Pts',(25.6167579436671,0.999695893276376,4.10633016775929));
#47329=CARTESIAN_POINT('Ctrl Pts',(25.6329072257467,0.996748084390898,4.12989207384508));
#47330=CARTESIAN_POINT('Ctrl Pts',(25.6603122906273,0.992653949439047,4.15729713872561));
#47331=CARTESIAN_POINT('Ctrl Pts',(25.6701985776047,0.991291921976381,4.16559486531132));
#47332=CARTESIAN_POINT('Ctrl Pts',(25.6809411910021,0.99,4.17298843892006));
#47333=CARTESIAN_POINT('',(25.59,1.5,4.));
#47334=CARTESIAN_POINT('',(25.59,0.99,4.));
#47335=CARTESIAN_POINT('',(25.8,1.48522725533839,4.21));
#47336=CARTESIAN_POINT('Ctrl Pts',(25.8,1.48522725533839,4.21));
#47337=CARTESIAN_POINT('Ctrl Pts',(25.7735944730755,1.48522725533839,4.21));
#47338=CARTESIAN_POINT('Ctrl Pts',(25.7454529259093,1.48600415954412,4.2047157372696));
#47339=CARTESIAN_POINT('Ctrl Pts',(25.6937237310949,1.48880073282317,4.18327376303633));
#47340=CARTESIAN_POINT('Ctrl Pts',(25.670133075872,1.49077897157582,4.16711792397039));
#47341=CARTESIAN_POINT('Ctrl Pts',(25.632882321789,1.49448481141327,4.12986716988737));
#47342=CARTESIAN_POINT('Ctrl Pts',(25.6167262899986,1.49645455657129,4.10627640830577));
#47343=CARTESIAN_POINT('Ctrl Pts',(25.5952841751738,1.49923165515646,4.0545468514059));
#47344=CARTESIAN_POINT('Ctrl Pts',(25.59,1.5,4.02640517850928));
#47345=CARTESIAN_POINT('Ctrl Pts',(25.59,1.5,4.));
#47346=CARTESIAN_POINT('Ctrl Pts',(25.59,1.5,4.));
#47347=CARTESIAN_POINT('Ctrl Pts',(25.59,1.5,3.97359482149072));
#47348=CARTESIAN_POINT('Ctrl Pts',(25.5952841751738,1.49923165515646,3.9454531485941));
#47349=CARTESIAN_POINT('Ctrl Pts',(25.6167262899986,1.49645455657129,3.89372359169423));
#47350=CARTESIAN_POINT('Ctrl Pts',(25.632882321789,1.49448481141327,3.87013283011263));
#47351=CARTESIAN_POINT('Ctrl Pts',(25.670133075872,1.49077897157582,3.83288207602961));
#47352=CARTESIAN_POINT('Ctrl Pts',(25.6937237310949,1.48880073282317,3.81672623696366));
#47353=CARTESIAN_POINT('Ctrl Pts',(25.7454529259093,1.48600415954412,3.7952842627304));
#47354=CARTESIAN_POINT('Ctrl Pts',(25.7735944730755,1.48522725533839,3.79));
#47355=CARTESIAN_POINT('Ctrl Pts',(25.8264055269245,1.48522725533839,3.79));
#47356=CARTESIAN_POINT('Ctrl Pts',(25.8545470740907,1.48600415954412,3.7952842627304));
#47357=CARTESIAN_POINT('Ctrl Pts',(25.9062762689051,1.48880073282317,3.81672623696367));
#47358=CARTESIAN_POINT('Ctrl Pts',(25.929866924128,1.49077897157582,3.83288207602961));
#47359=CARTESIAN_POINT('Ctrl Pts',(25.967117678211,1.49448481141327,3.87013283011263));
#47360=CARTESIAN_POINT('Ctrl Pts',(25.9832737100014,1.49645455657129,3.89372359169423));
#47361=CARTESIAN_POINT('Ctrl Pts',(26.0047158248262,1.49923165515646,3.9454531485941));
#47362=CARTESIAN_POINT('Ctrl Pts',(26.01,1.5,3.97359482149072));
#47363=CARTESIAN_POINT('Ctrl Pts',(26.01,1.5,4.02640517850928));
#47364=CARTESIAN_POINT('Ctrl Pts',(26.0047158248262,1.49923165515646,4.0545468514059));
#47365=CARTESIAN_POINT('Ctrl Pts',(25.9832737100014,1.49645455657129,4.10627640830577));
#47366=CARTESIAN_POINT('Ctrl Pts',(25.967117678211,1.49448481141327,4.12986716988737));
#47367=CARTESIAN_POINT('Ctrl Pts',(25.929866924128,1.49077897157582,4.16711792397039));
#47368=CARTESIAN_POINT('Ctrl Pts',(25.9062762689051,1.48880073282317,4.18327376303633));
#47369=CARTESIAN_POINT('Ctrl Pts',(25.8545470740907,1.48600415954412,4.20471573726959));
#47370=CARTESIAN_POINT('Ctrl Pts',(25.8264055269245,1.48522725533839,4.21));
#47371=CARTESIAN_POINT('Ctrl Pts',(25.8,1.48522725533839,4.21));
#47372=CARTESIAN_POINT('Origin',(25.8,0.99,4.));
#47373=CARTESIAN_POINT('',(25.4,0.99,3.82701156107994));
#47374=CARTESIAN_POINT('Origin',(25.4,0.,4.));
#47375=CARTESIAN_POINT('',(26.2,-1.23077003314309E-16,5.005));
#47376=CARTESIAN_POINT('Origin',(26.2,0.,4.));
#47377=CARTESIAN_POINT('',(25.4,-1.23077003314309E-16,5.005));
#47378=CARTESIAN_POINT('',(25.4,-1.23077003314309E-16,5.005));
#47379=CARTESIAN_POINT('Origin',(25.4,0.,4.));
#47380=CARTESIAN_POINT('Origin',(25.4,0.,4.));
#47381=CARTESIAN_POINT('',(26.2,-1.83697019872103E-16,5.5));
#47382=CARTESIAN_POINT('Origin',(26.2,0.,4.));
#47383=CARTESIAN_POINT('',(25.4,-1.83697019872103E-16,5.5));
#47384=CARTESIAN_POINT('',(25.4,-1.83697019872103E-16,5.5));
#47385=CARTESIAN_POINT('Origin',(25.4,0.,4.));
#47386=CARTESIAN_POINT('Origin',(26.2,0.,4.));
#47387=CARTESIAN_POINT('Origin',(25.4,0.,4.));
#47388=CARTESIAN_POINT('',(0.,0.,0.));
#47389=CARTESIAN_POINT('Origin',(28.7,0.,6.5));
#47390=CARTESIAN_POINT('',(28.8,-3.06161699786838E-17,6.75));
#47391=CARTESIAN_POINT('Origin',(28.8,0.,6.5));
#47392=CARTESIAN_POINT('',(29.4,3.06161699786838E-17,6.75));
#47393=CARTESIAN_POINT('',(28.7,-3.06161699786838E-17,6.75));
#47394=CARTESIAN_POINT('Origin',(29.4,0.,6.5));
#47395=CARTESIAN_POINT('Origin',(28.,0.99,4.));
#47396=CARTESIAN_POINT('',(27.844436508139,0.99,4.14106735979666));
#47397=CARTESIAN_POINT('',(28.155563491861,0.99,4.14106735979666));
#47398=CARTESIAN_POINT('',(27.,0.99,4.14106735979666));
#47399=CARTESIAN_POINT('Origin',(28.,0.99,4.));
#47400=CARTESIAN_POINT('Origin',(28.,0.99,4.));
#47401=CARTESIAN_POINT('',(27.844436508139,0.99,3.85893264020334));
#47402=CARTESIAN_POINT('',(27.79,1.,4.));
#47403=CARTESIAN_POINT('Ctrl Pts',(27.844436508139,0.99,3.85893264020334));
#47404=CARTESIAN_POINT('Ctrl Pts',(27.8287948476368,0.992457849824465,3.87618164330178));
#47405=CARTESIAN_POINT('Ctrl Pts',(27.815375956669,0.994938193049464,3.8970013568903));
#47406=CARTESIAN_POINT('Ctrl Pts',(27.7953025362756,0.998844492372413,3.94538588560165));
#47407=CARTESIAN_POINT('Ctrl Pts',(27.79,1.,3.97354792631755));
#47408=CARTESIAN_POINT('Ctrl Pts',(27.79,1.,4.));
#47409=CARTESIAN_POINT('',(28.155563491861,0.99,3.85893264020334));
#47410=CARTESIAN_POINT('Origin',(28.,0.99,4.));
#47411=CARTESIAN_POINT('Ctrl Pts',(28.155563491861,0.99,4.14106735979666));
#47412=CARTESIAN_POINT('Ctrl Pts',(28.1712051523632,0.992457849824465,4.12381835669823));
#47413=CARTESIAN_POINT('Ctrl Pts',(28.184624043331,0.994938193049464,4.1029986431097));
#47414=CARTESIAN_POINT('Ctrl Pts',(28.2046974637244,0.998844492372413,4.05461411439835));
#47415=CARTESIAN_POINT('Ctrl Pts',(28.21,1.,4.02645207368245));
#47416=CARTESIAN_POINT('Ctrl Pts',(28.21,1.,3.97354792631755));
#47417=CARTESIAN_POINT('Ctrl Pts',(28.2046974637244,0.998844492372413,3.94538588560165));
#47418=CARTESIAN_POINT('Ctrl Pts',(28.184624043331,0.994938193049464,3.8970013568903));
#47419=CARTESIAN_POINT('Ctrl Pts',(28.1712051523632,0.992457849824465,3.87618164330178));
#47420=CARTESIAN_POINT('Ctrl Pts',(28.155563491861,0.99,3.85893264020334));
#47421=CARTESIAN_POINT('Ctrl Pts',(27.79,1.,4.));
#47422=CARTESIAN_POINT('Ctrl Pts',(27.79,1.,4.02645207368245));
#47423=CARTESIAN_POINT('Ctrl Pts',(27.7953025362756,0.998844492372413,4.05461411439835));
#47424=CARTESIAN_POINT('Ctrl Pts',(27.815375956669,0.994938193049464,4.1029986431097));
#47425=CARTESIAN_POINT('Ctrl Pts',(27.8287948476368,0.992457849824465,4.12381835669823));
#47426=CARTESIAN_POINT('Ctrl Pts',(27.844436508139,0.99,4.14106735979666));
#47427=CARTESIAN_POINT('',(27.79,1.5,4.));
#47428=CARTESIAN_POINT('',(27.79,0.99,4.));
#47429=CARTESIAN_POINT('',(28.,1.48522725533839,4.21));
#47430=CARTESIAN_POINT('Ctrl Pts',(28.,1.48522725533839,4.21));
#47431=CARTESIAN_POINT('Ctrl Pts',(27.9735944730755,1.48522725533839,4.21));
#47432=CARTESIAN_POINT('Ctrl Pts',(27.9454529259093,1.48600415954412,4.20471573726959));
#47433=CARTESIAN_POINT('Ctrl Pts',(27.8937237310949,1.48880073282317,4.18327376303633));
#47434=CARTESIAN_POINT('Ctrl Pts',(27.870133075872,1.49077897157582,4.16711792397039));
#47435=CARTESIAN_POINT('Ctrl Pts',(27.832882321789,1.49448481141327,4.12986716988737));
#47436=CARTESIAN_POINT('Ctrl Pts',(27.8167262899986,1.49645455657129,4.10627640830576));
#47437=CARTESIAN_POINT('Ctrl Pts',(27.7952841751738,1.49923165515646,4.0545468514059));
#47438=CARTESIAN_POINT('Ctrl Pts',(27.79,1.5,4.02640517850928));
#47439=CARTESIAN_POINT('Ctrl Pts',(27.79,1.5,4.));
#47440=CARTESIAN_POINT('Ctrl Pts',(27.79,1.5,4.));
#47441=CARTESIAN_POINT('Ctrl Pts',(27.79,1.5,3.97359482149072));
#47442=CARTESIAN_POINT('Ctrl Pts',(27.7952841751738,1.49923165515646,3.9454531485941));
#47443=CARTESIAN_POINT('Ctrl Pts',(27.8167262899986,1.49645455657129,3.89372359169424));
#47444=CARTESIAN_POINT('Ctrl Pts',(27.832882321789,1.49448481141327,3.87013283011263));
#47445=CARTESIAN_POINT('Ctrl Pts',(27.870133075872,1.49077897157582,3.83288207602961));
#47446=CARTESIAN_POINT('Ctrl Pts',(27.8937237310949,1.48880073282317,3.81672623696367));
#47447=CARTESIAN_POINT('Ctrl Pts',(27.9454529259093,1.48600415954412,3.7952842627304));
#47448=CARTESIAN_POINT('Ctrl Pts',(27.9735944730755,1.48522725533839,3.79));
#47449=CARTESIAN_POINT('Ctrl Pts',(28.0264055269245,1.48522725533839,3.79));
#47450=CARTESIAN_POINT('Ctrl Pts',(28.0545470740907,1.48600415954412,3.7952842627304));
#47451=CARTESIAN_POINT('Ctrl Pts',(28.1062762689051,1.48880073282317,3.81672623696367));
#47452=CARTESIAN_POINT('Ctrl Pts',(28.129866924128,1.49077897157582,3.83288207602961));
#47453=CARTESIAN_POINT('Ctrl Pts',(28.167117678211,1.49448481141327,3.87013283011263));
#47454=CARTESIAN_POINT('Ctrl Pts',(28.1832737100014,1.49645455657129,3.89372359169424));
#47455=CARTESIAN_POINT('Ctrl Pts',(28.2047158248262,1.49923165515646,3.9454531485941));
#47456=CARTESIAN_POINT('Ctrl Pts',(28.21,1.5,3.97359482149072));
#47457=CARTESIAN_POINT('Ctrl Pts',(28.21,1.5,4.02640517850928));
#47458=CARTESIAN_POINT('Ctrl Pts',(28.2047158248262,1.49923165515646,4.0545468514059));
#47459=CARTESIAN_POINT('Ctrl Pts',(28.1832737100014,1.49645455657129,4.10627640830576));
#47460=CARTESIAN_POINT('Ctrl Pts',(28.167117678211,1.49448481141327,4.12986716988737));
#47461=CARTESIAN_POINT('Ctrl Pts',(28.129866924128,1.49077897157582,4.16711792397039));
#47462=CARTESIAN_POINT('Ctrl Pts',(28.1062762689051,1.48880073282317,4.18327376303633));
#47463=CARTESIAN_POINT('Ctrl Pts',(28.0545470740907,1.48600415954412,4.2047157372696));
#47464=CARTESIAN_POINT('Ctrl Pts',(28.0264055269245,1.48522725533839,4.21));
#47465=CARTESIAN_POINT('Ctrl Pts',(28.,1.48522725533839,4.21));
#47466=CARTESIAN_POINT('Origin',(28.,0.99,4.));
#47467=CARTESIAN_POINT('',(27.,0.99,3.85893264020334));
#47468=CARTESIAN_POINT('Origin',(26.9,-0.3,4.));
#47469=CARTESIAN_POINT('',(29.4,-0.3,2.5));
#47470=CARTESIAN_POINT('',(29.4,-0.3,3.04606079858305));
#47471=CARTESIAN_POINT('',(29.4,-0.3,4.));
#47472=CARTESIAN_POINT('',(28.8,-0.3,2.5));
#47473=CARTESIAN_POINT('',(26.9,-0.3,2.5));
#47474=CARTESIAN_POINT('',(28.8,-0.3,2.53030615433009));
#47475=CARTESIAN_POINT('',(28.8,-0.3,4.));
#47476=CARTESIAN_POINT('',(27.,-0.3,2.53030615433009));
#47477=CARTESIAN_POINT('',(27.,-0.3,2.53030615433009));
#47478=CARTESIAN_POINT('',(27.,-0.3,3.04606079858305));
#47479=CARTESIAN_POINT('',(27.,-0.3,4.));
#47480=CARTESIAN_POINT('',(27.,-0.3,3.04606079858305));
#47481=CARTESIAN_POINT('Origin',(26.9,-0.3,2.5));
#47482=CARTESIAN_POINT('',(29.4,0.3,2.5));
#47483=CARTESIAN_POINT('',(29.4,-0.15,2.5));
#47484=CARTESIAN_POINT('',(28.8,0.3,2.5));
#47485=CARTESIAN_POINT('',(26.9,0.3,2.5));
#47486=CARTESIAN_POINT('',(28.8,-0.15,2.5));
#47487=CARTESIAN_POINT('Origin',(26.9,0.3,2.5));
#47488=CARTESIAN_POINT('',(29.4,0.3,3.04606079858305));
#47489=CARTESIAN_POINT('',(29.4,0.3,3.25));
#47490=CARTESIAN_POINT('',(27.,0.3,3.04606079858305));
#47491=CARTESIAN_POINT('',(27.,0.3,3.04606079858305));
#47492=CARTESIAN_POINT('',(27.,0.3,2.53030615433009));
#47493=CARTESIAN_POINT('',(27.,0.3,3.25));
#47494=CARTESIAN_POINT('',(28.8,0.3,2.53030615433009));
#47495=CARTESIAN_POINT('',(27.,0.3,2.53030615433009));
#47496=CARTESIAN_POINT('',(28.8,0.3,3.25));
#47497=CARTESIAN_POINT('Origin',(29.4,0.,4.));
#47498=CARTESIAN_POINT('',(29.4,-4.28626379701574E-16,7.5));
#47499=CARTESIAN_POINT('Origin',(29.4,0.,4.));
#47500=CARTESIAN_POINT('Origin',(29.4,0.,4.));
#47501=CARTESIAN_POINT('Origin',(28.8,0.,4.));
#47502=CARTESIAN_POINT('',(28.8,-4.28626379701574E-16,7.5));
#47503=CARTESIAN_POINT('Origin',(28.8,0.,4.));
#47504=CARTESIAN_POINT('Origin',(28.8,0.,4.));
#47505=CARTESIAN_POINT('Origin',(28.8,0.,4.));
#47506=CARTESIAN_POINT('',(28.8,-4.28626379701574E-16,7.5));
#47507=CARTESIAN_POINT('Origin',(27.,0.,4.));
#47508=CARTESIAN_POINT('Origin',(27.,0.,4.));
#47509=CARTESIAN_POINT('Origin',(27.,0.,4.));
#47510=CARTESIAN_POINT('Origin',(27.,0.,4.));
#47511=CARTESIAN_POINT('Origin',(27.,0.,4.));
#47512=CARTESIAN_POINT('',(0.,0.,0.));
#47513=CARTESIAN_POINT('Origin',(29.4,0.,6.5));
#47514=CARTESIAN_POINT('',(31.03,-4.04133443718627E-17,6.83));
#47515=CARTESIAN_POINT('Origin',(31.03,0.,6.5));
#47516=CARTESIAN_POINT('',(29.4,-4.04133443718627E-17,6.83));
#47517=CARTESIAN_POINT('',(29.4,-4.04133443718627E-17,6.83));
#47518=CARTESIAN_POINT('Origin',(29.4,0.,6.5));
#47519=CARTESIAN_POINT('Origin',(29.4,0.,6.5));
#47520=CARTESIAN_POINT('',(31.03,-4.89858719658942E-17,6.9));
#47521=CARTESIAN_POINT('Origin',(31.03,0.,6.5));
#47522=CARTESIAN_POINT('',(29.4,-4.89858719658942E-17,6.9));
#47523=CARTESIAN_POINT('',(29.4,-4.89858719658942E-17,6.9));
#47524=CARTESIAN_POINT('Origin',(29.4,0.,6.5));
#47525=CARTESIAN_POINT('Origin',(31.03,0.,6.5));
#47526=CARTESIAN_POINT('Origin',(29.4,0.,6.5));
#47527=CARTESIAN_POINT('',(0.,0.,0.));
#47528=CARTESIAN_POINT('Origin',(29.4,0.,6.5));
#47529=CARTESIAN_POINT('',(31.,-4.95981953654678E-17,6.905));
#47530=CARTESIAN_POINT('Origin',(31.,0.,6.5));
#47531=CARTESIAN_POINT('',(29.4,-4.95981953654678E-17,6.905));
#47532=CARTESIAN_POINT('',(29.4,-4.95981953654678E-17,6.905));
#47533=CARTESIAN_POINT('Origin',(29.4,0.,6.5));
#47534=CARTESIAN_POINT('Origin',(29.4,0.,6.5));
#47535=CARTESIAN_POINT('',(31.,-1.10218211923262E-16,7.4));
#47536=CARTESIAN_POINT('Origin',(31.,0.,6.5));
#47537=CARTESIAN_POINT('',(29.4,-1.10218211923262E-16,7.4));
#47538=CARTESIAN_POINT('',(29.4,-1.10218211923262E-16,7.4));
#47539=CARTESIAN_POINT('Origin',(29.4,0.,6.5));
#47540=CARTESIAN_POINT('Origin',(31.,0.,6.5));
#47541=CARTESIAN_POINT('Origin',(29.4,0.,6.5));
#47542=CARTESIAN_POINT('',(0.,0.,0.));
#47543=CARTESIAN_POINT('Origin',(-1.,0.,0.35));
#47544=CARTESIAN_POINT('',(-1.,-0.26,0.6));
#47545=CARTESIAN_POINT('',(-1.,-0.3,0.56));
#47546=CARTESIAN_POINT('',(-1.,-0.2675,0.5925));
#47547=CARTESIAN_POINT('',(-1.,0.26,0.6));
#47548=CARTESIAN_POINT('',(-1.,0.,0.6));
#47549=CARTESIAN_POINT('',(-1.,0.3,0.56));
#47550=CARTESIAN_POINT('',(-1.,0.2675,0.5925));
#47551=CARTESIAN_POINT('',(-1.,0.3,0.04));
#47552=CARTESIAN_POINT('',(-1.,0.3,0.175));
#47553=CARTESIAN_POINT('',(-1.,0.26,0.));
#47554=CARTESIAN_POINT('',(-1.,0.2925,0.0325));
#47555=CARTESIAN_POINT('',(-1.,-0.26,0.));
#47556=CARTESIAN_POINT('',(-1.,0.,0.));
#47557=CARTESIAN_POINT('',(-1.,-0.3,0.04));
#47558=CARTESIAN_POINT('',(-1.,-0.2925,0.0325));
#47559=CARTESIAN_POINT('',(-1.,-0.3,0.175));
#47560=CARTESIAN_POINT('Origin',(0.75,0.28,0.02));
#47561=CARTESIAN_POINT('',(1.,0.3,0.04));
#47562=CARTESIAN_POINT('',(0.75,0.3,0.04));
#47563=CARTESIAN_POINT('',(1.,0.26,0.));
#47564=CARTESIAN_POINT('',(1.,0.2925,0.0325));
#47565=CARTESIAN_POINT('',(0.75,0.26,0.));
#47566=CARTESIAN_POINT('Origin',(1.5,0.3,0.));
#47567=CARTESIAN_POINT('',(1.,0.3,0.56));
#47568=CARTESIAN_POINT('',(0.75,0.3,0.56));
#47569=CARTESIAN_POINT('',(1.,0.3,0.175));
#47570=CARTESIAN_POINT('Origin',(0.75,0.28,0.58));
#47571=CARTESIAN_POINT('',(1.,0.26,0.6));
#47572=CARTESIAN_POINT('',(0.75,0.26,0.6));
#47573=CARTESIAN_POINT('',(1.,0.2675,0.5925));
#47574=CARTESIAN_POINT('Origin',(0.,0.,0.6));
#47575=CARTESIAN_POINT('',(1.,-0.26,0.6));
#47576=CARTESIAN_POINT('',(-0.75,-0.26,0.6));
#47577=CARTESIAN_POINT('',(1.,0.,0.6));
#47578=CARTESIAN_POINT('Origin',(1.,0.,0.35));
#47579=CARTESIAN_POINT('',(1.,-0.26,0.));
#47580=CARTESIAN_POINT('',(1.,-0.3,0.04));
#47581=CARTESIAN_POINT('',(1.,-0.2925,0.0325));
#47582=CARTESIAN_POINT('',(1.,0.,0.));
#47583=CARTESIAN_POINT('',(1.,-0.3,0.56));
#47584=CARTESIAN_POINT('',(1.,-0.2675,0.5925));
#47585=CARTESIAN_POINT('',(1.,-0.3,0.175));
#47586=CARTESIAN_POINT('Origin',(0.,0.,0.));
#47587=CARTESIAN_POINT('',(-0.75,-0.26,0.));
#47588=CARTESIAN_POINT('Origin',(-0.75,-0.28,0.58));
#47589=CARTESIAN_POINT('',(-0.75,-0.3,0.56));
#47590=CARTESIAN_POINT('Origin',(-0.75,-0.28,0.02));
#47591=CARTESIAN_POINT('',(-0.75,-0.3,0.04));
#47592=CARTESIAN_POINT('Origin',(-1.5,-0.3,0.));
#47593=CARTESIAN_POINT('',(0.,0.,0.));
#47594=CARTESIAN_POINT('Origin',(0.0721687836487032,0.,-0.125));
#47595=CARTESIAN_POINT('',(0.0721687836487032,0.,-0.125));
#47596=CARTESIAN_POINT('',(0.144337567297406,0.,0.));
#47597=CARTESIAN_POINT('',(0.117710979560879,0.,-0.0461186027918559));
#47598=CARTESIAN_POINT('',(0.0721687836487032,-0.25,-0.125));
#47599=CARTESIAN_POINT('',(0.0721687836487032,0.,-0.125));
#47600=CARTESIAN_POINT('',(0.144337567297406,-0.25,0.));
#47601=CARTESIAN_POINT('',(0.144337567297406,-0.25,0.));
#47602=CARTESIAN_POINT('',(0.144337567297406,0.,0.));
#47603=CARTESIAN_POINT('Origin',(-0.0721687836487032,0.,-0.125));
#47604=CARTESIAN_POINT('',(-0.0721687836487032,0.,-0.125));
#47605=CARTESIAN_POINT('',(0.0739156081756484,0.,-0.125));
#47606=CARTESIAN_POINT('',(-0.0721687836487032,-0.25,-0.125));
#47607=CARTESIAN_POINT('',(-0.0721687836487032,0.,-0.125));
#47608=CARTESIAN_POINT('',(0.0721687836487032,-0.25,-0.125));
#47609=CARTESIAN_POINT('Origin',(-0.144337567297406,0.,-4.16333634234434E-17));
#47610=CARTESIAN_POINT('',(-0.144337567297406,0.,-1.76762539787485E-17));
#47611=CARTESIAN_POINT('',(-0.0987953713852306,0.,-0.0788813972081442));
#47612=CARTESIAN_POINT('',(-0.144337567297406,-0.25,-2.77555756156289E-17));
#47613=CARTESIAN_POINT('',(-0.144337567297406,0.,-1.76762539787485E-17));
#47614=CARTESIAN_POINT('',(-0.0721687836487032,-0.25,-0.125));
#47615=CARTESIAN_POINT('Origin',(-0.0721687836487033,0.,0.125));
#47616=CARTESIAN_POINT('',(-0.0721687836487033,0.,0.125));
#47617=CARTESIAN_POINT('',(-0.0627109795608791,0.,0.141381397208144));
#47618=CARTESIAN_POINT('',(-0.0721687836487033,-0.25,0.125));
#47619=CARTESIAN_POINT('',(-0.0721687836487033,0.,0.125));
#47620=CARTESIAN_POINT('',(-0.144337567297406,-0.25,-1.76762539787485E-17));
#47621=CARTESIAN_POINT('Origin',(0.0721687836487032,0.,0.125));
#47622=CARTESIAN_POINT('',(0.0721687836487032,0.,0.125));
#47623=CARTESIAN_POINT('',(0.146084391824352,0.,0.125));
#47624=CARTESIAN_POINT('',(0.0721687836487032,-0.25,0.125));
#47625=CARTESIAN_POINT('',(0.0721687836487032,0.,0.125));
#47626=CARTESIAN_POINT('',(-0.0721687836487033,-0.25,0.125));
#47627=CARTESIAN_POINT('Origin',(0.144337567297406,0.,0.));
#47628=CARTESIAN_POINT('',(0.153795371385231,0.,-0.0163813972081441));
#47629=CARTESIAN_POINT('',(0.0721687836487032,-0.25,0.125));
#47630=CARTESIAN_POINT('Origin',(0.,-0.25,0.));
#47631=CARTESIAN_POINT('Origin',(0.22,0.,0.));
#47632=CARTESIAN_POINT('',(-0.22,-8.67361737988404E-18,-2.69422295812418E-17));
#47633=CARTESIAN_POINT('Origin',(0.,0.,0.));
#47634=CARTESIAN_POINT('Origin',(0.,-0.015,0.));
#47635=CARTESIAN_POINT('',(-0.24505,-0.02505,-3.00099698131059E-17));
#47636=CARTESIAN_POINT('Origin',(0.,-0.02505,0.));
#47637=CARTESIAN_POINT('',(-0.235,-0.015,-2.87791997799628E-17));
#47638=CARTESIAN_POINT('Origin',(0.,-0.3775,0.));
#47639=CARTESIAN_POINT('',(-0.24505,-0.72995,3.00099698131059E-17));
#47640=CARTESIAN_POINT('Origin',(0.,-0.72995,0.));
#47641=CARTESIAN_POINT('',(-0.24505,-0.3775,-3.00099698131059E-17));
#47642=CARTESIAN_POINT('Origin',(0.,-0.7625,0.));
#47643=CARTESIAN_POINT('',(-0.175,-0.8,-2.14313189850787E-17));
#47644=CARTESIAN_POINT('Origin',(0.,-0.8,0.));
#47645=CARTESIAN_POINT('',(-0.2125,-0.7625,-2.60237444818813E-17));
#47646=CARTESIAN_POINT('Origin',(0.,-0.8,0.));
#47647=CARTESIAN_POINT('',(0.,0.,0.));
#47648=CARTESIAN_POINT('Origin',(0.,0.,0.));
#47649=CARTESIAN_POINT('',(-0.32,0.16,3.91886975727153E-17));
#47650=CARTESIAN_POINT('Origin',(0.,0.16,0.));
#47651=CARTESIAN_POINT('',(-0.32,0.,3.91886975727153E-17));
#47652=CARTESIAN_POINT('',(-0.32,0.,3.91886975727153E-17));
#47653=CARTESIAN_POINT('Origin',(0.,0.,0.));
#47654=CARTESIAN_POINT('Origin',(0.,0.,0.));
#47655=CARTESIAN_POINT('',(-0.6,0.16,7.34788079488412E-17));
#47656=CARTESIAN_POINT('Origin',(0.,0.16,0.));
#47657=CARTESIAN_POINT('',(-0.6,0.,7.34788079488412E-17));
#47658=CARTESIAN_POINT('',(-0.6,0.,7.34788079488412E-17));
#47659=CARTESIAN_POINT('Origin',(0.,0.,0.));
#47660=CARTESIAN_POINT('Origin',(0.,0.16,0.));
#47661=CARTESIAN_POINT('Origin',(0.,0.,0.));
#47662=CARTESIAN_POINT('',(0.,0.,0.));
#47663=CARTESIAN_POINT('Origin',(0.45,0.6,0.));
#47664=CARTESIAN_POINT('',(-0.45,0.6,-5.51091059616309E-17));
#47665=CARTESIAN_POINT('Origin',(0.,0.6,0.));
#47666=CARTESIAN_POINT('Origin',(0.,0.575,0.));
#47667=CARTESIAN_POINT('',(-0.5,0.55,-6.12323399573677E-17));
#47668=CARTESIAN_POINT('Origin',(0.,0.55,0.));
#47669=CARTESIAN_POINT('',(-0.475,0.575,-5.81707229594993E-17));
#47670=CARTESIAN_POINT('Origin',(0.,0.29,0.));
#47671=CARTESIAN_POINT('',(-0.5,0.0299999999999998,-6.12323399573677E-17));
#47672=CARTESIAN_POINT('Origin',(0.,0.0299999999999998,0.));
#47673=CARTESIAN_POINT('',(-0.5,0.29,-6.12323399573677E-17));
#47674=CARTESIAN_POINT('Origin',(0.,0.0150000000000001,0.));
#47675=CARTESIAN_POINT('',(-0.47,7.11236625150491E-17,-5.75583995599256E-17));
#47676=CARTESIAN_POINT('Origin',(0.,0.,0.));
#47677=CARTESIAN_POINT('',(-0.485,0.0150000000000001,-5.93953697586466E-17));
#47678=CARTESIAN_POINT('Origin',(0.32,0.,0.));
#47679=CARTESIAN_POINT('',(-0.32,-6.93889390390723E-18,-3.91886975727153E-17));
#47680=CARTESIAN_POINT('Origin',(0.,0.,0.));
#47681=CARTESIAN_POINT('Origin',(0.,-0.02,0.));
#47682=CARTESIAN_POINT('',(-0.2942,-0.0515999999999999,3.60291088309151E-17));
#47683=CARTESIAN_POINT('Origin',(0.,-0.0515999999999999,0.));
#47684=CARTESIAN_POINT('',(-0.31,-0.02,-3.7964050773568E-17));
#47685=CARTESIAN_POINT('Origin',(0.,-1.24,0.));
#47686=CARTESIAN_POINT('',(-0.2942,-2.4458,3.60291088309151E-17));
#47687=CARTESIAN_POINT('Origin',(0.,-2.4458,0.));
#47688=CARTESIAN_POINT('',(-0.2942,-1.24,-3.60291088309151E-17));
#47689=CARTESIAN_POINT('Origin',(0.,-2.47,0.));
#47690=CARTESIAN_POINT('',(-0.24,-2.5,-2.93915231795365E-17));
#47691=CARTESIAN_POINT('Origin',(0.,-2.5,0.));
#47692=CARTESIAN_POINT('',(-0.27,-2.47,-3.30654635769785E-17));
#47693=CARTESIAN_POINT('Origin',(0.,-2.5,0.));
#47694=CARTESIAN_POINT('Origin',(0.144337567297406,-0.6,-0.25));
#47695=CARTESIAN_POINT('',(0.288675134594813,-0.6,0.));
#47696=CARTESIAN_POINT('',(0.144337567297406,-0.6,-0.25));
#47697=CARTESIAN_POINT('',(0.288675134594813,-0.6,0.));
#47698=CARTESIAN_POINT('',(0.144337567297406,-0.96,-0.25));
#47699=CARTESIAN_POINT('',(0.144337567297406,-0.6,-0.25));
#47700=CARTESIAN_POINT('',(0.288675134594813,-0.96,0.));
#47701=CARTESIAN_POINT('',(0.288675134594813,-0.96,0.));
#47702=CARTESIAN_POINT('',(0.288675134594813,-0.6,0.));
#47703=CARTESIAN_POINT('Origin',(-0.144337567297406,-0.6,-0.25));
#47704=CARTESIAN_POINT('',(-0.144337567297406,-0.6,-0.25));
#47705=CARTESIAN_POINT('',(0.144337567297406,-0.6,-0.25));
#47706=CARTESIAN_POINT('',(-0.144337567297406,-0.96,-0.25));
#47707=CARTESIAN_POINT('',(-0.144337567297406,-0.6,-0.25));
#47708=CARTESIAN_POINT('',(0.144337567297406,-0.96,-0.25));
#47709=CARTESIAN_POINT('Origin',(-0.288675134594813,-0.6,-8.32667268468867E-17));
#47710=CARTESIAN_POINT('',(-0.288675134594813,-0.6,-3.53525079574969E-17));
#47711=CARTESIAN_POINT('',(-0.144337567297406,-0.6,-0.25));
#47712=CARTESIAN_POINT('',(-0.288675134594813,-0.96,-5.55111512312578E-17));
#47713=CARTESIAN_POINT('',(-0.288675134594813,-0.6,-3.53525079574969E-17));
#47714=CARTESIAN_POINT('',(-0.144337567297406,-0.96,-0.25));
#47715=CARTESIAN_POINT('Origin',(-0.144337567297407,-0.6,0.25));
#47716=CARTESIAN_POINT('',(-0.144337567297407,-0.6,0.25));
#47717=CARTESIAN_POINT('',(-0.288675134594813,-0.6,-3.53525079574969E-17));
#47718=CARTESIAN_POINT('',(-0.144337567297407,-0.96,0.25));
#47719=CARTESIAN_POINT('',(-0.144337567297407,-0.6,0.25));
#47720=CARTESIAN_POINT('',(-0.288675134594813,-0.96,-3.53525079574969E-17));
#47721=CARTESIAN_POINT('Origin',(0.144337567297406,-0.6,0.25));
#47722=CARTESIAN_POINT('',(0.144337567297406,-0.6,0.25));
#47723=CARTESIAN_POINT('',(-0.144337567297407,-0.6,0.25));
#47724=CARTESIAN_POINT('',(0.144337567297406,-0.96,0.25));
#47725=CARTESIAN_POINT('',(0.144337567297406,-0.6,0.25));
#47726=CARTESIAN_POINT('',(-0.144337567297407,-0.96,0.25));
#47727=CARTESIAN_POINT('Origin',(0.288675134594813,-0.6,0.));
#47728=CARTESIAN_POINT('',(0.144337567297406,-0.6,0.25));
#47729=CARTESIAN_POINT('',(0.144337567297406,-0.96,0.25));
#47730=CARTESIAN_POINT('Origin',(0.,-0.6,0.));
#47731=CARTESIAN_POINT('Origin',(0.,-0.96,0.));
#47732=CARTESIAN_POINT('',(0.,0.,0.));
#47733=CARTESIAN_POINT('',(0.,0.,0.));
#47734=CARTESIAN_POINT('',(0.,0.,0.));
#47735=CARTESIAN_POINT('',(0.,0.,0.));
#47736=CARTESIAN_POINT('',(0.,0.,0.));
#47737=CARTESIAN_POINT('',(0.,0.,0.));
#47738=CARTESIAN_POINT('',(0.,0.,0.));
#47739=CARTESIAN_POINT('',(0.,0.,0.));
#47740=CARTESIAN_POINT('',(0.,0.,0.));
#47741=CARTESIAN_POINT('',(0.,0.,0.));
#47742=CARTESIAN_POINT('',(1.,-7.8,2.2));
#47743=CARTESIAN_POINT('',(1.,-5.5,2.2));
#47744=CARTESIAN_POINT('',(26.,-7.8,2.2));
#47745=CARTESIAN_POINT('',(26.,-5.5,2.2));
#47746=CARTESIAN_POINT('',(2.5,-6.,2.8));
#47747=CARTESIAN_POINT('',(4.5,-6.,3.77));
#47748=CARTESIAN_POINT('',(10.5,-6.,3.77));
#47749=CARTESIAN_POINT('',(16.5,-6.,3.77));
#47750=CARTESIAN_POINT('',(22.5,-6.,3.77));
#47751=CARTESIAN_POINT('',(3.,-2.4,0.));
#47752=CARTESIAN_POINT('',(3.,2.4,0.));
#47753=CARTESIAN_POINT('',(3.,0.,4.));
#47754=CARTESIAN_POINT('',(1.6,-2.1,4.));
#47755=CARTESIAN_POINT('',(1.6,2.1,4.));
#47756=CARTESIAN_POINT('',(1.6,0.,6.1));
#47757=CARTESIAN_POINT('',(24.,-3.5,0.));
#47758=CARTESIAN_POINT('',(24.,3.5,0.));
#47759=CARTESIAN_POINT('',(24.,0.,4.));
#47760=CARTESIAN_POINT('',(25.4,-2.6,4.));
#47761=CARTESIAN_POINT('',(25.4,2.6,4.));
#47762=CARTESIAN_POINT('',(25.4,0.,6.6));
#47763=CARTESIAN_POINT('',(3.5,-9.25,2.4));
#47764=CARTESIAN_POINT('',(23.5,-9.25,2.4));
#47765=CARTESIAN_POINT('',(0.,0.,0.));
#47766=CARTESIAN_POINT('',(0.,0.,0.));
#47767=CARTESIAN_POINT('',(0.,0.,0.));
#47768=CARTESIAN_POINT('',(0.,0.,0.));
#47769=CARTESIAN_POINT('',(0.,0.,0.));
#47770=CARTESIAN_POINT('',(0.,0.,0.));
#47771=CARTESIAN_POINT('',(28.2,0.,3.35));
#47772=CARTESIAN_POINT('',(25.8,1.8,4.));
#47773=CARTESIAN_POINT('',(28.,1.8,4.));
#47774=CARTESIAN_POINT('',(31.03,0.,6.5));
#47775=CARTESIAN_POINT('',(31.19,0.,6.5));
#47776=CARTESIAN_POINT('',(0.,0.,0.));
#47777=CARTESIAN_POINT('',(0.,0.,0.));
#47778=CARTESIAN_POINT('',(0.,-3.46410161513776,6.));
#47779=CARTESIAN_POINT('',(0.,0.,0.));
#47780=CARTESIAN_POINT('',(0.,0.,0.));
#47781=CARTESIAN_POINT('',(0.,0.,0.));
#47782=CARTESIAN_POINT('Origin',(15.5,-5.,-0.1));
#47783=CARTESIAN_POINT('',(14.95,-5.,0.));
#47784=CARTESIAN_POINT('Origin',(15.5,-5.,0.));
#47785=CARTESIAN_POINT('',(14.95,-5.,0.8));
#47786=CARTESIAN_POINT('',(14.95,-5.,-0.1));
#47787=CARTESIAN_POINT('Origin',(15.5,-5.,0.8));
#47788=CARTESIAN_POINT('Origin',(15.5,-5.,0.8));
#47789=CARTESIAN_POINT('Origin',(15.5,-3.5,-0.1));
#47790=CARTESIAN_POINT('',(14.95,-3.5,0.));
#47791=CARTESIAN_POINT('Origin',(15.5,-3.5,0.));
#47792=CARTESIAN_POINT('',(14.95,-3.5,0.8));
#47793=CARTESIAN_POINT('',(14.95,-3.5,-0.1));
#47794=CARTESIAN_POINT('Origin',(15.5,-3.5,0.8));
#47795=CARTESIAN_POINT('Origin',(15.5,-3.5,0.8));
#47796=CARTESIAN_POINT('Origin',(12.9,-6.,-0.1));
#47797=CARTESIAN_POINT('',(12.35,-6.,0.));
#47798=CARTESIAN_POINT('Origin',(12.9,-6.,0.));
#47799=CARTESIAN_POINT('',(12.35,-6.,0.8));
#47800=CARTESIAN_POINT('',(12.35,-6.,-0.1));
#47801=CARTESIAN_POINT('Origin',(12.9,-6.,0.8));
#47802=CARTESIAN_POINT('Origin',(12.9,-6.,0.8));
#47803=CARTESIAN_POINT('Origin',(12.9,-3.,-0.1));
#47804=CARTESIAN_POINT('',(12.35,-3.,0.));
#47805=CARTESIAN_POINT('Origin',(12.9,-3.,0.));
#47806=CARTESIAN_POINT('',(12.35,-3.,0.8));
#47807=CARTESIAN_POINT('',(12.35,-3.,-0.1));
#47808=CARTESIAN_POINT('Origin',(12.9,-3.,0.8));
#47809=CARTESIAN_POINT('Origin',(12.9,-3.,0.8));
#47810=CARTESIAN_POINT('Origin',(9.1,-6.,-0.1));
#47811=CARTESIAN_POINT('',(8.55,-6.,0.));
#47812=CARTESIAN_POINT('Origin',(9.1,-6.,0.));
#47813=CARTESIAN_POINT('',(8.55,-6.,0.8));
#47814=CARTESIAN_POINT('',(8.55,-6.,-0.1));
#47815=CARTESIAN_POINT('Origin',(9.1,-6.,0.8));
#47816=CARTESIAN_POINT('Origin',(9.1,-6.,0.8));
#47817=CARTESIAN_POINT('Origin',(9.1,-3.,-0.1));
#47818=CARTESIAN_POINT('',(8.55,-3.,0.));
#47819=CARTESIAN_POINT('Origin',(9.1,-3.,0.));
#47820=CARTESIAN_POINT('',(8.55,-3.,0.8));
#47821=CARTESIAN_POINT('',(8.55,-3.,-0.1));
#47822=CARTESIAN_POINT('Origin',(9.1,-3.,0.8));
#47823=CARTESIAN_POINT('Origin',(9.1,-3.,0.8));
#47824=CARTESIAN_POINT('Origin',(18.5,-3.5,-0.1));
#47825=CARTESIAN_POINT('',(17.95,-3.5,0.));
#47826=CARTESIAN_POINT('Origin',(18.5,-3.5,0.));
#47827=CARTESIAN_POINT('',(17.95,-3.5,0.8));
#47828=CARTESIAN_POINT('',(17.95,-3.5,-0.1));
#47829=CARTESIAN_POINT('Origin',(18.5,-3.5,0.8));
#47830=CARTESIAN_POINT('Origin',(18.5,-3.5,0.8));
#47831=CARTESIAN_POINT('Origin',(18.5,-5.,-0.1));
#47832=CARTESIAN_POINT('',(17.95,-5.,0.));
#47833=CARTESIAN_POINT('Origin',(18.5,-5.,0.));
#47834=CARTESIAN_POINT('',(17.95,-5.,0.8));
#47835=CARTESIAN_POINT('',(17.95,-5.,-0.1));
#47836=CARTESIAN_POINT('Origin',(18.5,-5.,0.8));
#47837=CARTESIAN_POINT('Origin',(18.5,-5.,0.8));
#47838=CARTESIAN_POINT('Origin',(8.,-7.2,0.6));
#47839=CARTESIAN_POINT('',(7.5,-7.2,0.6));
#47840=CARTESIAN_POINT('Origin',(8.,-7.2,0.6));
#47841=CARTESIAN_POINT('',(7.5,-7.2,1.2));
#47842=CARTESIAN_POINT('',(7.5,-7.2,0.6));
#47843=CARTESIAN_POINT('Origin',(8.,-7.2,1.2));
#47844=CARTESIAN_POINT('Origin',(8.,-7.2,0.6));
#47845=CARTESIAN_POINT('',(7.725,-7.2,0.6));
#47846=CARTESIAN_POINT('Origin',(8.,-7.2,0.6));
#47847=CARTESIAN_POINT('Origin',(18.,-1.8,0.6));
#47848=CARTESIAN_POINT('',(17.5,-1.8,0.6));
#47849=CARTESIAN_POINT('Origin',(18.,-1.8,0.6));
#47850=CARTESIAN_POINT('',(17.5,-1.8,1.2));
#47851=CARTESIAN_POINT('',(17.5,-1.8,0.6));
#47852=CARTESIAN_POINT('Origin',(18.,-1.8,1.2));
#47853=CARTESIAN_POINT('Origin',(18.,-1.8,0.6));
#47854=CARTESIAN_POINT('',(17.725,-1.8,0.6));
#47855=CARTESIAN_POINT('Origin',(18.,-1.8,0.6));
#47856=CARTESIAN_POINT('Origin',(8.,-1.8,0.6));
#47857=CARTESIAN_POINT('',(7.5,-1.8,0.6));
#47858=CARTESIAN_POINT('Origin',(8.,-1.8,0.6));
#47859=CARTESIAN_POINT('',(7.5,-1.8,1.2));
#47860=CARTESIAN_POINT('',(7.5,-1.8,0.6));
#47861=CARTESIAN_POINT('Origin',(8.,-1.8,1.2));
#47862=CARTESIAN_POINT('Origin',(8.,-1.8,0.6));
#47863=CARTESIAN_POINT('',(7.725,-1.8,0.6));
#47864=CARTESIAN_POINT('Origin',(8.,-1.8,0.6));
#47865=CARTESIAN_POINT('Origin',(18.,-7.2,0.6));
#47866=CARTESIAN_POINT('',(17.5,-7.2,0.6));
#47867=CARTESIAN_POINT('Origin',(18.,-7.2,0.6));
#47868=CARTESIAN_POINT('',(17.5,-7.2,1.2));
#47869=CARTESIAN_POINT('',(17.5,-7.2,0.6));
#47870=CARTESIAN_POINT('Origin',(18.,-7.2,1.2));
#47871=CARTESIAN_POINT('Origin',(18.,-7.2,0.6));
#47872=CARTESIAN_POINT('',(17.725,-7.2,0.6));
#47873=CARTESIAN_POINT('Origin',(18.,-7.2,0.6));
#47874=CARTESIAN_POINT('Origin',(8.,-7.2,-0.1));
#47875=CARTESIAN_POINT('',(7.725,-7.2,0.));
#47876=CARTESIAN_POINT('Origin',(8.,-7.2,0.));
#47877=CARTESIAN_POINT('',(7.725,-7.2,-0.1));
#47878=CARTESIAN_POINT('Origin',(18.,-1.8,-0.1));
#47879=CARTESIAN_POINT('',(17.725,-1.8,0.));
#47880=CARTESIAN_POINT('Origin',(18.,-1.8,0.));
#47881=CARTESIAN_POINT('',(17.725,-1.8,-0.1));
#47882=CARTESIAN_POINT('Origin',(8.,-1.8,-0.1));
#47883=CARTESIAN_POINT('',(7.725,-1.8,0.));
#47884=CARTESIAN_POINT('Origin',(8.,-1.8,0.));
#47885=CARTESIAN_POINT('',(7.725,-1.8,-0.1));
#47886=CARTESIAN_POINT('Origin',(18.,-7.2,-0.1));
#47887=CARTESIAN_POINT('',(17.725,-7.2,0.));
#47888=CARTESIAN_POINT('Origin',(18.,-7.2,0.));
#47889=CARTESIAN_POINT('',(17.725,-7.2,-0.1));
#47890=CARTESIAN_POINT('Origin',(23.5,-9.25,-0.1));
#47891=CARTESIAN_POINT('',(23.29,-9.25,0.));
#47892=CARTESIAN_POINT('Origin',(23.5,-9.25,0.));
#47893=CARTESIAN_POINT('',(23.29,-9.25,1.2));
#47894=CARTESIAN_POINT('',(23.29,-9.25,-0.1));
#47895=CARTESIAN_POINT('Origin',(23.5,-9.25,1.2));
#47896=CARTESIAN_POINT('Origin',(3.5,-9.25,-0.1));
#47897=CARTESIAN_POINT('',(3.29,-9.25,0.));
#47898=CARTESIAN_POINT('Origin',(3.5,-9.25,0.));
#47899=CARTESIAN_POINT('',(3.29,-9.25,1.2));
#47900=CARTESIAN_POINT('',(3.29,-9.25,-0.1));
#47901=CARTESIAN_POINT('Origin',(3.5,-9.25,1.2));
#47902=CARTESIAN_POINT('Origin',(24.,-3.5,-0.1));
#47903=CARTESIAN_POINT('',(23.67,-3.5,0.));
#47904=CARTESIAN_POINT('Origin',(24.,-3.5,0.));
#47905=CARTESIAN_POINT('',(23.67,-3.5,1.2));
#47906=CARTESIAN_POINT('',(23.67,-3.5,-0.1));
#47907=CARTESIAN_POINT('Origin',(24.,-3.5,1.2));
#47908=CARTESIAN_POINT('Origin',(24.,3.5,-0.1));
#47909=CARTESIAN_POINT('',(23.67,3.5,0.));
#47910=CARTESIAN_POINT('Origin',(24.,3.5,0.));
#47911=CARTESIAN_POINT('',(23.67,3.5,1.2));
#47912=CARTESIAN_POINT('',(23.67,3.5,-0.1));
#47913=CARTESIAN_POINT('Origin',(24.,3.5,1.2));
#47914=CARTESIAN_POINT('Origin',(3.,-2.4,-0.1));
#47915=CARTESIAN_POINT('',(2.725,-2.4,0.));
#47916=CARTESIAN_POINT('Origin',(3.,-2.4,0.));
#47917=CARTESIAN_POINT('',(2.725,-2.4,1.2));
#47918=CARTESIAN_POINT('',(2.725,-2.4,-0.1));
#47919=CARTESIAN_POINT('Origin',(3.,-2.4,1.2));
#47920=CARTESIAN_POINT('Origin',(3.,2.4,-0.1));
#47921=CARTESIAN_POINT('',(2.725,2.4,0.));
#47922=CARTESIAN_POINT('Origin',(3.,2.4,0.));
#47923=CARTESIAN_POINT('',(2.725,2.4,1.2));
#47924=CARTESIAN_POINT('',(2.725,2.4,-0.1));
#47925=CARTESIAN_POINT('Origin',(3.,2.4,1.2));
#47926=CARTESIAN_POINT('Origin',(26.,-7.8,-0.1));
#47927=CARTESIAN_POINT('',(25.79,-7.8,0.));
#47928=CARTESIAN_POINT('Origin',(26.,-7.8,0.));
#47929=CARTESIAN_POINT('',(25.79,-7.8,1.2));
#47930=CARTESIAN_POINT('',(25.79,-7.8,-0.1));
#47931=CARTESIAN_POINT('Origin',(26.,-7.8,1.2));
#47932=CARTESIAN_POINT('Origin',(1.,-5.5,-0.1));
#47933=CARTESIAN_POINT('',(0.79,-5.5,0.));
#47934=CARTESIAN_POINT('Origin',(1.,-5.5,0.));
#47935=CARTESIAN_POINT('',(0.79,-5.5,1.2));
#47936=CARTESIAN_POINT('',(0.79,-5.5,-0.1));
#47937=CARTESIAN_POINT('Origin',(1.,-5.5,1.2));
#47938=CARTESIAN_POINT('Origin',(1.,-7.8,-0.1));
#47939=CARTESIAN_POINT('',(0.79,-7.8,0.));
#47940=CARTESIAN_POINT('Origin',(1.,-7.8,0.));
#47941=CARTESIAN_POINT('',(0.79,-7.8,1.2));
#47942=CARTESIAN_POINT('',(0.79,-7.8,-0.1));
#47943=CARTESIAN_POINT('Origin',(1.,-7.8,1.2));
#47944=CARTESIAN_POINT('Origin',(26.,-5.5,-0.1));
#47945=CARTESIAN_POINT('',(25.79,-5.5,0.));
#47946=CARTESIAN_POINT('Origin',(26.,-5.5,0.));
#47947=CARTESIAN_POINT('',(25.79,-5.5,1.2));
#47948=CARTESIAN_POINT('',(25.79,-5.5,-0.1));
#47949=CARTESIAN_POINT('Origin',(26.,-5.5,1.2));
#47950=CARTESIAN_POINT('Origin',(27.,5.,0.));
#47951=CARTESIAN_POINT('',(27.,5.,0.));
#47952=CARTESIAN_POINT('',(0.,5.,0.));
#47953=CARTESIAN_POINT('',(27.,5.,0.));
#47954=CARTESIAN_POINT('',(0.,5.,1.2));
#47955=CARTESIAN_POINT('',(0.,5.,0.));
#47956=CARTESIAN_POINT('',(27.,5.,1.2));
#47957=CARTESIAN_POINT('',(27.,5.,1.2));
#47958=CARTESIAN_POINT('',(27.,5.,0.));
#47959=CARTESIAN_POINT('Origin',(27.,-10.,0.));
#47960=CARTESIAN_POINT('',(27.,-10.,0.));
#47961=CARTESIAN_POINT('',(27.,-10.,0.));
#47962=CARTESIAN_POINT('',(27.,-10.,1.2));
#47963=CARTESIAN_POINT('',(27.,-10.,1.2));
#47964=CARTESIAN_POINT('',(27.,-10.,0.));
#47965=CARTESIAN_POINT('Origin',(0.,-10.,0.));
#47966=CARTESIAN_POINT('',(0.,-10.,0.));
#47967=CARTESIAN_POINT('',(0.,-10.,0.));
#47968=CARTESIAN_POINT('',(0.,-10.,1.2));
#47969=CARTESIAN_POINT('',(0.,-10.,1.2));
#47970=CARTESIAN_POINT('',(0.,-10.,0.));
#47971=CARTESIAN_POINT('Origin',(0.,5.,0.));
#47972=CARTESIAN_POINT('',(0.,5.,0.));
#47973=CARTESIAN_POINT('',(0.,5.,1.2));
#47974=CARTESIAN_POINT('Origin',(13.5,-2.5,1.2));
#47975=CARTESIAN_POINT('Origin',(13.5,-2.5,0.));
#47976=CARTESIAN_POINT('',(0.,0.,0.));
#47977=CARTESIAN_POINT('Origin',(26.,-5.5,2.2));
#47978=CARTESIAN_POINT('',(25.5,-5.5,2.2));
#47979=CARTESIAN_POINT('',(25.5,-5.5,2.8));
#47980=CARTESIAN_POINT('',(25.5,-5.5,2.2));
#47981=CARTESIAN_POINT('',(26.,-5.,2.2));
#47982=CARTESIAN_POINT('Origin',(26.,-5.5,2.2));
#47983=CARTESIAN_POINT('',(26.,-5.,2.8));
#47984=CARTESIAN_POINT('',(26.,-5.,2.2));
#47985=CARTESIAN_POINT('Origin',(26.,-5.5,2.8));
#47986=CARTESIAN_POINT('Origin',(1.,-5.5,2.2));
#47987=CARTESIAN_POINT('',(0.5,-5.5,2.2));
#47988=CARTESIAN_POINT('',(0.5,-5.5,2.8));
#47989=CARTESIAN_POINT('',(0.5,-5.5,2.2));
#47990=CARTESIAN_POINT('',(1.,-5.,2.2));
#47991=CARTESIAN_POINT('Origin',(1.,-5.5,2.2));
#47992=CARTESIAN_POINT('',(1.,-5.,2.8));
#47993=CARTESIAN_POINT('',(1.,-5.,2.2));
#47994=CARTESIAN_POINT('Origin',(1.,-5.5,2.8));
#47995=CARTESIAN_POINT('Origin',(16.5,-6.,1.1));
#47996=CARTESIAN_POINT('',(16.335,-6.,1.2));
#47997=CARTESIAN_POINT('Origin',(16.5,-6.,1.2));
#47998=CARTESIAN_POINT('',(16.335,-6.,2.8));
#47999=CARTESIAN_POINT('',(16.335,-6.,1.1));
#48000=CARTESIAN_POINT('Origin',(16.5,-6.,2.8));
#48001=CARTESIAN_POINT('Origin',(10.5,-6.,1.1));
#48002=CARTESIAN_POINT('',(10.335,-6.,1.2));
#48003=CARTESIAN_POINT('Origin',(10.5,-6.,1.2));
#48004=CARTESIAN_POINT('',(10.335,-6.,2.8));
#48005=CARTESIAN_POINT('',(10.335,-6.,1.1));
#48006=CARTESIAN_POINT('Origin',(10.5,-6.,2.8));
#48007=CARTESIAN_POINT('Origin',(4.5,-6.,1.1));
#48008=CARTESIAN_POINT('',(4.335,-6.,1.2));
#48009=CARTESIAN_POINT('Origin',(4.5,-6.,1.2));
#48010=CARTESIAN_POINT('',(4.335,-6.,2.8));
#48011=CARTESIAN_POINT('',(4.335,-6.,1.1));
#48012=CARTESIAN_POINT('Origin',(4.5,-6.,2.8));
#48013=CARTESIAN_POINT('Origin',(22.5,-6.,1.1));
#48014=CARTESIAN_POINT('',(22.335,-6.,1.2));
#48015=CARTESIAN_POINT('Origin',(22.5,-6.,1.2));
#48016=CARTESIAN_POINT('',(22.335,-6.,2.8));
#48017=CARTESIAN_POINT('',(22.335,-6.,1.1));
#48018=CARTESIAN_POINT('Origin',(22.5,-6.,2.8));
#48019=CARTESIAN_POINT('Origin',(26.,-7.8,2.2));
#48020=CARTESIAN_POINT('',(25.5,-7.8,2.2));
#48021=CARTESIAN_POINT('Origin',(26.,-7.8,2.2));
#48022=CARTESIAN_POINT('',(25.5,-7.8,2.8));
#48023=CARTESIAN_POINT('',(25.5,-7.8,2.2));
#48024=CARTESIAN_POINT('Origin',(26.,-7.8,2.8));
#48025=CARTESIAN_POINT('Origin',(26.,-7.8,2.2));
#48026=CARTESIAN_POINT('',(25.725,-7.8,2.2));
#48027=CARTESIAN_POINT('Origin',(26.,-7.8,2.2));
#48028=CARTESIAN_POINT('Origin',(1.,-5.5,2.2));
#48029=CARTESIAN_POINT('Origin',(1.,-5.5,2.8));
#48030=CARTESIAN_POINT('',(1.,-5.,2.2));
#48031=CARTESIAN_POINT('Origin',(1.,-5.5,2.2));
#48032=CARTESIAN_POINT('Origin',(1.,-5.5,2.2));
#48033=CARTESIAN_POINT('',(0.725,-5.5,2.2));
#48034=CARTESIAN_POINT('Origin',(1.,-5.5,2.2));
#48035=CARTESIAN_POINT('Origin',(1.,-7.8,2.2));
#48036=CARTESIAN_POINT('',(0.5,-7.8,2.2));
#48037=CARTESIAN_POINT('Origin',(1.,-7.8,2.2));
#48038=CARTESIAN_POINT('',(0.5,-7.8,2.8));
#48039=CARTESIAN_POINT('',(0.5,-7.8,2.2));
#48040=CARTESIAN_POINT('Origin',(1.,-7.8,2.8));
#48041=CARTESIAN_POINT('Origin',(1.,-7.8,2.2));
#48042=CARTESIAN_POINT('',(0.725,-7.8,2.2));
#48043=CARTESIAN_POINT('Origin',(1.,-7.8,2.2));
#48044=CARTESIAN_POINT('Origin',(26.,-5.5,2.2));
#48045=CARTESIAN_POINT('Origin',(26.,-5.5,2.8));
#48046=CARTESIAN_POINT('',(26.,-5.,2.2));
#48047=CARTESIAN_POINT('Origin',(26.,-5.5,2.2));
#48048=CARTESIAN_POINT('Origin',(26.,-5.5,2.2));
#48049=CARTESIAN_POINT('',(25.725,-5.5,2.2));
#48050=CARTESIAN_POINT('Origin',(26.,-5.5,2.2));
#48051=CARTESIAN_POINT('Origin',(13.5,-6.75,2.8));
#48052=CARTESIAN_POINT('',(0.,-5.,2.8));
#48053=CARTESIAN_POINT('',(0.,-8.5,2.8));
#48054=CARTESIAN_POINT('',(0.,-5.,2.8));
#48055=CARTESIAN_POINT('',(27.,-8.5,2.8));
#48056=CARTESIAN_POINT('',(0.,-8.5,2.8));
#48057=CARTESIAN_POINT('',(27.,-5.,2.8));
#48058=CARTESIAN_POINT('',(27.,-8.5,2.8));
#48059=CARTESIAN_POINT('',(27.,-5.,2.8));
#48060=CARTESIAN_POINT('',(27.,-5.,2.8));
#48061=CARTESIAN_POINT('',(27.,-5.,2.8));
#48062=CARTESIAN_POINT('Origin',(26.,-7.8,1.1));
#48063=CARTESIAN_POINT('',(25.725,-7.8,1.2));
#48064=CARTESIAN_POINT('Origin',(26.,-7.8,1.2));
#48065=CARTESIAN_POINT('',(25.725,-7.8,1.1));
#48066=CARTESIAN_POINT('Origin',(1.,-5.5,1.1));
#48067=CARTESIAN_POINT('',(0.725,-5.5,1.2));
#48068=CARTESIAN_POINT('Origin',(1.,-5.5,1.2));
#48069=CARTESIAN_POINT('',(0.725,-5.5,1.1));
#48070=CARTESIAN_POINT('Origin',(1.,-7.8,1.1));
#48071=CARTESIAN_POINT('',(0.725,-7.8,1.2));
#48072=CARTESIAN_POINT('Origin',(1.,-7.8,1.2));
#48073=CARTESIAN_POINT('',(0.725,-7.8,1.1));
#48074=CARTESIAN_POINT('Origin',(26.,-5.5,1.1));
#48075=CARTESIAN_POINT('',(25.725,-5.5,1.2));
#48076=CARTESIAN_POINT('Origin',(26.,-5.5,1.2));
#48077=CARTESIAN_POINT('',(25.725,-5.5,1.1));
#48078=CARTESIAN_POINT('Origin',(27.,-5.,1.2));
#48079=CARTESIAN_POINT('',(27.,-5.,1.2));
#48080=CARTESIAN_POINT('',(0.,-5.,1.2));
#48081=CARTESIAN_POINT('',(27.,-5.,1.2));
#48082=CARTESIAN_POINT('',(0.,-5.,1.2));
#48083=CARTESIAN_POINT('',(27.,-5.,1.2));
#48084=CARTESIAN_POINT('Origin',(27.,-8.5,1.2));
#48085=CARTESIAN_POINT('',(27.,-8.5,1.2));
#48086=CARTESIAN_POINT('',(27.,-8.5,1.2));
#48087=CARTESIAN_POINT('',(27.,-8.5,1.2));
#48088=CARTESIAN_POINT('Origin',(0.,-8.5,1.2));
#48089=CARTESIAN_POINT('',(0.,-8.5,1.2));
#48090=CARTESIAN_POINT('',(0.,-8.5,1.2));
#48091=CARTESIAN_POINT('',(0.,-8.5,1.2));
#48092=CARTESIAN_POINT('Origin',(0.,-5.,1.2));
#48093=CARTESIAN_POINT('',(0.,-5.,1.2));
#48094=CARTESIAN_POINT('Origin',(13.5,-6.75,1.2));
#48095=CARTESIAN_POINT('',(0.,0.,0.));
#48096=CARTESIAN_POINT('Origin',(1.9,-2.1,4.));
#48097=CARTESIAN_POINT('',(2.,-2.1,4.165));
#48098=CARTESIAN_POINT('Origin',(2.,-2.1,4.));
#48099=CARTESIAN_POINT('',(4.,-2.1,4.165));
#48100=CARTESIAN_POINT('',(1.9,-2.1,4.165));
#48101=CARTESIAN_POINT('Origin',(4.,-2.1,4.));
#48102=CARTESIAN_POINT('Origin',(1.9,2.1,4.));
#48103=CARTESIAN_POINT('',(2.,2.1,4.165));
#48104=CARTESIAN_POINT('Origin',(2.,2.1,4.));
#48105=CARTESIAN_POINT('',(4.,2.1,4.165));
#48106=CARTESIAN_POINT('',(1.9,2.1,4.165));
#48107=CARTESIAN_POINT('Origin',(4.,2.1,4.));
#48108=CARTESIAN_POINT('Origin',(1.9,0.,6.1));
#48109=CARTESIAN_POINT('',(2.,-2.02066721859313E-17,6.265));
#48110=CARTESIAN_POINT('Origin',(2.,0.,6.1));
#48111=CARTESIAN_POINT('',(4.,2.02066721859313E-17,6.265));
#48112=CARTESIAN_POINT('',(1.9,-2.02066721859313E-17,6.265));
#48113=CARTESIAN_POINT('Origin',(4.,0.,6.1));
#48114=CARTESIAN_POINT('Origin',(1.9,0.,4.));
#48115=CARTESIAN_POINT('',(2.,-1.95943487863577E-16,5.6));
#48116=CARTESIAN_POINT('Origin',(2.,0.,4.));
#48117=CARTESIAN_POINT('',(3.5,-1.95943487863577E-16,5.6));
#48118=CARTESIAN_POINT('',(1.9,-1.95943487863577E-16,5.6));
#48119=CARTESIAN_POINT('Origin',(3.5,0.,4.));
#48120=CARTESIAN_POINT('Origin',(3.5,0.,4.));
#48121=CARTESIAN_POINT('',(3.5,1.71450551880629E-16,5.4));
#48122=CARTESIAN_POINT('Origin',(3.5,0.,4.));
#48123=CARTESIAN_POINT('Origin',(1.9,0.,4.));
#48124=CARTESIAN_POINT('',(4.,1.71450551880629E-16,5.4));
#48125=CARTESIAN_POINT('',(1.9,-1.71450551880629E-16,5.4));
#48126=CARTESIAN_POINT('Origin',(4.,0.,4.));
#48127=CARTESIAN_POINT('Origin',(3.,-2.4,1.1));
#48128=CARTESIAN_POINT('',(2.79,-2.4,1.2));
#48129=CARTESIAN_POINT('Origin',(3.,-2.4,1.2));
#48130=CARTESIAN_POINT('',(2.79,-2.4,2.9));
#48131=CARTESIAN_POINT('',(2.79,-2.4,1.1));
#48132=CARTESIAN_POINT('Origin',(3.,-2.4,2.9));
#48133=CARTESIAN_POINT('Origin',(3.,-2.4,2.9));
#48134=CARTESIAN_POINT('Origin',(3.,2.4,1.1));
#48135=CARTESIAN_POINT('',(2.79,2.4,1.2));
#48136=CARTESIAN_POINT('Origin',(3.,2.4,1.2));
#48137=CARTESIAN_POINT('',(2.79,2.4,2.9));
#48138=CARTESIAN_POINT('',(2.79,2.4,1.1));
#48139=CARTESIAN_POINT('Origin',(3.,2.4,2.9));
#48140=CARTESIAN_POINT('Origin',(3.,2.4,2.9));
#48141=CARTESIAN_POINT('Origin',(4.,3.,1.2));
#48142=CARTESIAN_POINT('',(4.,3.,1.2));
#48143=CARTESIAN_POINT('',(2.,3.,1.2));
#48144=CARTESIAN_POINT('',(4.,3.,1.2));
#48145=CARTESIAN_POINT('',(2.,3.,7.));
#48146=CARTESIAN_POINT('',(2.,3.,1.2));
#48147=CARTESIAN_POINT('',(4.,3.,7.));
#48148=CARTESIAN_POINT('',(4.,3.,7.));
#48149=CARTESIAN_POINT('',(4.,3.,1.2));
#48150=CARTESIAN_POINT('Origin',(4.,-3.,1.2));
#48151=CARTESIAN_POINT('',(4.,-3.,1.2));
#48152=CARTESIAN_POINT('',(4.,-3.,1.2));
#48153=CARTESIAN_POINT('',(4.,-3.,7.));
#48154=CARTESIAN_POINT('',(4.,-3.,7.));
#48155=CARTESIAN_POINT('',(4.,-3.,1.2));
#48156=CARTESIAN_POINT('Origin',(2.,-3.,1.2));
#48157=CARTESIAN_POINT('',(2.,-3.,1.2));
#48158=CARTESIAN_POINT('',(2.,-3.,1.2));
#48159=CARTESIAN_POINT('',(2.,-3.,7.));
#48160=CARTESIAN_POINT('',(2.,-3.,7.));
#48161=CARTESIAN_POINT('',(2.,-3.,1.2));
#48162=CARTESIAN_POINT('Origin',(2.,3.,1.2));
#48163=CARTESIAN_POINT('',(2.,3.,1.2));
#48164=CARTESIAN_POINT('',(2.,3.,7.));
#48165=CARTESIAN_POINT('Origin',(3.,0.,7.));
#48166=CARTESIAN_POINT('Origin',(3.,0.,1.2));
#48167=CARTESIAN_POINT('',(0.,0.,0.));
#48168=CARTESIAN_POINT('Origin',(1.5,-2.1,4.));
#48169=CARTESIAN_POINT('',(1.6,-2.1,4.225));
#48170=CARTESIAN_POINT('Origin',(1.6,-2.1,4.));
#48171=CARTESIAN_POINT('',(2.,-2.1,4.225));
#48172=CARTESIAN_POINT('',(1.5,-2.1,4.225));
#48173=CARTESIAN_POINT('Origin',(2.,-2.1,4.));
#48174=CARTESIAN_POINT('Origin',(1.5,2.1,4.));
#48175=CARTESIAN_POINT('',(1.6,2.1,4.225));
#48176=CARTESIAN_POINT('Origin',(1.6,2.1,4.));
#48177=CARTESIAN_POINT('',(2.,2.1,4.225));
#48178=CARTESIAN_POINT('',(1.5,2.1,4.225));
#48179=CARTESIAN_POINT('Origin',(2.,2.1,4.));
#48180=CARTESIAN_POINT('Origin',(1.5,0.,6.1));
#48181=CARTESIAN_POINT('',(1.6,-2.75545529808154E-17,6.325));
#48182=CARTESIAN_POINT('Origin',(1.6,0.,6.1));
#48183=CARTESIAN_POINT('',(2.,2.75545529808154E-17,6.325));
#48184=CARTESIAN_POINT('',(1.5,-2.75545529808154E-17,6.325));
#48185=CARTESIAN_POINT('Origin',(2.,0.,6.1));
#48186=CARTESIAN_POINT('Origin',(2.,0.,4.));
#48187=CARTESIAN_POINT('',(2.5,-1.94718841064429E-16,5.59));
#48188=CARTESIAN_POINT('Origin',(2.5,0.,4.));
#48189=CARTESIAN_POINT('',(2.,-1.94718841064429E-16,5.59));
#48190=CARTESIAN_POINT('',(2.,-1.94718841064429E-16,5.59));
#48191=CARTESIAN_POINT('Origin',(2.,0.,4.));
#48192=CARTESIAN_POINT('Origin',(2.5,0.,4.));
#48193=CARTESIAN_POINT('',(2.5,-1.46957615897682E-16,5.2));
#48194=CARTESIAN_POINT('Origin',(2.5,0.,4.));
#48195=CARTESIAN_POINT('Origin',(1.6,0.,4.));
#48196=CARTESIAN_POINT('',(1.6,-1.46957615897682E-16,5.2));
#48197=CARTESIAN_POINT('',(1.6,-1.46957615897682E-16,5.2));
#48198=CARTESIAN_POINT('Origin',(1.6,0.,4.));
#48199=CARTESIAN_POINT('Origin',(1.6,0.,4.));
#48200=CARTESIAN_POINT('',(2.,-2.93915231795365E-16,6.4));
#48201=CARTESIAN_POINT('Origin',(2.,0.,4.));
#48202=CARTESIAN_POINT('',(1.6,-2.93915231795365E-16,6.4));
#48203=CARTESIAN_POINT('',(1.6,-2.93915231795365E-16,6.4));
#48204=CARTESIAN_POINT('Origin',(1.6,0.,4.));
#48205=CARTESIAN_POINT('Origin',(2.,0.,4.));
#48206=CARTESIAN_POINT('Origin',(1.6,0.,4.));
#48207=CARTESIAN_POINT('',(0.,0.,0.));
#48208=CARTESIAN_POINT('Origin',(22.9,-2.6,4.));
#48209=CARTESIAN_POINT('',(23.,-2.6,4.165));
#48210=CARTESIAN_POINT('Origin',(23.,-2.6,4.));
#48211=CARTESIAN_POINT('',(25.,-2.6,4.165));
#48212=CARTESIAN_POINT('',(22.9,-2.6,4.165));
#48213=CARTESIAN_POINT('Origin',(25.,-2.6,4.));
#48214=CARTESIAN_POINT('Origin',(22.9,2.6,4.));
#48215=CARTESIAN_POINT('',(23.,2.6,4.165));
#48216=CARTESIAN_POINT('Origin',(23.,2.6,4.));
#48217=CARTESIAN_POINT('',(25.,2.6,4.165));
#48218=CARTESIAN_POINT('',(22.9,2.6,4.165));
#48219=CARTESIAN_POINT('Origin',(25.,2.6,4.));
#48220=CARTESIAN_POINT('Origin',(22.9,0.,6.6));
#48221=CARTESIAN_POINT('',(23.,-2.02066721859313E-17,6.765));
#48222=CARTESIAN_POINT('Origin',(23.,0.,6.6));
#48223=CARTESIAN_POINT('',(25.,2.02066721859313E-17,6.765));
#48224=CARTESIAN_POINT('',(22.9,-2.02066721859313E-17,6.765));
#48225=CARTESIAN_POINT('Origin',(25.,0.,6.6));
#48226=CARTESIAN_POINT('Origin',(23.3,0.,4.));
#48227=CARTESIAN_POINT('',(23.3,-2.87791997799628E-16,6.35));
#48228=CARTESIAN_POINT('Origin',(23.3,0.,4.));
#48229=CARTESIAN_POINT('',(25.,2.87791997799628E-16,6.35));
#48230=CARTESIAN_POINT('',(23.3,-2.87791997799628E-16,6.35));
#48231=CARTESIAN_POINT('Origin',(25.,0.,4.));
#48232=CARTESIAN_POINT('Origin',(23.3,0.,4.));
#48233=CARTESIAN_POINT('',(23.3,-2.63299061816681E-16,6.15));
#48234=CARTESIAN_POINT('Origin',(23.3,0.,4.));
#48235=CARTESIAN_POINT('Origin',(22.9,0.,4.));
#48236=CARTESIAN_POINT('',(23.,-2.63299061816681E-16,6.15));
#48237=CARTESIAN_POINT('Origin',(23.,0.,4.));
#48238=CARTESIAN_POINT('',(22.9,-2.63299061816681E-16,6.15));
#48239=CARTESIAN_POINT('Origin',(24.,-3.5,1.1));
#48240=CARTESIAN_POINT('',(23.75,-3.5,1.2));
#48241=CARTESIAN_POINT('Origin',(24.,-3.5,1.2));
#48242=CARTESIAN_POINT('',(23.75,-3.5,2.9));
#48243=CARTESIAN_POINT('',(23.75,-3.5,1.1));
#48244=CARTESIAN_POINT('Origin',(24.,-3.5,2.9));
#48245=CARTESIAN_POINT('Origin',(24.,-3.5,2.9));
#48246=CARTESIAN_POINT('Origin',(24.,3.5,1.1));
#48247=CARTESIAN_POINT('',(23.75,3.5,1.2));
#48248=CARTESIAN_POINT('Origin',(24.,3.5,1.2));
#48249=CARTESIAN_POINT('',(23.75,3.5,2.9));
#48250=CARTESIAN_POINT('',(23.75,3.5,1.1));
#48251=CARTESIAN_POINT('Origin',(24.,3.5,2.9));
#48252=CARTESIAN_POINT('Origin',(24.,3.5,2.9));
#48253=CARTESIAN_POINT('Origin',(25.,5.,1.2));
#48254=CARTESIAN_POINT('',(25.,5.,1.2));
#48255=CARTESIAN_POINT('',(23.,5.,1.2));
#48256=CARTESIAN_POINT('',(25.,5.,1.2));
#48257=CARTESIAN_POINT('',(23.,5.,7.));
#48258=CARTESIAN_POINT('',(23.,5.,1.2));
#48259=CARTESIAN_POINT('',(25.,5.,7.));
#48260=CARTESIAN_POINT('',(25.,5.,7.));
#48261=CARTESIAN_POINT('',(25.,5.,1.2));
#48262=CARTESIAN_POINT('Origin',(25.,-5.,1.2));
#48263=CARTESIAN_POINT('',(25.,-5.,1.2));
#48264=CARTESIAN_POINT('',(25.,-5.,1.2));
#48265=CARTESIAN_POINT('',(25.,-5.,7.));
#48266=CARTESIAN_POINT('',(25.,-5.,7.));
#48267=CARTESIAN_POINT('',(25.,-5.,1.2));
#48268=CARTESIAN_POINT('Origin',(23.,-5.,1.2));
#48269=CARTESIAN_POINT('',(23.,-5.,1.2));
#48270=CARTESIAN_POINT('',(23.,-5.,1.2));
#48271=CARTESIAN_POINT('',(23.,-5.,7.));
#48272=CARTESIAN_POINT('',(23.,-5.,7.));
#48273=CARTESIAN_POINT('',(23.,-5.,1.2));
#48274=CARTESIAN_POINT('Origin',(23.,5.,1.2));
#48275=CARTESIAN_POINT('',(23.,5.,1.2));
#48276=CARTESIAN_POINT('',(23.,5.,7.));
#48277=CARTESIAN_POINT('Origin',(24.,0.,7.));
#48278=CARTESIAN_POINT('Origin',(24.,0.,1.2));
#48279=CARTESIAN_POINT('',(0.,0.,0.));
#48280=CARTESIAN_POINT('Origin',(24.9,-2.6,4.));
#48281=CARTESIAN_POINT('',(25.,-2.6,4.225));
#48282=CARTESIAN_POINT('Origin',(25.,-2.6,4.));
#48283=CARTESIAN_POINT('',(25.4,-2.6,4.225));
#48284=CARTESIAN_POINT('',(24.9,-2.6,4.225));
#48285=CARTESIAN_POINT('Origin',(25.4,-2.6,4.));
#48286=CARTESIAN_POINT('Origin',(24.9,2.6,4.));
#48287=CARTESIAN_POINT('',(25.,2.6,4.225));
#48288=CARTESIAN_POINT('Origin',(25.,2.6,4.));
#48289=CARTESIAN_POINT('',(25.4,2.6,4.225));
#48290=CARTESIAN_POINT('',(24.9,2.6,4.225));
#48291=CARTESIAN_POINT('Origin',(25.4,2.6,4.));
#48292=CARTESIAN_POINT('Origin',(24.9,0.,6.6));
#48293=CARTESIAN_POINT('',(25.,-2.75545529808154E-17,6.825));
#48294=CARTESIAN_POINT('Origin',(25.,0.,6.6));
#48295=CARTESIAN_POINT('',(25.4,2.75545529808154E-17,6.825));
#48296=CARTESIAN_POINT('',(24.9,-2.75545529808154E-17,6.825));
#48297=CARTESIAN_POINT('Origin',(25.4,0.,6.6));
#48298=CARTESIAN_POINT('Origin',(24.9,3.5,1.22));
#48299=CARTESIAN_POINT('',(25.,-1.12765242872084,1.22));
#48300=CARTESIAN_POINT('',(25.4,-1.12765242872084,1.22));
#48301=CARTESIAN_POINT('',(25.,-1.12765242872084,1.22));
#48302=CARTESIAN_POINT('',(25.,1.12765242872084,1.22));
#48303=CARTESIAN_POINT('',(25.,1.75,1.22));
#48304=CARTESIAN_POINT('',(25.4,1.12765242872084,1.22));
#48305=CARTESIAN_POINT('',(25.,1.12765242872084,1.22));
#48306=CARTESIAN_POINT('',(25.4,1.75,1.22));
#48307=CARTESIAN_POINT('Origin',(25.,0.,4.));
#48308=CARTESIAN_POINT('Origin',(25.,0.,4.));
#48309=CARTESIAN_POINT('',(25.,-2.86567351000481E-16,6.34));
#48310=CARTESIAN_POINT('Origin',(25.,0.,4.));
#48311=CARTESIAN_POINT('Origin',(25.,0.,4.));
#48312=CARTESIAN_POINT('Origin',(25.4,0.,4.));
#48313=CARTESIAN_POINT('Origin',(24.7,0.,4.));
#48314=CARTESIAN_POINT('',(24.7,-2.86567351000481E-16,6.34));
#48315=CARTESIAN_POINT('',(24.7,-2.86567351000481E-16,6.34));
#48316=CARTESIAN_POINT('Origin',(24.7,0.,4.));
#48317=CARTESIAN_POINT('Origin',(24.7,0.,4.));
#48318=CARTESIAN_POINT('',(24.7,-2.20436423846524E-16,5.8));
#48319=CARTESIAN_POINT('Origin',(24.7,0.,4.));
#48320=CARTESIAN_POINT('Origin',(25.,0.,4.));
#48321=CARTESIAN_POINT('',(25.4,-2.20436423846524E-16,5.8));
#48322=CARTESIAN_POINT('Origin',(25.4,0.,4.));
#48323=CARTESIAN_POINT('',(25.,-2.20436423846524E-16,5.8));
#48324=CARTESIAN_POINT('Origin',(25.4,0.,4.));
#48325=CARTESIAN_POINT('',(0.,0.,0.));
#48326=CARTESIAN_POINT('Origin',(3.5,-9.25,2.4));
#48327=CARTESIAN_POINT('',(3.025,-9.25,2.4));
#48328=CARTESIAN_POINT('Origin',(3.5,-9.25,2.4));
#48329=CARTESIAN_POINT('',(3.025,-9.25,7.));
#48330=CARTESIAN_POINT('',(3.025,-9.25,2.4));
#48331=CARTESIAN_POINT('Origin',(3.5,-9.25,7.));
#48332=CARTESIAN_POINT('Origin',(3.5,-9.25,2.4));
#48333=CARTESIAN_POINT('',(3.225,-9.25,2.4));
#48334=CARTESIAN_POINT('Origin',(3.5,-9.25,2.4));
#48335=CARTESIAN_POINT('Origin',(3.5,-9.25,1.1));
#48336=CARTESIAN_POINT('',(3.225,-9.25,1.2));
#48337=CARTESIAN_POINT('Origin',(3.5,-9.25,1.2));
#48338=CARTESIAN_POINT('',(3.225,-9.25,1.1));
#48339=CARTESIAN_POINT('Origin',(4.,-8.5,1.2));
#48340=CARTESIAN_POINT('',(4.,-8.5,1.2));
#48341=CARTESIAN_POINT('',(3.,-8.5,1.2));
#48342=CARTESIAN_POINT('',(4.,-8.5,1.2));
#48343=CARTESIAN_POINT('',(3.,-8.5,7.));
#48344=CARTESIAN_POINT('',(3.,-8.5,1.2));
#48345=CARTESIAN_POINT('',(4.,-8.5,7.));
#48346=CARTESIAN_POINT('',(4.,-8.5,7.));
#48347=CARTESIAN_POINT('',(4.,-8.5,1.2));
#48348=CARTESIAN_POINT('Origin',(4.,-10.,1.2));
#48349=CARTESIAN_POINT('',(4.,-10.,1.2));
#48350=CARTESIAN_POINT('',(4.,-10.,1.2));
#48351=CARTESIAN_POINT('',(4.,-10.,7.));
#48352=CARTESIAN_POINT('',(4.,-10.,7.));
#48353=CARTESIAN_POINT('',(4.,-10.,1.2));
#48354=CARTESIAN_POINT('Origin',(3.,-10.,1.2));
#48355=CARTESIAN_POINT('',(3.,-10.,1.2));
#48356=CARTESIAN_POINT('',(3.,-10.,1.2));
#48357=CARTESIAN_POINT('',(3.,-10.,7.));
#48358=CARTESIAN_POINT('',(3.,-10.,7.));
#48359=CARTESIAN_POINT('',(3.,-10.,1.2));
#48360=CARTESIAN_POINT('Origin',(3.,-8.5,1.2));
#48361=CARTESIAN_POINT('',(3.,-8.5,1.2));
#48362=CARTESIAN_POINT('',(3.,-8.5,7.));
#48363=CARTESIAN_POINT('Origin',(3.5,-9.25,7.));
#48364=CARTESIAN_POINT('Origin',(3.5,-9.25,1.2));
#48365=CARTESIAN_POINT('',(0.,0.,0.));
#48366=CARTESIAN_POINT('Origin',(23.5,-9.25,2.4));
#48367=CARTESIAN_POINT('',(23.025,-9.25,2.4));
#48368=CARTESIAN_POINT('Origin',(23.5,-9.25,2.4));
#48369=CARTESIAN_POINT('',(23.025,-9.25,7.));
#48370=CARTESIAN_POINT('',(23.025,-9.25,2.4));
#48371=CARTESIAN_POINT('Origin',(23.5,-9.25,7.));
#48372=CARTESIAN_POINT('Origin',(23.5,-9.25,2.4));
#48373=CARTESIAN_POINT('',(23.225,-9.25,2.4));
#48374=CARTESIAN_POINT('Origin',(23.5,-9.25,2.4));
#48375=CARTESIAN_POINT('Origin',(23.5,-9.25,1.1));
#48376=CARTESIAN_POINT('',(23.225,-9.25,1.2));
#48377=CARTESIAN_POINT('Origin',(23.5,-9.25,1.2));
#48378=CARTESIAN_POINT('',(23.225,-9.25,1.1));
#48379=CARTESIAN_POINT('Origin',(24.,-8.5,1.2));
#48380=CARTESIAN_POINT('',(24.,-8.5,1.2));
#48381=CARTESIAN_POINT('',(23.,-8.5,1.2));
#48382=CARTESIAN_POINT('',(24.,-8.5,1.2));
#48383=CARTESIAN_POINT('',(23.,-8.5,7.));
#48384=CARTESIAN_POINT('',(23.,-8.5,1.2));
#48385=CARTESIAN_POINT('',(24.,-8.5,7.));
#48386=CARTESIAN_POINT('',(24.,-8.5,7.));
#48387=CARTESIAN_POINT('',(24.,-8.5,1.2));
#48388=CARTESIAN_POINT('Origin',(24.,-10.,1.2));
#48389=CARTESIAN_POINT('',(24.,-10.,1.2));
#48390=CARTESIAN_POINT('',(24.,-10.,1.2));
#48391=CARTESIAN_POINT('',(24.,-10.,7.));
#48392=CARTESIAN_POINT('',(24.,-10.,7.));
#48393=CARTESIAN_POINT('',(24.,-10.,1.2));
#48394=CARTESIAN_POINT('Origin',(23.,-10.,1.2));
#48395=CARTESIAN_POINT('',(23.,-10.,1.2));
#48396=CARTESIAN_POINT('',(23.,-10.,1.2));
#48397=CARTESIAN_POINT('',(23.,-10.,7.));
#48398=CARTESIAN_POINT('',(23.,-10.,7.));
#48399=CARTESIAN_POINT('',(23.,-10.,1.2));
#48400=CARTESIAN_POINT('Origin',(23.,-8.5,1.2));
#48401=CARTESIAN_POINT('',(23.,-8.5,1.2));
#48402=CARTESIAN_POINT('',(23.,-8.5,7.));
#48403=CARTESIAN_POINT('Origin',(23.5,-9.25,7.));
#48404=CARTESIAN_POINT('Origin',(23.5,-9.25,1.2));
#48405=CARTESIAN_POINT('',(0.,0.,0.));
#48406=CARTESIAN_POINT('Origin',(14.,0.,0.97));
#48407=CARTESIAN_POINT('',(13.625,-4.59242549680257E-17,0.97));
#48408=CARTESIAN_POINT('Origin',(14.,0.,0.97));
#48409=CARTESIAN_POINT('',(13.625,4.59242549680257E-17,1.5));
#48410=CARTESIAN_POINT('',(13.625,-4.59242549680257E-17,0.97));
#48411=CARTESIAN_POINT('Origin',(14.,0.,1.5));
#48412=CARTESIAN_POINT('Origin',(14.,0.,0.97));
#48413=CARTESIAN_POINT('',(13.775,-2.75545529808154E-17,0.97));
#48414=CARTESIAN_POINT('Origin',(14.,0.,0.97));
#48415=CARTESIAN_POINT('Origin',(8.,0.,0.97));
#48416=CARTESIAN_POINT('',(7.625,-4.59242549680257E-17,0.97));
#48417=CARTESIAN_POINT('Origin',(8.,0.,0.97));
#48418=CARTESIAN_POINT('',(7.625,4.59242549680257E-17,1.5));
#48419=CARTESIAN_POINT('',(7.625,-4.59242549680257E-17,0.97));
#48420=CARTESIAN_POINT('Origin',(8.,0.,1.5));
#48421=CARTESIAN_POINT('Origin',(8.,0.,0.97));
#48422=CARTESIAN_POINT('',(7.775,-2.75545529808154E-17,0.97));
#48423=CARTESIAN_POINT('Origin',(8.,0.,0.97));
#48424=CARTESIAN_POINT('Origin',(2.,0.,0.97));
#48425=CARTESIAN_POINT('',(1.625,-4.59242549680257E-17,0.97));
#48426=CARTESIAN_POINT('Origin',(2.,0.,0.97));
#48427=CARTESIAN_POINT('',(1.625,4.59242549680257E-17,1.5));
#48428=CARTESIAN_POINT('',(1.625,-4.59242549680257E-17,0.97));
#48429=CARTESIAN_POINT('Origin',(2.,0.,1.5));
#48430=CARTESIAN_POINT('Origin',(2.,0.,0.97));
#48431=CARTESIAN_POINT('',(1.775,-2.75545529808155E-17,0.97));
#48432=CARTESIAN_POINT('Origin',(2.,0.,0.97));
#48433=CARTESIAN_POINT('Origin',(20.,0.,0.97));
#48434=CARTESIAN_POINT('',(19.625,-4.59242549680257E-17,0.97));
#48435=CARTESIAN_POINT('Origin',(20.,0.,0.97));
#48436=CARTESIAN_POINT('',(19.625,4.59242549680257E-17,1.5));
#48437=CARTESIAN_POINT('',(19.625,-4.59242549680257E-17,0.97));
#48438=CARTESIAN_POINT('Origin',(20.,0.,1.5));
#48439=CARTESIAN_POINT('Origin',(20.,0.,0.97));
#48440=CARTESIAN_POINT('',(19.775,-2.75545529808156E-17,0.97));
#48441=CARTESIAN_POINT('Origin',(20.,0.,0.97));
#48442=CARTESIAN_POINT('Origin',(14.,0.,-0.1));
#48443=CARTESIAN_POINT('',(13.775,-2.75545529808154E-17,0.));
#48444=CARTESIAN_POINT('Origin',(14.,0.,0.));
#48445=CARTESIAN_POINT('',(13.775,-2.75545529808154E-17,-0.1));
#48446=CARTESIAN_POINT('Origin',(8.,0.,-0.1));
#48447=CARTESIAN_POINT('',(7.775,-2.75545529808154E-17,0.));
#48448=CARTESIAN_POINT('Origin',(8.,0.,0.));
#48449=CARTESIAN_POINT('',(7.775,-2.75545529808154E-17,-0.1));
#48450=CARTESIAN_POINT('Origin',(2.,0.,-0.1));
#48451=CARTESIAN_POINT('',(1.775,-2.75545529808155E-17,0.));
#48452=CARTESIAN_POINT('Origin',(2.,0.,0.));
#48453=CARTESIAN_POINT('',(1.775,-2.75545529808155E-17,-0.1));
#48454=CARTESIAN_POINT('Origin',(20.,0.,-0.1));
#48455=CARTESIAN_POINT('',(19.775,-2.75545529808156E-17,0.));
#48456=CARTESIAN_POINT('Origin',(20.,0.,0.));
#48457=CARTESIAN_POINT('',(19.775,-2.75545529808156E-17,-0.1));
#48458=CARTESIAN_POINT('Origin',(0.,-0.53,1.));
#48459=CARTESIAN_POINT('',(0.,-0.53,1.));
#48460=CARTESIAN_POINT('',(0.,-0.75,0.85));
#48461=CARTESIAN_POINT('',(0.,-0.53,1.));
#48462=CARTESIAN_POINT('',(22.,-0.75,0.85));
#48463=CARTESIAN_POINT('',(0.,-0.75,0.85));
#48464=CARTESIAN_POINT('',(22.,-0.53,1.));
#48465=CARTESIAN_POINT('',(22.,-0.53,1.));
#48466=CARTESIAN_POINT('',(0.,-0.53,1.));
#48467=CARTESIAN_POINT('Origin',(0.,-0.53,1.15));
#48468=CARTESIAN_POINT('',(0.,-0.53,1.15));
#48469=CARTESIAN_POINT('',(0.,-0.53,1.15));
#48470=CARTESIAN_POINT('',(22.,-0.53,1.15));
#48471=CARTESIAN_POINT('',(22.,-0.53,1.15));
#48472=CARTESIAN_POINT('',(0.,-0.53,1.15));
#48473=CARTESIAN_POINT('Origin',(0.,-0.75,1.3));
#48474=CARTESIAN_POINT('',(0.,-0.75,1.3));
#48475=CARTESIAN_POINT('',(0.,-0.75,1.3));
#48476=CARTESIAN_POINT('',(22.,-0.75,1.3));
#48477=CARTESIAN_POINT('',(22.,-0.75,1.3));
#48478=CARTESIAN_POINT('',(0.,-0.75,1.3));
#48479=CARTESIAN_POINT('Origin',(0.,-0.75,1.5));
#48480=CARTESIAN_POINT('',(0.,-0.75,1.5));
#48481=CARTESIAN_POINT('',(0.,-0.75,1.5));
#48482=CARTESIAN_POINT('',(22.,-0.75,1.5));
#48483=CARTESIAN_POINT('',(22.,-0.75,1.5));
#48484=CARTESIAN_POINT('',(0.,-0.75,1.5));
#48485=CARTESIAN_POINT('Origin',(0.,0.75,1.5));
#48486=CARTESIAN_POINT('',(0.,0.75,1.5));
#48487=CARTESIAN_POINT('',(0.,0.75,1.5));
#48488=CARTESIAN_POINT('',(22.,0.75,1.5));
#48489=CARTESIAN_POINT('',(22.,0.75,1.5));
#48490=CARTESIAN_POINT('',(0.,0.75,1.5));
#48491=CARTESIAN_POINT('Origin',(0.,0.75,1.3));
#48492=CARTESIAN_POINT('',(0.,0.75,1.3));
#48493=CARTESIAN_POINT('',(0.,0.75,1.3));
#48494=CARTESIAN_POINT('',(22.,0.75,1.3));
#48495=CARTESIAN_POINT('',(22.,0.75,1.3));
#48496=CARTESIAN_POINT('',(0.,0.75,1.3));
#48497=CARTESIAN_POINT('Origin',(0.,0.53,1.15));
#48498=CARTESIAN_POINT('',(0.,0.53,1.15));
#48499=CARTESIAN_POINT('',(0.,0.53,1.15));
#48500=CARTESIAN_POINT('',(22.,0.53,1.15));
#48501=CARTESIAN_POINT('',(22.,0.53,1.15));
#48502=CARTESIAN_POINT('',(0.,0.53,1.15));
#48503=CARTESIAN_POINT('Origin',(0.,0.53,1.));
#48504=CARTESIAN_POINT('',(0.,0.53,1.));
#48505=CARTESIAN_POINT('',(0.,0.53,1.));
#48506=CARTESIAN_POINT('',(22.,0.53,1.));
#48507=CARTESIAN_POINT('',(22.,0.53,1.));
#48508=CARTESIAN_POINT('',(0.,0.53,1.));
#48509=CARTESIAN_POINT('Origin',(0.,0.75,0.85));
#48510=CARTESIAN_POINT('',(0.,0.75,0.85));
#48511=CARTESIAN_POINT('',(0.,0.75,0.85));
#48512=CARTESIAN_POINT('',(22.,0.75,0.85));
#48513=CARTESIAN_POINT('',(22.,0.75,0.85));
#48514=CARTESIAN_POINT('',(0.,0.75,0.85));
#48515=CARTESIAN_POINT('Origin',(0.,0.75,0.));
#48516=CARTESIAN_POINT('',(0.,0.75,0.));
#48517=CARTESIAN_POINT('',(0.,0.75,0.));
#48518=CARTESIAN_POINT('',(22.,0.75,0.));
#48519=CARTESIAN_POINT('',(22.,0.75,0.));
#48520=CARTESIAN_POINT('',(0.,0.75,0.));
#48521=CARTESIAN_POINT('Origin',(0.,-0.75,0.));
#48522=CARTESIAN_POINT('',(0.,-0.75,0.));
#48523=CARTESIAN_POINT('',(0.,-0.75,0.));
#48524=CARTESIAN_POINT('',(22.,-0.75,0.));
#48525=CARTESIAN_POINT('',(22.,-0.75,0.));
#48526=CARTESIAN_POINT('',(0.,-0.75,0.));
#48527=CARTESIAN_POINT('Origin',(0.,-0.75,0.85));
#48528=CARTESIAN_POINT('',(0.,-0.75,0.85));
#48529=CARTESIAN_POINT('',(22.,-0.75,0.85));
#48530=CARTESIAN_POINT('Origin',(22.,0.,0.75));
#48531=CARTESIAN_POINT('Origin',(0.,0.,0.75));
#48532=CARTESIAN_POINT('',(0.,0.,0.));
#48533=CARTESIAN_POINT('',(0.,0.,0.));
#48534=CARTESIAN_POINT('Origin',(0.,0.,0.));
#48535=CARTESIAN_POINT('',(-1.070235,-0.308121667383195,-1.31065986708547E-16));
#48536=CARTESIAN_POINT('',(-1.31065986708547E-16,-0.308121667383195,1.070235));
#48537=CARTESIAN_POINT('Origin',(0.,-0.308121667383195,0.));
#48538=CARTESIAN_POINT('Origin',(0.,-0.308121667383195,0.));
#48539=CARTESIAN_POINT('',(-1.31065986708547E-16,0.308121667383195,1.070235));
#48540=CARTESIAN_POINT('Origin',(-1.34711147906209E-16,0.,1.1));
#48541=CARTESIAN_POINT('',(-1.070235,0.308121667383195,1.31065986708547E-16));
#48542=CARTESIAN_POINT('Origin',(0.,0.308121667383195,0.));
#48543=CARTESIAN_POINT('Origin',(0.,0.308121667383195,0.));
#48544=CARTESIAN_POINT('Origin',(0.,0.,0.));
#48545=CARTESIAN_POINT('',(-1.070235,0.5,-1.31065986708547E-16));
#48546=CARTESIAN_POINT('',(-1.070235,0.,-1.31065986708547E-16));
#48547=CARTESIAN_POINT('Origin',(0.,0.5,0.));
#48548=CARTESIAN_POINT('Origin',(0.,0.,0.));
#48549=CARTESIAN_POINT('',(-0.6,-0.44,-7.34788079488412E-17));
#48550=CARTESIAN_POINT('Origin',(0.,-0.44,0.));
#48551=CARTESIAN_POINT('',(-0.6,0.44,-7.34788079488412E-17));
#48552=CARTESIAN_POINT('',(-0.6,0.,-7.34788079488412E-17));
#48553=CARTESIAN_POINT('Origin',(0.,0.44,0.));
#48554=CARTESIAN_POINT('Origin',(0.,0.47,0.));
#48555=CARTESIAN_POINT('',(-0.66,0.5,-8.08266887437253E-17));
#48556=CARTESIAN_POINT('',(-0.63,0.47,-7.71527483462832E-17));
#48557=CARTESIAN_POINT('Origin',(0.,0.5,0.));
#48558=CARTESIAN_POINT('Origin',(1.070235,0.5,0.));
#48559=CARTESIAN_POINT('Origin',(0.,0.,0.));
#48560=CARTESIAN_POINT('',(-1.070235,-0.5,-1.31065986708547E-16));
#48561=CARTESIAN_POINT('Origin',(0.,-0.5,0.));
#48562=CARTESIAN_POINT('',(-1.070235,0.,-1.31065986708547E-16));
#48563=CARTESIAN_POINT('Origin',(0.66,-0.5,0.));
#48564=CARTESIAN_POINT('',(-0.66,-0.5,-8.08266887437253E-17));
#48565=CARTESIAN_POINT('Origin',(0.,-0.5,0.));
#48566=CARTESIAN_POINT('Origin',(0.,-0.47,0.));
#48567=CARTESIAN_POINT('',(-0.63,-0.47,-7.71527483462832E-17));
#48568=CARTESIAN_POINT('',(0.,0.,0.));
#48569=CARTESIAN_POINT('Origin',(0.,0.,0.));
#48570=CARTESIAN_POINT('',(-1.129765,0.308121667383195,-1.38356309103871E-16));
#48571=CARTESIAN_POINT('',(-1.38356309103871E-16,0.308121667383195,1.129765));
#48572=CARTESIAN_POINT('Origin',(0.,0.308121667383195,0.));
#48573=CARTESIAN_POINT('Origin',(0.,0.308121667383195,0.));
#48574=CARTESIAN_POINT('',(-1.38356309103871E-16,-0.308121667383195,1.129765));
#48575=CARTESIAN_POINT('Origin',(-1.34711147906209E-16,0.,1.1));
#48576=CARTESIAN_POINT('',(-1.129765,-0.308121667383195,1.38356309103871E-16));
#48577=CARTESIAN_POINT('Origin',(0.,-0.308121667383195,0.));
#48578=CARTESIAN_POINT('Origin',(0.,-0.308121667383195,0.));
#48579=CARTESIAN_POINT('Origin',(0.,0.,0.));
#48580=CARTESIAN_POINT('',(-1.129765,-0.5,-1.38356309103871E-16));
#48581=CARTESIAN_POINT('Origin',(0.,-0.5,0.));
#48582=CARTESIAN_POINT('',(-1.129765,0.,-1.38356309103871E-16));
#48583=CARTESIAN_POINT('Origin',(1.54,0.5,0.));
#48584=CARTESIAN_POINT('',(-1.54,0.5,-1.88595607068692E-16));
#48585=CARTESIAN_POINT('Origin',(0.,0.5,0.));
#48586=CARTESIAN_POINT('',(-1.129765,0.5,-1.38356309103871E-16));
#48587=CARTESIAN_POINT('Origin',(0.,0.5,0.));
#48588=CARTESIAN_POINT('Origin',(0.,0.47,0.));
#48589=CARTESIAN_POINT('',(-1.6,0.44,-1.95943487863577E-16));
#48590=CARTESIAN_POINT('Origin',(0.,0.44,0.));
#48591=CARTESIAN_POINT('',(-1.57,0.47,-1.92269547466134E-16));
#48592=CARTESIAN_POINT('Origin',(0.,0.,0.));
#48593=CARTESIAN_POINT('',(-1.6,-0.44,-1.95943487863577E-16));
#48594=CARTESIAN_POINT('Origin',(0.,-0.44,0.));
#48595=CARTESIAN_POINT('',(-1.6,0.,-1.95943487863577E-16));
#48596=CARTESIAN_POINT('Origin',(0.,-0.47,0.));
#48597=CARTESIAN_POINT('',(-1.54,-0.5,-1.88595607068692E-16));
#48598=CARTESIAN_POINT('Origin',(0.,-0.5,0.));
#48599=CARTESIAN_POINT('',(-1.57,-0.47,-1.92269547466134E-16));
#48600=CARTESIAN_POINT('Origin',(1.129765,-0.5,0.));
#48601=CARTESIAN_POINT('Origin',(0.,0.,0.));
#48602=CARTESIAN_POINT('',(-1.129765,0.,-1.38356309103871E-16));
#48603=CARTESIAN_POINT('',(0.,0.,0.));
#48604=CARTESIAN_POINT('Origin',(1.1,0.,0.));
#48605=CARTESIAN_POINT('',(1.1,-2.23201749654651E-33,0.29765));
#48606=CARTESIAN_POINT('',(1.1,-2.23201749654651E-33,-0.29765));
#48607=CARTESIAN_POINT('Origin',(1.1,0.,0.));
#48608=CARTESIAN_POINT('Origin',(0.685838782044607,0.,-0.860014630714833));
#48609=CARTESIAN_POINT('',(0.918550922801216,-5.31350540756609E-33,-0.674432891191581));
#48610=CARTESIAN_POINT('',(0.453126641287998,8.49470414473068E-34,-1.04559637023808));
#48611=CARTESIAN_POINT('Origin',(0.685838782044607,0.,-0.860014630714833));
#48612=CARTESIAN_POINT('Origin',(-0.244773027351946,0.,-1.07242070340001));
#48613=CARTESIAN_POINT('',(0.0454142657089739,-2.23201749654651E-33,-1.1386540593921));
#48614=CARTESIAN_POINT('',(-0.534960320412865,-2.23201749654651E-33,-1.00618734740791));
#48615=CARTESIAN_POINT('Origin',(-0.244773027351946,0.,-1.07242070340001));
#48616=CARTESIAN_POINT('Origin',(-0.991065754692661,0.,-0.477272113029314));
#48617=CARTESIAN_POINT('',(-0.86192025974432,8.49470414473067E-34,-0.745445496560469));
#48618=CARTESIAN_POINT('',(-1.120211249641,-5.31350540756609E-33,-0.209098729498159));
#48619=CARTESIAN_POINT('Origin',(-0.991065754692661,0.,-0.477272113029314));
#48620=CARTESIAN_POINT('Origin',(-0.991065754692661,0.,0.477272113029314));
#48621=CARTESIAN_POINT('',(-1.120211249641,-2.23201749654651E-33,0.209098729498159));
#48622=CARTESIAN_POINT('',(-0.86192025974432,-2.23201749654651E-33,0.745445496560469));
#48623=CARTESIAN_POINT('Origin',(-0.991065754692661,0.,0.477272113029314));
#48624=CARTESIAN_POINT('Origin',(-0.244773027351946,0.,1.07242070340001));
#48625=CARTESIAN_POINT('',(-0.534960320412866,-2.23201749654651E-33,1.00618734740791));
#48626=CARTESIAN_POINT('',(0.0454142657089737,-2.23201749654651E-33,1.1386540593921));
#48627=CARTESIAN_POINT('Origin',(-0.244773027351946,0.,1.07242070340001));
#48628=CARTESIAN_POINT('Origin',(0.685838782044607,0.,0.860014630714833));
#48629=CARTESIAN_POINT('',(0.453126641287998,-2.23201749654651E-33,1.04559637023808));
#48630=CARTESIAN_POINT('',(0.918550922801216,-2.23201749654651E-33,0.674432891191581));
#48631=CARTESIAN_POINT('Origin',(0.685838782044607,0.,0.860014630714833));
#48632=CARTESIAN_POINT('',(0.,0.,0.));
#48633=CARTESIAN_POINT('Origin',(0.685838782044607,0.,0.860014630714833));
#48634=CARTESIAN_POINT('',(0.413083465285518,-0.05953,0.993751811093549));
#48635=CARTESIAN_POINT('',(0.876916659919095,-0.05953,0.623857181492959));
#48636=CARTESIAN_POINT('Ctrl Pts',(0.413083465285518,-0.05953,0.993751811093549));
#48637=CARTESIAN_POINT('Ctrl Pts',(0.419070565453383,-0.0925528133349865,
0.991263089003441));
#48638=CARTESIAN_POINT('Ctrl Pts',(0.430199341854858,-0.124911173756694,
0.986608710139579));
#48639=CARTESIAN_POINT('Ctrl Pts',(0.457978755888596,-0.177924977804098,
0.973971221090534));
#48640=CARTESIAN_POINT('Ctrl Pts',(0.473077587363685,-0.199697230012983,
0.966820759530997));
#48641=CARTESIAN_POINT('Ctrl Pts',(0.507057380724533,-0.237895043532788,
0.949440676105255));
#48642=CARTESIAN_POINT('Ctrl Pts',(0.525933334162555,-0.254319232363049,
0.939198248544428));
#48643=CARTESIAN_POINT('Ctrl Pts',(0.564362943424238,-0.28018331644634,
0.916597376014514));
#48644=CARTESIAN_POINT('Ctrl Pts',(0.585840553788742,-0.29104845371857,
0.903141581680914));
#48645=CARTESIAN_POINT('Ctrl Pts',(0.629305439856167,-0.30527573347708,
0.873412008702649));
#48646=CARTESIAN_POINT('Ctrl Pts',(0.651278921914856,-0.308638795020976,
0.857118508332695));
#48647=CARTESIAN_POINT('Ctrl Pts',(0.690705563850638,-0.308638795020976,
0.825676810575914));
#48648=CARTESIAN_POINT('Ctrl Pts',(0.711480111898423,-0.30527573347708,
0.807879894508811));
#48649=CARTESIAN_POINT('Ctrl Pts',(0.750136149454208,-0.29104845371857,
0.772120216227122));
#48650=CARTESIAN_POINT('Ctrl Pts',(0.768033796848072,-0.28018331644634,
0.754175290318038));
#48651=CARTESIAN_POINT('Ctrl Pts',(0.798619410861634,-0.254319232363049,
0.721738358858166));
#48652=CARTESIAN_POINT('Ctrl Pts',(0.812805334167529,-0.237895043532788,
0.705614819529209));
#48653=CARTESIAN_POINT('Ctrl Pts',(0.837310877969633,-0.199697230012983,
0.676354402927683));
#48654=CARTESIAN_POINT('Ctrl Pts',(0.847641868610495,-0.177924977804098,
0.663225258065736));
#48655=CARTESIAN_POINT('Ctrl Pts',(0.866144010579847,-0.124911173756694,
0.638954437806245));
#48656=CARTESIAN_POINT('Ctrl Pts',(0.873158080166742,-0.0925528133349865,
0.62914037979579));
#48657=CARTESIAN_POINT('Ctrl Pts',(0.876916659919095,-0.05953,0.623857181492959));
#48658=CARTESIAN_POINT('',(0.437601487681057,-0.05953,1.03511272300331));
#48659=CARTESIAN_POINT('Origin',(0.685838782044607,-0.05953,0.860014630714833));
#48660=CARTESIAN_POINT('',(0.911784794170997,-0.05953,0.656964154625313));
#48661=CARTESIAN_POINT('Ctrl Pts',(0.911784794170998,-0.0595300000000001,
0.656964154625312));
#48662=CARTESIAN_POINT('Ctrl Pts',(0.909827729890942,-0.0762225747374255,
0.659680317203144));
#48663=CARTESIAN_POINT('Ctrl Pts',(0.907004864562642,-0.0928409665394228,
0.663576540841106));
#48664=CARTESIAN_POINT('Ctrl Pts',(0.895234408667242,-0.144299303100741,
0.679480524217551));
#48665=CARTESIAN_POINT('Ctrl Pts',(0.882797231409153,-0.177024326825049,
0.695831250979106));
#48666=CARTESIAN_POINT('Ctrl Pts',(0.854332839576145,-0.227269801620064,
0.73042219438957));
#48667=CARTESIAN_POINT('Ctrl Pts',(0.834863020612702,-0.251265615809407,
0.752807465209441));
#48668=CARTESIAN_POINT('Ctrl Pts',(0.800439809856111,-0.279889827963178,
0.789147407129766));
#48669=CARTESIAN_POINT('Ctrl Pts',(0.781998747691871,-0.290879136862659,
0.80756613568454));
#48670=CARTESIAN_POINT('Ctrl Pts',(0.742239891936898,-0.305251990234487,
0.844254137480382));
#48671=CARTESIAN_POINT('Ctrl Pts',(0.720906778729541,-0.308638795020976,
0.862505527716294));
#48672=CARTESIAN_POINT('Ctrl Pts',(0.680463863683392,-0.308638795020976,
0.894757676234429));
#48673=CARTESIAN_POINT('Ctrl Pts',(0.657923009631182,-0.305251990234488,
0.91149460735272));
#48674=CARTESIAN_POINT('Ctrl Pts',(0.613307674922609,-0.290879136862659,
0.942092777160053));
#48675=CARTESIAN_POINT('Ctrl Pts',(0.591247219971725,-0.279889827963178,
0.955972930713954));
#48676=CARTESIAN_POINT('Ctrl Pts',(0.548158511259202,-0.251265615809407,
0.981446681891443));
#48677=CARTESIAN_POINT('Ctrl Pts',(0.522002043615455,-0.227269801620063,
0.995447160474328));
#48678=CARTESIAN_POINT('Ctrl Pts',(0.481944444320713,-0.177024326825049,
1.01550068154148));
#48679=CARTESIAN_POINT('Ctrl Pts',(0.463236132117164,-0.14429930310074,
1.0239876538093));
#48680=CARTESIAN_POINT('Ctrl Pts',(0.445111721969657,-0.0928409665394226,
1.03192403056628));
#48681=CARTESIAN_POINT('Ctrl Pts',(0.440685038163619,-0.0762225747374254,
1.03380912944435));
#48682=CARTESIAN_POINT('Ctrl Pts',(0.437601487681056,-0.05953,1.03511272300331));
#48683=CARTESIAN_POINT('Origin',(0.685838782044607,-0.05953,0.860014630714833));
#48684=CARTESIAN_POINT('Origin',(0.,-0.208355,0.));
#48685=CARTESIAN_POINT('',(0.0548532617164168,-0.05953,1.12247250791415));
#48686=CARTESIAN_POINT('Origin',(0.,-0.05953,0.));
#48687=CARTESIAN_POINT('',(-0.536443649899848,-0.05953,0.987512846410683));
#48688=CARTESIAN_POINT('Ctrl Pts',(0.0548532617164173,-0.0595300000000001,
1.12247250791414));
#48689=CARTESIAN_POINT('Ctrl Pts',(0.05150947068137,-0.0762225747374254,
1.12263591311425));
#48690=CARTESIAN_POINT('Ctrl Pts',(0.0467032526342597,-0.0928409665394227,
1.12285816383385));
#48691=CARTESIAN_POINT('Ctrl Pts',(0.0269302585198975,-0.144299303100741,
1.12357162229597));
#48692=CARTESIAN_POINT('Ctrl Pts',(0.006392292392153,-0.177024326825049,
1.12404235695137));
#48693=CARTESIAN_POINT('Ctrl Pts',(-0.0383992541984087,-0.227269801620063,
1.12335509974011));
#48694=CARTESIAN_POINT('Ctrl Pts',(-0.0680399972366993,-0.251265615809407,
1.12208997038458));
#48695=CARTESIAN_POINT('Ctrl Pts',(-0.117914228755037,-0.279889827963178,
1.1178344036749));
#48696=CARTESIAN_POINT('Ctrl Pts',(-0.14381238480104,-0.290879136862659,
1.11490049012186));
#48697=CARTESIAN_POINT('Ctrl Pts',(-0.19728546073067,-0.305251990234488,
1.10669035995599));
#48698=CARTESIAN_POINT('Ctrl Pts',(-0.224855950742601,-0.308638795020976,
1.10139101611326));
#48699=CARTESIAN_POINT('Ctrl Pts',(-0.275287440920027,-0.308638795020976,
1.0898803575765));
#48700=CARTESIAN_POINT('Ctrl Pts',(-0.302426893214945,-0.305251990234488,
1.08269251410343));
#48701=CARTESIAN_POINT('Ctrl Pts',(-0.35416671187353,-0.290879136862659,
1.06688848765783));
#48702=CARTESIAN_POINT('Ctrl Pts',(-0.3787731215897,-0.279889827963178,
1.05829506364875));
#48703=CARTESIAN_POINT('Ctrl Pts',(-0.425554672694338,-0.251265615809407,
1.04048957871266));
#48704=CARTESIAN_POINT('Ctrl Pts',(-0.452808978448581,-0.227269801620063,
1.02876878445619));
#48705=CARTESIAN_POINT('Ctrl Pts',(-0.493462957200432,-0.177024326825049,
1.0099536580922));
#48706=CARTESIAN_POINT('Ctrl Pts',(-0.511762781179148,-0.14429930310074,
1.00061845128527));
#48707=CARTESIAN_POINT('Ctrl Pts',(-0.529268075276157,-0.0928409665394226,
0.991396466802468));
#48708=CARTESIAN_POINT('Ctrl Pts',(-0.533501897135713,-0.0762225747374254,
0.989110885965947));
#48709=CARTESIAN_POINT('Ctrl Pts',(-0.536443649899848,-0.0595300000000001,
0.987512846410683));
#48710=CARTESIAN_POINT('',(-0.843383895613249,-0.05953,0.742736168477219));
#48711=CARTESIAN_POINT('Origin',(0.,-0.05953,0.));
#48712=CARTESIAN_POINT('',(-1.10653577764992,-0.05953,0.196295654879792));
#48713=CARTESIAN_POINT('Ctrl Pts',(-0.843383895613249,-0.0595300000000001,
0.742736168477219));
#48714=CARTESIAN_POINT('Ctrl Pts',(-0.84559647055299,-0.0762225747374255,
0.740223768851062));
#48715=CARTESIAN_POINT('Ctrl Pts',(-0.848766861100456,-0.0928409665394227,
0.736604687327351));
#48716=CARTESIAN_POINT('Ctrl Pts',(-0.861652925570091,-0.144299303100741,
0.721590372101268));
#48717=CARTESIAN_POINT('Ctrl Pts',(-0.87482617317514,-0.177024326825049,
0.705826641853758));
#48718=CARTESIAN_POINT('Ctrl Pts',(-0.902215926359523,-0.227269801620063,
0.670378702718353));
#48719=CARTESIAN_POINT('Ctrl Pts',(-0.919707509403859,-0.251265615809407,
0.646415841396062));
#48720=CARTESIAN_POINT('Ctrl Pts',(-0.947476448101718,-0.279889827963178,
0.604769294586516));
#48721=CARTESIAN_POINT('Ctrl Pts',(-0.961329858300736,-0.290879136862659,
0.582692035672022));
#48722=CARTESIAN_POINT('Ctrl Pts',(-0.988250837578047,-0.305251990234488,
0.535766169015486));
#48723=CARTESIAN_POINT('Ctrl Pts',(-1.00129756308006,-0.308638795020976,
0.510906605094603));
#48724=CARTESIAN_POINT('Ctrl Pts',(-1.02374168767024,-0.308638795020976,
0.46430090015576));
#48725=CARTESIAN_POINT('Ctrl Pts',(-1.03504317708586,-0.305251990234488,
0.438600874831839));
#48726=CARTESIAN_POINT('Ctrl Pts',(-1.05494634094458,-0.290879136862659,
0.388295406390235));
#48727=CARTESIAN_POINT('Ctrl Pts',(-1.06356957703048,-0.279889827963178,
0.363699428370917));
#48728=CARTESIAN_POINT('Ctrl Pts',(-1.0788165083757,-0.251265615809407,
0.316022600643821));
#48729=CARTESIAN_POINT('Ctrl Pts',(-1.08664560412098,-0.227269801620063,
0.287406530683752));
#48730=CARTESIAN_POINT('Ctrl Pts',(-1.09728268713976,-0.177024326825049,
0.243890930799337));
#48731=CARTESIAN_POINT('Ctrl Pts',(-1.10139388218929,-0.144299303100741,
0.22376314604679));
#48732=CARTESIAN_POINT('Ctrl Pts',(-1.10509821673782,-0.0928409665394227,
0.204327142733961));
#48733=CARTESIAN_POINT('Ctrl Pts',(-1.10595102243643,-0.0762225747374254,
0.199591971170104));
#48734=CARTESIAN_POINT('Ctrl Pts',(-1.10653577764992,-0.0595300000000001,
0.196295654879792));
#48735=CARTESIAN_POINT('',(-1.123812,-0.05953,1.37627276864339E-16));
#48736=CARTESIAN_POINT('Origin',(0.,-0.05953,0.));
#48737=CARTESIAN_POINT('',(-1.123812,-0.35718,1.37627276864339E-16));
#48738=CARTESIAN_POINT('',(-1.123812,-0.208355,1.37627276864339E-16));
#48739=CARTESIAN_POINT('Origin',(0.,-0.35718,0.));
#48740=CARTESIAN_POINT('',(-1.10653577764992,-0.05953,-0.196295654879793));
#48741=CARTESIAN_POINT('Origin',(0.,-0.05953,0.));
#48742=CARTESIAN_POINT('',(-0.843383895613249,-0.05953,-0.742736168477219));
#48743=CARTESIAN_POINT('Ctrl Pts',(-1.10653577764992,-0.0595300000000001,
-0.196295654879792));
#48744=CARTESIAN_POINT('Ctrl Pts',(-1.10595102243643,-0.0762225747374255,
-0.199591971170104));
#48745=CARTESIAN_POINT('Ctrl Pts',(-1.10509821673782,-0.0928409665394228,
-0.204327142733962));
#48746=CARTESIAN_POINT('Ctrl Pts',(-1.10139388218929,-0.144299303100741,
-0.22376314604679));
#48747=CARTESIAN_POINT('Ctrl Pts',(-1.09728268713976,-0.177024326825049,
-0.243890930799338));
#48748=CARTESIAN_POINT('Ctrl Pts',(-1.08664560412098,-0.227269801620063,
-0.287406530683753));
#48749=CARTESIAN_POINT('Ctrl Pts',(-1.0788165083757,-0.251265615809407,
-0.316022600643821));
#48750=CARTESIAN_POINT('Ctrl Pts',(-1.06356957703048,-0.279889827963178,
-0.363699428370918));
#48751=CARTESIAN_POINT('Ctrl Pts',(-1.05494634094458,-0.290879136862659,
-0.388295406390235));
#48752=CARTESIAN_POINT('Ctrl Pts',(-1.03504317708586,-0.305251990234488,
-0.438600874831839));
#48753=CARTESIAN_POINT('Ctrl Pts',(-1.02374168767024,-0.308638795020976,
-0.46430090015576));
#48754=CARTESIAN_POINT('Ctrl Pts',(-1.00129756308006,-0.308638795020976,
-0.510906605094603));
#48755=CARTESIAN_POINT('Ctrl Pts',(-0.988250837578047,-0.305251990234488,
-0.535766169015486));
#48756=CARTESIAN_POINT('Ctrl Pts',(-0.961329858300736,-0.290879136862659,
-0.582692035672022));
#48757=CARTESIAN_POINT('Ctrl Pts',(-0.947476448101718,-0.279889827963178,
-0.604769294586516));
#48758=CARTESIAN_POINT('Ctrl Pts',(-0.919707509403859,-0.251265615809407,
-0.646415841396062));
#48759=CARTESIAN_POINT('Ctrl Pts',(-0.902215926359523,-0.227269801620064,
-0.670378702718353));
#48760=CARTESIAN_POINT('Ctrl Pts',(-0.87482617317514,-0.177024326825049,
-0.705826641853758));
#48761=CARTESIAN_POINT('Ctrl Pts',(-0.861652925570091,-0.144299303100741,
-0.721590372101268));
#48762=CARTESIAN_POINT('Ctrl Pts',(-0.848766861100456,-0.0928409665394229,
-0.736604687327351));
#48763=CARTESIAN_POINT('Ctrl Pts',(-0.84559647055299,-0.0762225747374255,
-0.740223768851063));
#48764=CARTESIAN_POINT('Ctrl Pts',(-0.843383895613249,-0.0595300000000001,
-0.742736168477219));
#48765=CARTESIAN_POINT('',(-0.536443649899847,-0.05953,-0.987512846410683));
#48766=CARTESIAN_POINT('Origin',(0.,-0.05953,0.));
#48767=CARTESIAN_POINT('',(0.0548532617164172,-0.05953,-1.12247250791415));
#48768=CARTESIAN_POINT('Ctrl Pts',(-0.536443649899848,-0.0595300000000001,
-0.987512846410683));
#48769=CARTESIAN_POINT('Ctrl Pts',(-0.533501897135712,-0.0762225747374254,
-0.989110885965947));
#48770=CARTESIAN_POINT('Ctrl Pts',(-0.529268075276156,-0.0928409665394227,
-0.991396466802469));
#48771=CARTESIAN_POINT('Ctrl Pts',(-0.511762781179147,-0.144299303100741,
-1.00061845128527));
#48772=CARTESIAN_POINT('Ctrl Pts',(-0.493462957200432,-0.177024326825049,
-1.0099536580922));
#48773=CARTESIAN_POINT('Ctrl Pts',(-0.45280897844858,-0.227269801620063,
-1.02876878445619));
#48774=CARTESIAN_POINT('Ctrl Pts',(-0.425554672694337,-0.251265615809407,
-1.04048957871266));
#48775=CARTESIAN_POINT('Ctrl Pts',(-0.3787731215897,-0.279889827963178,
-1.05829506364875));
#48776=CARTESIAN_POINT('Ctrl Pts',(-0.354166711873529,-0.290879136862659,
-1.06688848765783));
#48777=CARTESIAN_POINT('Ctrl Pts',(-0.302426893214944,-0.305251990234488,
-1.08269251410343));
#48778=CARTESIAN_POINT('Ctrl Pts',(-0.275287440920027,-0.308638795020976,
-1.0898803575765));
#48779=CARTESIAN_POINT('Ctrl Pts',(-0.224855950742601,-0.308638795020976,
-1.10139101611326));
#48780=CARTESIAN_POINT('Ctrl Pts',(-0.19728546073067,-0.305251990234488,
-1.10669035995599));
#48781=CARTESIAN_POINT('Ctrl Pts',(-0.143812384801039,-0.290879136862659,
-1.11490049012186));
#48782=CARTESIAN_POINT('Ctrl Pts',(-0.117914228755037,-0.279889827963178,
-1.1178344036749));
#48783=CARTESIAN_POINT('Ctrl Pts',(-0.0680399972366989,-0.251265615809407,
-1.12208997038458));
#48784=CARTESIAN_POINT('Ctrl Pts',(-0.0383992541984084,-0.227269801620063,
-1.12335509974011));
#48785=CARTESIAN_POINT('Ctrl Pts',(0.00639229239215326,-0.177024326825049,
-1.12404235695137));
#48786=CARTESIAN_POINT('Ctrl Pts',(0.0269302585198977,-0.144299303100741,
-1.12357162229597));
#48787=CARTESIAN_POINT('Ctrl Pts',(0.04670325263426,-0.0928409665394228,
-1.12285816383385));
#48788=CARTESIAN_POINT('Ctrl Pts',(0.0515094706813703,-0.0762225747374255,
-1.12263591311425));
#48789=CARTESIAN_POINT('Ctrl Pts',(0.0548532617164176,-0.0595300000000001,
-1.12247250791414));
#48790=CARTESIAN_POINT('',(0.437601487681057,-0.05953,-1.03511272300331));
#48791=CARTESIAN_POINT('Origin',(0.,-0.05953,0.));
#48792=CARTESIAN_POINT('',(0.911784794170997,-0.05953,-0.656964154625313));
#48793=CARTESIAN_POINT('Ctrl Pts',(0.437601487681056,-0.0595300000000001,
-1.03511272300331));
#48794=CARTESIAN_POINT('Ctrl Pts',(0.440685038163619,-0.0762225747374255,
-1.03380912944435));
#48795=CARTESIAN_POINT('Ctrl Pts',(0.445111721969657,-0.0928409665394228,
-1.03192403056628));
#48796=CARTESIAN_POINT('Ctrl Pts',(0.463236132117164,-0.144299303100741,
-1.0239876538093));
#48797=CARTESIAN_POINT('Ctrl Pts',(0.481944444320713,-0.177024326825049,
-1.01550068154148));
#48798=CARTESIAN_POINT('Ctrl Pts',(0.522002043615455,-0.227269801620064,
-0.995447160474328));
#48799=CARTESIAN_POINT('Ctrl Pts',(0.548158511259203,-0.251265615809407,
-0.981446681891443));
#48800=CARTESIAN_POINT('Ctrl Pts',(0.591247219971725,-0.279889827963178,
-0.955972930713954));
#48801=CARTESIAN_POINT('Ctrl Pts',(0.613307674922609,-0.290879136862659,
-0.942092777160053));
#48802=CARTESIAN_POINT('Ctrl Pts',(0.657923009631182,-0.305251990234487,
-0.91149460735272));
#48803=CARTESIAN_POINT('Ctrl Pts',(0.680463863683393,-0.308638795020976,
-0.894757676234429));
#48804=CARTESIAN_POINT('Ctrl Pts',(0.720906778729542,-0.308638795020976,
-0.862505527716294));
#48805=CARTESIAN_POINT('Ctrl Pts',(0.742239891936899,-0.305251990234488,
-0.844254137480381));
#48806=CARTESIAN_POINT('Ctrl Pts',(0.781998747691872,-0.290879136862659,
-0.80756613568454));
#48807=CARTESIAN_POINT('Ctrl Pts',(0.800439809856112,-0.279889827963178,
-0.789147407129765));
#48808=CARTESIAN_POINT('Ctrl Pts',(0.834863020612702,-0.251265615809407,
-0.752807465209441));
#48809=CARTESIAN_POINT('Ctrl Pts',(0.854332839576145,-0.227269801620064,
-0.73042219438957));
#48810=CARTESIAN_POINT('Ctrl Pts',(0.882797231409153,-0.177024326825049,
-0.695831250979106));
#48811=CARTESIAN_POINT('Ctrl Pts',(0.895234408667242,-0.144299303100741,
-0.679480524217551));
#48812=CARTESIAN_POINT('Ctrl Pts',(0.907004864562642,-0.0928409665394228,
-0.663576540841106));
#48813=CARTESIAN_POINT('Ctrl Pts',(0.909827729890942,-0.0762225747374256,
-0.659680317203144));
#48814=CARTESIAN_POINT('Ctrl Pts',(0.911784794170998,-0.0595300000000001,
-0.656964154625312));
#48815=CARTESIAN_POINT('',(1.08212377959455,-0.05953,-0.303251606722892));
#48816=CARTESIAN_POINT('Origin',(0.,-0.05953,0.));
#48817=CARTESIAN_POINT('',(1.08212377959455,-0.05953,0.303251606722892));
#48818=CARTESIAN_POINT('Ctrl Pts',(1.08212377959455,-0.0595300000000001,
-0.303251606722892));
#48819=CARTESIAN_POINT('Ctrl Pts',(1.0830271513892,-0.0762225747374255,
-0.300028012588062));
#48820=CARTESIAN_POINT('Ctrl Pts',(1.08431331394788,-0.0928409665394228,
-0.2953917518996));
#48821=CARTESIAN_POINT('Ctrl Pts',(1.08940878963422,-0.144299303100741,
-0.276273267473431));
#48822=CARTESIAN_POINT('Ctrl Pts',(1.09443784939331,-0.177024326825049,
-0.256354979351213));
#48823=CARTESIAN_POINT('Ctrl Pts',(1.10373487993589,-0.227269801620064,
-0.212533521233765));
#48824=CARTESIAN_POINT('Ctrl Pts',(1.10909715583869,-0.251265615809407,
-0.183354415742157));
#48825=CARTESIAN_POINT('Ctrl Pts',(1.1160463456491,-0.279889827963178,-0.133783682657561));
#48826=CARTESIAN_POINT('Ctrl Pts',(1.11894887330541,-0.290879136862659,
-0.107881990270302));
#48827=CARTESIAN_POINT('Ctrl Pts',(1.12284346704144,-0.305251990234488,
-0.0539226701638766));
#48828=CARTESIAN_POINT('Ctrl Pts',(1.123812,-0.308638795020976,-0.025864214957475));
#48829=CARTESIAN_POINT('Ctrl Pts',(1.123812,-0.308638795020976,0.025864214957475));
#48830=CARTESIAN_POINT('Ctrl Pts',(1.12284346704144,-0.305251990234488,
0.0539226701638766));
#48831=CARTESIAN_POINT('Ctrl Pts',(1.11894887330541,-0.290879136862659,
0.107881990270302));
#48832=CARTESIAN_POINT('Ctrl Pts',(1.1160463456491,-0.279889827963178,0.133783682657561));
#48833=CARTESIAN_POINT('Ctrl Pts',(1.10909715583869,-0.251265615809407,
0.183354415742157));
#48834=CARTESIAN_POINT('Ctrl Pts',(1.10373487993589,-0.227269801620064,
0.212533521233765));
#48835=CARTESIAN_POINT('Ctrl Pts',(1.09443784939331,-0.177024326825049,
0.256354979351213));
#48836=CARTESIAN_POINT('Ctrl Pts',(1.08940878963422,-0.144299303100741,
0.276273267473431));
#48837=CARTESIAN_POINT('Ctrl Pts',(1.08431331394788,-0.0928409665394228,
0.2953917518996));
#48838=CARTESIAN_POINT('Ctrl Pts',(1.0830271513892,-0.0762225747374255,
0.300028012588062));
#48839=CARTESIAN_POINT('Ctrl Pts',(1.08212377959455,-0.0595300000000001,
0.303251606722892));
#48840=CARTESIAN_POINT('Origin',(0.,-0.05953,0.));
#48841=CARTESIAN_POINT('Origin',(0.,-0.05953,0.));
#48842=CARTESIAN_POINT('',(0.0589974094846122,-0.05953,1.07456964270265));
#48843=CARTESIAN_POINT('Origin',(0.,-0.05953,0.));
#48844=CARTESIAN_POINT('Origin',(-0.244773027351946,-0.05953,1.07242070340001));
#48845=CARTESIAN_POINT('Origin',(-0.244773027351946,0.,1.07242070340001));
#48846=CARTESIAN_POINT('',(-0.519393123750572,-0.05953,0.942555777842682));
#48847=CARTESIAN_POINT('Ctrl Pts',(-0.519393123750572,-0.05953,0.942555777842682));
#48848=CARTESIAN_POINT('Ctrl Pts',(-0.513714466572041,-0.0925528133349865,
0.945684988399766));
#48849=CARTESIAN_POINT('Ctrl Pts',(-0.503136848051455,-0.124911173756694,
0.951483858396181));
#48850=CARTESIAN_POINT('Ctrl Pts',(-0.47593627990192,-0.177924977804098,
0.965323333309091));
#48851=CARTESIAN_POINT('Ctrl Pts',(-0.460931856495794,-0.199697230012983,
0.972669835243841));
#48852=CARTESIAN_POINT('Ctrl Pts',(-0.426157505475872,-0.237895043532788,
0.988400002689705));
#48853=CARTESIAN_POINT('Ctrl Pts',(-0.406380688682952,-0.254319232363049,
0.996771768218699));
#48854=CARTESIAN_POINT('Ctrl Pts',(-0.364750145543744,-0.28018331644634,
1.01272583306292));
#48855=CARTESIAN_POINT('Ctrl Pts',(-0.340838910881557,-0.29104845371857,
1.02112815447116));
#48856=CARTESIAN_POINT('Ctrl Pts',(-0.290495481564827,-0.30527573347708,
1.036574285215));
#48857=CARTESIAN_POINT('Ctrl Pts',(-0.264056468041074,-0.308638795020976,
1.04359501395068));
#48858=CARTESIAN_POINT('Ctrl Pts',(-0.214892249704082,-0.308638795020976,
1.05481642595959));
#48859=CARTESIAN_POINT('Ctrl Pts',(-0.188025341585962,-0.30527573347708,
1.05996242598502));
#48860=CARTESIAN_POINT('Ctrl Pts',(-0.135965654106109,-0.29104845371857,
1.06788913840721));
#48861=CARTESIAN_POINT('Ctrl Pts',(-0.110776745452494,-0.28018331644634,
1.07069360430242));
#48862=CARTESIAN_POINT('Ctrl Pts',(-0.0663467128214646,-0.254319232363049,
1.07438230428002));
#48863=CARTESIAN_POINT('Ctrl Pts',(-0.0448960436540983,-0.237895043532788,
1.07542044338697));
#48864=CARTESIAN_POINT('Ctrl Pts',(-0.00674037211528124,-0.199697230012983,
1.07633607767727));
#48865=CARTESIAN_POINT('Ctrl Pts',(0.00996567398334777,-0.177924977804098,
1.07622728347683));
#48866=CARTESIAN_POINT('Ctrl Pts',(0.0404772621979741,-0.124911173756694,
1.07556023164702));
#48867=CARTESIAN_POINT('Ctrl Pts',(0.0525234025782719,-0.0925528133349865,
1.07492508698591));
#48868=CARTESIAN_POINT('Ctrl Pts',(0.0589974094846124,-0.05953,1.07456964270265));
#48869=CARTESIAN_POINT('Origin',(-0.244773027351946,-0.05953,1.07242070340001));
#48870=CARTESIAN_POINT('Origin',(0.,-0.05953,0.));
#48871=CARTESIAN_POINT('',(-0.803348093619616,-0.05953,0.716109245731214));
#48872=CARTESIAN_POINT('Origin',(0.,-0.05953,0.));
#48873=CARTESIAN_POINT('Origin',(-0.991065754692661,-0.05953,0.477272113029314));
#48874=CARTESIAN_POINT('Origin',(-0.991065754692661,0.,0.477272113029314));
#48875=CARTESIAN_POINT('',(-1.06075609691358,-0.05953,0.181596019242328));
#48876=CARTESIAN_POINT('Ctrl Pts',(-1.06075609691358,-0.05953,0.181596019242328));
#48877=CARTESIAN_POINT('Ctrl Pts',(-1.05966202740332,-0.0925528133349865,
0.187986803072856));
#48878=CARTESIAN_POINT('Ctrl Pts',(-1.05760072925372,-0.124911173756694,
0.199872254546857));
#48879=CARTESIAN_POINT('Ctrl Pts',(-1.05146158959546,-0.177924977804098,
0.22976728653846));
#48880=CARTESIAN_POINT('Ctrl Pts',(-1.04785021111757,-0.199697230012983,
0.246078686169301));
#48881=CARTESIAN_POINT('Ctrl Pts',(-1.03846709802406,-0.237895043532788,
0.283073967563097));
#48882=CARTESIAN_POINT('Ctrl Pts',(-1.03268176429485,-0.254319232363049,
0.303755815985685));
#48883=CARTESIAN_POINT('Ctrl Pts',(-1.01919893537026,-0.28018331644634,
0.346251081972725));
#48884=CARTESIAN_POINT('Ctrl Pts',(-1.01085972381132,-0.29104845371857,
0.370184399726282));
#48885=CARTESIAN_POINT('Ctrl Pts',(-0.99154738033959,-0.30527573347708,
0.419174982698463));
#48886=CARTESIAN_POINT('Ctrl Pts',(-0.980551951791748,-0.308638795020976,
0.444223188605045));
#48887=CARTESIAN_POINT('Ctrl Pts',(-0.958671816228589,-0.308638795020976,
0.489657758261848));
#48888=CARTESIAN_POINT('Ctrl Pts',(-0.945943877838127,-0.30527573347708,
0.51387163140139));
#48889=CARTESIAN_POINT('Ctrl Pts',(-0.91968254693063,-0.29104845371857,
0.559515758398093));
#48890=CARTESIAN_POINT('Ctrl Pts',(-0.906170138993533,-0.28018331644634,
0.580957796077825));
#48891=CARTESIAN_POINT('Ctrl Pts',(-0.8813524085237,-0.254319232363049,
0.617994461173994));
#48892=CARTESIAN_POINT('Ctrl Pts',(-0.868789784891799,-0.237895043532788,
0.635412538795143));
#48893=CARTESIAN_POINT('Ctrl Pts',(-0.845715984518854,-0.199697230012983,
0.66581473268113));
#48894=CARTESIAN_POINT('Ctrl Pts',(-0.835214876415962,-0.177924977804098,
0.678808213394124));
#48895=CARTESIAN_POINT('Ctrl Pts',(-0.815669690204649,-0.124911173756694,
0.702247233627224));
#48896=CARTESIAN_POINT('Ctrl Pts',(-0.807662468433796,-0.0925528133349865,
0.711269279199861));
#48897=CARTESIAN_POINT('Ctrl Pts',(-0.803348093619616,-0.05953,0.716109245731214));
#48898=CARTESIAN_POINT('Origin',(-0.991065754692661,-0.05953,0.477272113029314));
#48899=CARTESIAN_POINT('Origin',(0.,-0.05953,0.));
#48900=CARTESIAN_POINT('',(-1.076188,-0.05953,1.31795018948079E-16));
#48901=CARTESIAN_POINT('Origin',(0.,-0.05953,0.));
#48902=CARTESIAN_POINT('',(-1.06075609691358,-0.05953,-0.181596019242328));
#48903=CARTESIAN_POINT('Origin',(0.,-0.05953,0.));
#48904=CARTESIAN_POINT('Origin',(-0.991065754692661,-0.05953,-0.477272113029314));
#48905=CARTESIAN_POINT('Origin',(-0.991065754692661,0.,-0.477272113029314));
#48906=CARTESIAN_POINT('',(-0.803348093619616,-0.05953,-0.716109245731215));
#48907=CARTESIAN_POINT('Ctrl Pts',(-0.803348093619616,-0.05953,-0.716109245731215));
#48908=CARTESIAN_POINT('Ctrl Pts',(-0.807662468433795,-0.0925528133349865,
-0.711269279199862));
#48909=CARTESIAN_POINT('Ctrl Pts',(-0.815669690204649,-0.124911173756694,
-0.702247233627224));
#48910=CARTESIAN_POINT('Ctrl Pts',(-0.835214876415962,-0.177924977804098,
-0.678808213394124));
#48911=CARTESIAN_POINT('Ctrl Pts',(-0.845715984518854,-0.199697230012983,
-0.66581473268113));
#48912=CARTESIAN_POINT('Ctrl Pts',(-0.868789784891799,-0.237895043532788,
-0.635412538795143));
#48913=CARTESIAN_POINT('Ctrl Pts',(-0.8813524085237,-0.254319232363049,
-0.617994461173994));
#48914=CARTESIAN_POINT('Ctrl Pts',(-0.906170138993533,-0.28018331644634,
-0.580957796077826));
#48915=CARTESIAN_POINT('Ctrl Pts',(-0.91968254693063,-0.29104845371857,
-0.559515758398093));
#48916=CARTESIAN_POINT('Ctrl Pts',(-0.945943877838127,-0.30527573347708,
-0.51387163140139));
#48917=CARTESIAN_POINT('Ctrl Pts',(-0.958671816228589,-0.308638795020976,
-0.489657758261848));
#48918=CARTESIAN_POINT('Ctrl Pts',(-0.980551951791748,-0.308638795020976,
-0.444223188605045));
#48919=CARTESIAN_POINT('Ctrl Pts',(-0.99154738033959,-0.30527573347708,
-0.419174982698463));
#48920=CARTESIAN_POINT('Ctrl Pts',(-1.01085972381132,-0.29104845371857,
-0.370184399726282));
#48921=CARTESIAN_POINT('Ctrl Pts',(-1.01919893537026,-0.28018331644634,
-0.346251081972725));
#48922=CARTESIAN_POINT('Ctrl Pts',(-1.03268176429485,-0.254319232363049,
-0.303755815985685));
#48923=CARTESIAN_POINT('Ctrl Pts',(-1.03846709802406,-0.237895043532788,
-0.283073967563097));
#48924=CARTESIAN_POINT('Ctrl Pts',(-1.04785021111757,-0.199697230012983,
-0.246078686169302));
#48925=CARTESIAN_POINT('Ctrl Pts',(-1.05146158959546,-0.177924977804098,
-0.229767286538461));
#48926=CARTESIAN_POINT('Ctrl Pts',(-1.05760072925372,-0.124911173756694,
-0.199872254546858));
#48927=CARTESIAN_POINT('Ctrl Pts',(-1.05966202740332,-0.0925528133349864,
-0.187986803072857));
#48928=CARTESIAN_POINT('Ctrl Pts',(-1.06075609691358,-0.05953,-0.181596019242328));
#48929=CARTESIAN_POINT('Origin',(-0.991065754692661,-0.05953,-0.477272113029314));
#48930=CARTESIAN_POINT('Origin',(0.,-0.05953,0.));
#48931=CARTESIAN_POINT('',(-0.519393123750572,-0.05953,-0.942555777842682));
#48932=CARTESIAN_POINT('Origin',(0.,-0.05953,0.));
#48933=CARTESIAN_POINT('Origin',(-0.244773027351946,-0.05953,-1.07242070340001));
#48934=CARTESIAN_POINT('Origin',(-0.244773027351946,0.,-1.07242070340001));
#48935=CARTESIAN_POINT('',(0.0589974094846125,-0.05953,-1.07456964270265));
#48936=CARTESIAN_POINT('Ctrl Pts',(0.0589974094846127,-0.05953,-1.07456964270265));
#48937=CARTESIAN_POINT('Ctrl Pts',(0.0525234025782722,-0.0925528133349865,
-1.07492508698591));
#48938=CARTESIAN_POINT('Ctrl Pts',(0.0404772621979744,-0.124911173756694,
-1.07556023164702));
#48939=CARTESIAN_POINT('Ctrl Pts',(0.0099656739833481,-0.177924977804098,
-1.07622728347683));
#48940=CARTESIAN_POINT('Ctrl Pts',(-0.00674037211528096,-0.199697230012983,
-1.07633607767727));
#48941=CARTESIAN_POINT('Ctrl Pts',(-0.044896043654098,-0.237895043532788,
-1.07542044338697));
#48942=CARTESIAN_POINT('Ctrl Pts',(-0.0663467128214644,-0.254319232363049,
-1.07438230428002));
#48943=CARTESIAN_POINT('Ctrl Pts',(-0.110776745452493,-0.28018331644634,
-1.07069360430242));
#48944=CARTESIAN_POINT('Ctrl Pts',(-0.135965654106109,-0.29104845371857,
-1.06788913840721));
#48945=CARTESIAN_POINT('Ctrl Pts',(-0.188025341585962,-0.30527573347708,
-1.05996242598502));
#48946=CARTESIAN_POINT('Ctrl Pts',(-0.214892249704082,-0.308638795020976,
-1.05481642595959));
#48947=CARTESIAN_POINT('Ctrl Pts',(-0.264056468041074,-0.308638795020976,
-1.04359501395068));
#48948=CARTESIAN_POINT('Ctrl Pts',(-0.290495481564827,-0.30527573347708,
-1.036574285215));
#48949=CARTESIAN_POINT('Ctrl Pts',(-0.340838910881557,-0.291048453718569,
-1.02112815447116));
#48950=CARTESIAN_POINT('Ctrl Pts',(-0.364750145543744,-0.28018331644634,
-1.01272583306292));
#48951=CARTESIAN_POINT('Ctrl Pts',(-0.406380688682952,-0.254319232363049,
-0.996771768218699));
#48952=CARTESIAN_POINT('Ctrl Pts',(-0.426157505475872,-0.237895043532788,
-0.988400002689705));
#48953=CARTESIAN_POINT('Ctrl Pts',(-0.460931856495794,-0.199697230012983,
-0.972669835243841));
#48954=CARTESIAN_POINT('Ctrl Pts',(-0.475936279901919,-0.177924977804098,
-0.965323333309091));
#48955=CARTESIAN_POINT('Ctrl Pts',(-0.503136848051454,-0.124911173756694,
-0.951483858396181));
#48956=CARTESIAN_POINT('Ctrl Pts',(-0.513714466572041,-0.0925528133349865,
-0.945684988399766));
#48957=CARTESIAN_POINT('Ctrl Pts',(-0.519393123750572,-0.05953,-0.942555777842682));
#48958=CARTESIAN_POINT('Origin',(-0.244773027351946,-0.05953,-1.07242070340001));
#48959=CARTESIAN_POINT('Origin',(0.,-0.05953,0.));
#48960=CARTESIAN_POINT('',(0.413083465285518,-0.05953,-0.993751811093549));
#48961=CARTESIAN_POINT('Origin',(0.,-0.05953,0.));
#48962=CARTESIAN_POINT('Origin',(0.685838782044607,-0.05953,-0.860014630714833));
#48963=CARTESIAN_POINT('Origin',(0.685838782044607,0.,-0.860014630714833));
#48964=CARTESIAN_POINT('',(0.876916659919095,-0.05953,-0.623857181492959));
#48965=CARTESIAN_POINT('Ctrl Pts',(0.876916659919095,-0.05953,-0.623857181492958));
#48966=CARTESIAN_POINT('Ctrl Pts',(0.873158080166742,-0.0925528133349865,
-0.62914037979579));
#48967=CARTESIAN_POINT('Ctrl Pts',(0.866144010579847,-0.124911173756694,
-0.638954437806245));
#48968=CARTESIAN_POINT('Ctrl Pts',(0.847641868610495,-0.177924977804098,
-0.663225258065736));
#48969=CARTESIAN_POINT('Ctrl Pts',(0.837310877969633,-0.199697230012983,
-0.676354402927683));
#48970=CARTESIAN_POINT('Ctrl Pts',(0.81280533416753,-0.237895043532788,
-0.705614819529209));
#48971=CARTESIAN_POINT('Ctrl Pts',(0.798619410861634,-0.254319232363049,
-0.721738358858166));
#48972=CARTESIAN_POINT('Ctrl Pts',(0.768033796848072,-0.28018331644634,
-0.754175290318038));
#48973=CARTESIAN_POINT('Ctrl Pts',(0.750136149454208,-0.29104845371857,
-0.772120216227122));
#48974=CARTESIAN_POINT('Ctrl Pts',(0.711480111898423,-0.30527573347708,
-0.807879894508811));
#48975=CARTESIAN_POINT('Ctrl Pts',(0.690705563850638,-0.308638795020976,
-0.825676810575913));
#48976=CARTESIAN_POINT('Ctrl Pts',(0.651278921914856,-0.308638795020976,
-0.857118508332695));
#48977=CARTESIAN_POINT('Ctrl Pts',(0.629305439856167,-0.30527573347708,
-0.873412008702649));
#48978=CARTESIAN_POINT('Ctrl Pts',(0.585840553788742,-0.29104845371857,
-0.903141581680914));
#48979=CARTESIAN_POINT('Ctrl Pts',(0.564362943424239,-0.28018331644634,
-0.916597376014514));
#48980=CARTESIAN_POINT('Ctrl Pts',(0.525933334162556,-0.254319232363049,
-0.939198248544427));
#48981=CARTESIAN_POINT('Ctrl Pts',(0.507057380724533,-0.237895043532788,
-0.949440676105255));
#48982=CARTESIAN_POINT('Ctrl Pts',(0.473077587363686,-0.199697230012983,
-0.966820759530997));
#48983=CARTESIAN_POINT('Ctrl Pts',(0.457978755888596,-0.177924977804098,
-0.973971221090534));
#48984=CARTESIAN_POINT('Ctrl Pts',(0.430199341854858,-0.124911173756694,
-0.986608710139579));
#48985=CARTESIAN_POINT('Ctrl Pts',(0.419070565453384,-0.0925528133349865,
-0.991263089003441));
#48986=CARTESIAN_POINT('Ctrl Pts',(0.413083465285518,-0.05953,-0.993751811093549));
#48987=CARTESIAN_POINT('Origin',(0.685838782044607,-0.05953,-0.860014630714833));
#48988=CARTESIAN_POINT('Origin',(0.,-0.208355,0.));
#48989=CARTESIAN_POINT('',(-1.076188,-0.35718,1.31795018948079E-16));
#48990=CARTESIAN_POINT('Origin',(0.,-0.35718,0.));
#48991=CARTESIAN_POINT('',(-1.076188,-0.208355,1.31795018948079E-16));
#48992=CARTESIAN_POINT('',(1.03449977959455,-0.05953,0.296632461748266));
#48993=CARTESIAN_POINT('Origin',(0.,-0.05953,0.));
#48994=CARTESIAN_POINT('',(1.03449977959455,-0.05953,-0.296632461748266));
#48995=CARTESIAN_POINT('Ctrl Pts',(1.03449977959455,-0.05953,0.296632461748267));
#48996=CARTESIAN_POINT('Ctrl Pts',(1.03628691421076,-0.0925528133349865,
0.290399865505497));
#48997=CARTESIAN_POINT('Ctrl Pts',(1.03958665287714,-0.124911173756694,
0.278797079997872));
#48998=CARTESIAN_POINT('Ctrl Pts',(1.0470264474309,-0.177924977804098,0.249198913998601));
#48999=CARTESIAN_POINT('Ctrl Pts',(1.05084995891418,-0.199697230012983,
0.232935932341942));
#49000=CARTESIAN_POINT('Ctrl Pts',(1.05844771715377,-0.237895043532788,
0.195533155353269));
#49001=CARTESIAN_POINT('Ctrl Pts',(1.06220882929878,-0.254319232363049,
0.17438929156337));
#49002=CARTESIAN_POINT('Ctrl Pts',(1.06849922508772,-0.28018331644634,0.130252399648131));
#49003=CARTESIAN_POINT('Ctrl Pts',(1.07137013248666,-0.29104845371857,0.105070977154072));
#49004=CARTESIAN_POINT('Ctrl Pts',(1.07522652957392,-0.30527573347708,0.0525526752791107));
#49005=CARTESIAN_POINT('Ctrl Pts',(1.076188,-0.308638795020976,0.025214283908933));
#49006=CARTESIAN_POINT('Ctrl Pts',(1.076188,-0.308638795020976,-0.025214283908933));
#49007=CARTESIAN_POINT('Ctrl Pts',(1.07522652957392,-0.30527573347708,-0.0525526752791107));
#49008=CARTESIAN_POINT('Ctrl Pts',(1.07137013248666,-0.29104845371857,-0.105070977154072));
#49009=CARTESIAN_POINT('Ctrl Pts',(1.06849922508772,-0.28018331644634,-0.130252399648131));
#49010=CARTESIAN_POINT('Ctrl Pts',(1.06220882929878,-0.254319232363049,
-0.17438929156337));
#49011=CARTESIAN_POINT('Ctrl Pts',(1.05844771715377,-0.237895043532788,
-0.195533155353269));
#49012=CARTESIAN_POINT('Ctrl Pts',(1.05084995891418,-0.199697230012983,
-0.232935932341942));
#49013=CARTESIAN_POINT('Ctrl Pts',(1.0470264474309,-0.177924977804098,-0.249198913998601));
#49014=CARTESIAN_POINT('Ctrl Pts',(1.03958665287714,-0.124911173756694,
-0.278797079997872));
#49015=CARTESIAN_POINT('Ctrl Pts',(1.03628691421076,-0.0925528133349865,
-0.290399865505497));
#49016=CARTESIAN_POINT('Ctrl Pts',(1.03449977959455,-0.05953,-0.296632461748267));
#49017=CARTESIAN_POINT('Origin',(0.,-0.05953,0.));
#49018=CARTESIAN_POINT('Origin',(0.,-0.05953,0.));
#49019=CARTESIAN_POINT('Origin',(1.1,-0.05953,0.));
#49020=CARTESIAN_POINT('Origin',(1.1,0.,0.));
#49021=CARTESIAN_POINT('Origin',(1.1,-0.05953,0.));
#49022=CARTESIAN_POINT('Origin',(0.,-0.35718,0.));
#49023=CARTESIAN_POINT('Origin',(0.,-0.05953,0.));
#49024=CARTESIAN_POINT('',(0.,0.,0.));
#49025=CARTESIAN_POINT('Origin',(1.119765,0.495,0.));
#49026=CARTESIAN_POINT('',(-1.119765,0.495,-1.37131662304724E-16));
#49027=CARTESIAN_POINT('Origin',(0.,0.495,0.));
#49028=CARTESIAN_POINT('',(-1.085235,0.495,-1.32902956907268E-16));
#49029=CARTESIAN_POINT('Origin',(0.,0.495,0.));
#49030=CARTESIAN_POINT('Origin',(0.,0.4575,0.));
#49031=CARTESIAN_POINT('',(-1.119765,0.42,-1.37131662304724E-16));
#49032=CARTESIAN_POINT('Origin',(0.,0.42,0.));
#49033=CARTESIAN_POINT('',(-1.119765,0.4575,-1.37131662304724E-16));
#49034=CARTESIAN_POINT('Origin',(1.085235,0.42,0.));
#49035=CARTESIAN_POINT('',(-1.085235,0.42,-1.32902956907268E-16));
#49036=CARTESIAN_POINT('Origin',(0.,0.42,0.));
#49037=CARTESIAN_POINT('Origin',(0.,0.4575,0.));
#49038=CARTESIAN_POINT('',(-1.085235,0.4575,-1.32902956907268E-16));
#49039=CARTESIAN_POINT('Origin',(1.119765,-0.42,0.));
#49040=CARTESIAN_POINT('',(-1.119765,-0.42,-1.37131662304724E-16));
#49041=CARTESIAN_POINT('Origin',(0.,-0.42,0.));
#49042=CARTESIAN_POINT('',(-1.085235,-0.42,-1.32902956907268E-16));
#49043=CARTESIAN_POINT('Origin',(0.,-0.42,0.));
#49044=CARTESIAN_POINT('Origin',(0.,-0.4575,0.));
#49045=CARTESIAN_POINT('',(-1.119765,-0.495,-1.37131662304724E-16));
#49046=CARTESIAN_POINT('Origin',(0.,-0.495,0.));
#49047=CARTESIAN_POINT('',(-1.119765,-0.4575,-1.37131662304724E-16));
#49048=CARTESIAN_POINT('Origin',(1.085235,-0.495,0.));
#49049=CARTESIAN_POINT('',(-1.085235,-0.495,-1.32902956907268E-16));
#49050=CARTESIAN_POINT('Origin',(0.,-0.495,0.));
#49051=CARTESIAN_POINT('Origin',(0.,-0.4575,0.));
#49052=CARTESIAN_POINT('',(-1.085235,-0.4575,-1.32902956907268E-16));
#49053=CARTESIAN_POINT('',(0.,0.,0.));
#49054=CARTESIAN_POINT('',(0.,0.,0.));
#49055=CARTESIAN_POINT('',(0.,0.,0.));
#49056=CARTESIAN_POINT('',(0.,0.,0.));
#49057=CARTESIAN_POINT('',(0.,0.,0.));
#49058=CARTESIAN_POINT('',(0.,0.,0.));
#49059=CARTESIAN_POINT('',(0.,0.,0.));
#49060=CARTESIAN_POINT('Origin',(0.,0.,0.));
#49061=CARTESIAN_POINT('',(-1.63531,-0.410863395882378,-2.00267715711366E-16));
#49062=CARTESIAN_POINT('',(-2.00267715711366E-16,-0.410863395882378,1.63531));
#49063=CARTESIAN_POINT('Origin',(0.,-0.410863395882378,0.));
#49064=CARTESIAN_POINT('Origin',(0.,-0.410863395882378,0.));
#49065=CARTESIAN_POINT('',(-2.00267715711366E-16,0.410863395882378,1.63531));
#49066=CARTESIAN_POINT('Origin',(-2.05128338857182E-16,0.,1.675));
#49067=CARTESIAN_POINT('',(-1.63531,0.410863395882378,2.00267715711366E-16));
#49068=CARTESIAN_POINT('Origin',(0.,0.410863395882378,0.));
#49069=CARTESIAN_POINT('Origin',(0.,0.410863395882378,0.));
#49070=CARTESIAN_POINT('Origin',(0.,0.,0.));
#49071=CARTESIAN_POINT('',(-1.63531,0.7,-2.00267715711366E-16));
#49072=CARTESIAN_POINT('',(-1.63531,0.,-2.00267715711366E-16));
#49073=CARTESIAN_POINT('Origin',(0.,0.7,0.));
#49074=CARTESIAN_POINT('Origin',(0.,0.,0.));
#49075=CARTESIAN_POINT('',(-1.,-0.6,-1.22464679914735E-16));
#49076=CARTESIAN_POINT('Origin',(0.,-0.6,0.));
#49077=CARTESIAN_POINT('',(-1.,0.6,-1.22464679914735E-16));
#49078=CARTESIAN_POINT('',(-1.,0.,-1.22464679914735E-16));
#49079=CARTESIAN_POINT('Origin',(0.,0.6,0.));
#49080=CARTESIAN_POINT('Origin',(0.,0.65,0.));
#49081=CARTESIAN_POINT('',(-1.1,0.7,-1.34711147906209E-16));
#49082=CARTESIAN_POINT('',(-1.05,0.65,-1.28587913910472E-16));
#49083=CARTESIAN_POINT('Origin',(0.,0.7,0.));
#49084=CARTESIAN_POINT('Origin',(1.63531,0.7,0.));
#49085=CARTESIAN_POINT('Origin',(0.,0.,0.));
#49086=CARTESIAN_POINT('',(-1.63531,-0.7,-2.00267715711366E-16));
#49087=CARTESIAN_POINT('Origin',(0.,-0.7,0.));
#49088=CARTESIAN_POINT('',(-1.63531,0.,-2.00267715711366E-16));
#49089=CARTESIAN_POINT('Origin',(1.1,-0.7,0.));
#49090=CARTESIAN_POINT('',(-1.1,-0.7,-1.34711147906209E-16));
#49091=CARTESIAN_POINT('Origin',(0.,-0.7,0.));
#49092=CARTESIAN_POINT('Origin',(0.,-0.65,0.));
#49093=CARTESIAN_POINT('',(-1.05,-0.65,-1.28587913910472E-16));
#49094=CARTESIAN_POINT('',(0.,0.,0.));
#49095=CARTESIAN_POINT('Origin',(0.,0.,0.));
#49096=CARTESIAN_POINT('',(-1.71469,0.410863395882378,-2.09988962002998E-16));
#49097=CARTESIAN_POINT('',(-2.09988962002998E-16,0.410863395882378,1.71469));
#49098=CARTESIAN_POINT('Origin',(0.,0.410863395882378,0.));
#49099=CARTESIAN_POINT('Origin',(0.,0.410863395882378,0.));
#49100=CARTESIAN_POINT('',(-2.09988962002998E-16,-0.410863395882378,1.71469));
#49101=CARTESIAN_POINT('Origin',(-2.05128338857182E-16,0.,1.675));
#49102=CARTESIAN_POINT('',(-1.71469,-0.410863395882378,2.09988962002998E-16));
#49103=CARTESIAN_POINT('Origin',(0.,-0.410863395882378,0.));
#49104=CARTESIAN_POINT('Origin',(0.,-0.410863395882378,0.));
#49105=CARTESIAN_POINT('Origin',(0.,0.,0.));
#49106=CARTESIAN_POINT('',(-1.71469,-0.7,-2.09988962002998E-16));
#49107=CARTESIAN_POINT('Origin',(0.,-0.7,0.));
#49108=CARTESIAN_POINT('',(-1.71469,0.,-2.09988962002998E-16));
#49109=CARTESIAN_POINT('Origin',(2.25,0.7,0.));
#49110=CARTESIAN_POINT('',(-2.25,0.7,-2.75545529808154E-16));
#49111=CARTESIAN_POINT('Origin',(0.,0.7,0.));
#49112=CARTESIAN_POINT('',(-1.71469,0.7,-2.09988962002998E-16));
#49113=CARTESIAN_POINT('Origin',(0.,0.7,0.));
#49114=CARTESIAN_POINT('Origin',(0.,0.65,0.));
#49115=CARTESIAN_POINT('',(-2.35,0.6,-2.87791997799628E-16));
#49116=CARTESIAN_POINT('Origin',(0.,0.6,0.));
#49117=CARTESIAN_POINT('',(-2.3,0.65,-2.81668763803891E-16));
#49118=CARTESIAN_POINT('Origin',(0.,0.,0.));
#49119=CARTESIAN_POINT('',(-2.35,-0.6,-2.87791997799628E-16));
#49120=CARTESIAN_POINT('Origin',(0.,-0.6,0.));
#49121=CARTESIAN_POINT('',(-2.35,0.,-2.87791997799628E-16));
#49122=CARTESIAN_POINT('Origin',(0.,-0.65,0.));
#49123=CARTESIAN_POINT('',(-2.25,-0.7,-2.75545529808154E-16));
#49124=CARTESIAN_POINT('Origin',(0.,-0.7,0.));
#49125=CARTESIAN_POINT('',(-2.3,-0.65,-2.81668763803891E-16));
#49126=CARTESIAN_POINT('Origin',(1.71469,-0.7,0.));
#49127=CARTESIAN_POINT('Origin',(0.,0.,0.));
#49128=CARTESIAN_POINT('',(-1.71469,0.,-2.09988962002998E-16));
#49129=CARTESIAN_POINT('',(0.,0.,0.));
#49130=CARTESIAN_POINT('Origin',(1.675,0.,0.));
#49131=CARTESIAN_POINT('',(1.675,-2.97627328869245E-33,0.3969));
#49132=CARTESIAN_POINT('',(1.675,-2.97627328869245E-33,-0.3969));
#49133=CARTESIAN_POINT('Origin',(1.675,0.,0.));
#49134=CARTESIAN_POINT('Origin',(1.18440385848747,0.,-1.18440385848747));
#49135=CARTESIAN_POINT('',(1.46505453994041,3.1867025333467E-33,-0.903753177034526));
#49136=CARTESIAN_POINT('',(0.903753177034527,-9.13924911073161E-33,-1.46505453994041));
#49137=CARTESIAN_POINT('Origin',(1.18440385848747,0.,-1.18440385848747));
#49138=CARTESIAN_POINT('Origin',(1.02564169428591E-16,0.,-1.675));
#49139=CARTESIAN_POINT('',(0.3969,-2.97627328869246E-33,-1.675));
#49140=CARTESIAN_POINT('',(-0.3969,-2.97627328869245E-33,-1.675));
#49141=CARTESIAN_POINT('Origin',(1.02564169428591E-16,0.,-1.675));
#49142=CARTESIAN_POINT('Origin',(-1.18440385848747,0.,-1.18440385848747));
#49143=CARTESIAN_POINT('',(-0.903753177034526,3.1867025333467E-33,-1.46505453994041));
#49144=CARTESIAN_POINT('',(-1.46505453994041,-9.13924911073161E-33,-0.903753177034527));
#49145=CARTESIAN_POINT('Origin',(-1.18440385848747,0.,-1.18440385848747));
#49146=CARTESIAN_POINT('Origin',(-1.675,0.,-2.05128338857182E-16));
#49147=CARTESIAN_POINT('',(-1.675,-2.97627328869246E-33,-0.3969));
#49148=CARTESIAN_POINT('',(-1.675,-2.97627328869245E-33,0.3969));
#49149=CARTESIAN_POINT('Origin',(-1.675,0.,-2.05128338857182E-16));
#49150=CARTESIAN_POINT('Origin',(-1.18440385848747,0.,1.18440385848747));
#49151=CARTESIAN_POINT('',(-1.46505453994041,6.26819044436628E-33,0.903753177034526));
#49152=CARTESIAN_POINT('',(-0.903753177034527,-1.22207370217512E-32,1.46505453994041));
#49153=CARTESIAN_POINT('Origin',(-1.18440385848747,0.,1.18440385848747));
#49154=CARTESIAN_POINT('Origin',(-3.07692508285772E-16,0.,1.675));
#49155=CARTESIAN_POINT('',(-0.3969,-2.97627328869246E-33,1.675));
#49156=CARTESIAN_POINT('',(0.396899999999999,-2.97627328869245E-33,1.675));
#49157=CARTESIAN_POINT('Origin',(-3.07692508285772E-16,0.,1.675));
#49158=CARTESIAN_POINT('Origin',(1.18440385848747,0.,1.18440385848747));
#49159=CARTESIAN_POINT('',(0.903753177034526,9.34967835538585E-33,1.46505453994041));
#49160=CARTESIAN_POINT('',(1.46505453994041,-1.53022249327708E-32,0.903753177034527));
#49161=CARTESIAN_POINT('Origin',(1.18440385848747,0.,1.18440385848747));
#49162=CARTESIAN_POINT('',(0.,0.,0.));
#49163=CARTESIAN_POINT('Origin',(1.18440385848747,0.,1.18440385848747));
#49164=CARTESIAN_POINT('',(0.846804978391753,-0.07938,1.40825612658882));
#49165=CARTESIAN_POINT('',(1.40825612658882,-0.07938,0.846804978391754));
#49166=CARTESIAN_POINT('Ctrl Pts',(0.846804978391752,-0.0793800000000001,
1.40825612658882));
#49167=CARTESIAN_POINT('Ctrl Pts',(0.854205272175554,-0.123401821157026,
1.40380622184538));
#49168=CARTESIAN_POINT('Ctrl Pts',(0.867957148219441,-0.166543350814306,
1.39550172959303));
#49169=CARTESIAN_POINT('Ctrl Pts',(0.902193646979982,-0.237231147975234,
1.3735491215176));
#49170=CARTESIAN_POINT('Ctrl Pts',(0.920778333482564,-0.266264900654909,
1.36127834356734));
#49171=CARTESIAN_POINT('Ctrl Pts',(0.962485392528369,-0.317195968905306,
1.33211611256184));
#49172=CARTESIAN_POINT('Ctrl Pts',(0.985600426557816,-0.33909093068465,
1.31521005565926));
#49173=CARTESIAN_POINT('Ctrl Pts',(1.03253285680459,-0.373586846396559,
1.27866649102984));
#49174=CARTESIAN_POINT('Ctrl Pts',(1.05871835910697,-0.388086240756494,
1.25722555095714));
#49175=CARTESIAN_POINT('Ctrl Pts',(1.11153475808518,-0.407068917407805,
1.2107812086231));
#49176=CARTESIAN_POINT('Ctrl Pts',(1.13814686046673,-0.411552957311693,
1.18575674747573));
#49177=CARTESIAN_POINT('Ctrl Pts',(1.18575674747573,-0.411552957311693,
1.13814686046673));
#49178=CARTESIAN_POINT('Ctrl Pts',(1.2107812086231,-0.407068917407805,1.11153475808518));
#49179=CARTESIAN_POINT('Ctrl Pts',(1.25722555095713,-0.388086240756494,
1.05871835910697));
#49180=CARTESIAN_POINT('Ctrl Pts',(1.27866649102984,-0.373586846396559,
1.03253285680459));
#49181=CARTESIAN_POINT('Ctrl Pts',(1.31521005565926,-0.33909093068465,0.985600426557816));
#49182=CARTESIAN_POINT('Ctrl Pts',(1.33211611256184,-0.317195968905306,
0.962485392528369));
#49183=CARTESIAN_POINT('Ctrl Pts',(1.36127834356734,-0.266264900654909,
0.920778333482565));
#49184=CARTESIAN_POINT('Ctrl Pts',(1.3735491215176,-0.237231147975234,0.902193646979983));
#49185=CARTESIAN_POINT('Ctrl Pts',(1.39550172959303,-0.166543350814306,
0.867957148219442));
#49186=CARTESIAN_POINT('Ctrl Pts',(1.40380622184538,-0.123401821157026,
0.854205272175555));
#49187=CARTESIAN_POINT('Ctrl Pts',(1.40825612658882,-0.0793800000000001,
0.846804978391753));
#49188=CARTESIAN_POINT('',(0.886256117232623,-0.07938,1.45861320581289));
#49189=CARTESIAN_POINT('Origin',(1.18440385848747,-0.07938,1.18440385848747));
#49190=CARTESIAN_POINT('',(1.45861320581289,-0.07938,0.886256117232624));
#49191=CARTESIAN_POINT('Ctrl Pts',(1.45861320581289,-0.0793800000000001,
0.886256117232623));
#49192=CARTESIAN_POINT('Ctrl Pts',(1.45630208793976,-0.101649918886749,
0.890059788636852));
#49193=CARTESIAN_POINT('Ctrl Pts',(1.45296717977858,-0.123823518623746,
0.895520212222107));
#49194=CARTESIAN_POINT('Ctrl Pts',(1.43904931717599,-0.192480977588836,
0.917859913453975));
#49195=CARTESIAN_POINT('Ctrl Pts',(1.4243271592157,-0.236152929235938,0.940896403863072));
#49196=CARTESIAN_POINT('Ctrl Pts',(1.39055359345152,-0.303141259068212,
0.990027513266106));
#49197=CARTESIAN_POINT('Ctrl Pts',(1.36743459453896,-0.335108247315849,
1.02199477007745));
#49198=CARTESIAN_POINT('Ctrl Pts',(1.32643091652006,-0.373243761060364,
1.07446535104584));
#49199=CARTESIAN_POINT('Ctrl Pts',(1.30441816675528,-0.387888272594439,
1.10126842659597));
#49200=CARTESIAN_POINT('Ctrl Pts',(1.25681160160691,-0.407041111792943,
1.15530234155453));
#49201=CARTESIAN_POINT('Ctrl Pts',(1.23119764287622,-0.411552957311693,
1.18251418313119));
#49202=CARTESIAN_POINT('Ctrl Pts',(1.18251418313119,-0.411552957311693,
1.23119764287622));
#49203=CARTESIAN_POINT('Ctrl Pts',(1.15530234155453,-0.407041111792943,
1.25681160160691));
#49204=CARTESIAN_POINT('Ctrl Pts',(1.10126842659597,-0.387888272594439,
1.30441816675528));
#49205=CARTESIAN_POINT('Ctrl Pts',(1.07446535104584,-0.373243761060364,
1.32643091652006));
#49206=CARTESIAN_POINT('Ctrl Pts',(1.02199477007745,-0.335108247315848,
1.36743459453896));
#49207=CARTESIAN_POINT('Ctrl Pts',(0.990027513266105,-0.303141259068211,
1.39055359345152));
#49208=CARTESIAN_POINT('Ctrl Pts',(0.940896403863071,-0.236152929235937,
1.42432715921571));
#49209=CARTESIAN_POINT('Ctrl Pts',(0.917859913453974,-0.192480977588835,
1.43904931717599));
#49210=CARTESIAN_POINT('Ctrl Pts',(0.895520212222106,-0.123823518623745,
1.45296717977858));
#49211=CARTESIAN_POINT('Ctrl Pts',(0.890059788636851,-0.101649918886749,
1.45630208793976));
#49212=CARTESIAN_POINT('Ctrl Pts',(0.886256117232622,-0.0793800000000001,
1.45861320581289));
#49213=CARTESIAN_POINT('Origin',(1.18440385848747,-0.07938,1.18440385848747));
#49214=CARTESIAN_POINT('Origin',(0.,-0.27783,0.));
#49215=CARTESIAN_POINT('',(0.404717578595295,-0.07938,1.65807299932179));
#49216=CARTESIAN_POINT('Origin',(0.,-0.07938,0.));
#49217=CARTESIAN_POINT('',(-0.404717578595296,-0.07938,1.65807299932179));
#49218=CARTESIAN_POINT('Ctrl Pts',(0.404717578595296,-0.0793800000000001,
1.65807299932179));
#49219=CARTESIAN_POINT('Ctrl Pts',(0.400393769631747,-0.101649918886749,
1.65912839404491));
#49220=CARTESIAN_POINT('Ctrl Pts',(0.394174530911058,-0.123823518623745,
1.66063136041479));
#49221=CARTESIAN_POINT('Ctrl Pts',(0.368536561654407,-0.192480977588835,
1.66658649961961));
#49222=CARTESIAN_POINT('Ctrl Pts',(0.341837165343982,-0.236152929235937,
1.67246562047521));
#49223=CARTESIAN_POINT('Ctrl Pts',(0.283214707341173,-0.303141259068211,
1.68332504372461));
#49224=CARTESIAN_POINT('Ctrl Pts',(0.244262842368623,-0.335108247315849,
1.68958170688653));
#49225=CARTESIAN_POINT('Ctrl Pts',(0.178166559972324,-0.373243761060364,
1.69769003172132));
#49226=CARTESIAN_POINT('Ctrl Pts',(0.143648558862931,-0.387888272594439,
1.70107730356824));
#49227=CARTESIAN_POINT('Ctrl Pts',(0.0717778861362652,-0.407041111792943,
1.70562212620408));
#49228=CARTESIAN_POINT('Ctrl Pts',(0.0344244045173309,-0.411552957311693,
1.706752));
#49229=CARTESIAN_POINT('Ctrl Pts',(-0.0344244045173315,-0.411552957311693,
1.706752));
#49230=CARTESIAN_POINT('Ctrl Pts',(-0.0717778861362658,-0.407041111792943,
1.70562212620408));
#49231=CARTESIAN_POINT('Ctrl Pts',(-0.143648558862932,-0.387888272594439,
1.70107730356824));
#49232=CARTESIAN_POINT('Ctrl Pts',(-0.178166559972325,-0.373243761060364,
1.69769003172132));
#49233=CARTESIAN_POINT('Ctrl Pts',(-0.244262842368624,-0.335108247315849,
1.68958170688653));
#49234=CARTESIAN_POINT('Ctrl Pts',(-0.283214707341173,-0.303141259068212,
1.68332504372461));
#49235=CARTESIAN_POINT('Ctrl Pts',(-0.341837165343982,-0.236152929235937,
1.67246562047521));
#49236=CARTESIAN_POINT('Ctrl Pts',(-0.368536561654408,-0.192480977588835,
1.66658649961961));
#49237=CARTESIAN_POINT('Ctrl Pts',(-0.394174530911059,-0.123823518623745,
1.66063136041479));
#49238=CARTESIAN_POINT('Ctrl Pts',(-0.400393769631748,-0.101649918886749,
1.65912839404491));
#49239=CARTESIAN_POINT('Ctrl Pts',(-0.404717578595297,-0.0793800000000001,
1.65807299932179));
#49240=CARTESIAN_POINT('',(-0.886256117232624,-0.07938,1.45861320581289));
#49241=CARTESIAN_POINT('Origin',(0.,-0.07938,0.));
#49242=CARTESIAN_POINT('',(-1.45861320581289,-0.07938,0.886256117232623));
#49243=CARTESIAN_POINT('Ctrl Pts',(-0.886256117232623,-0.0793800000000001,
1.45861320581289));
#49244=CARTESIAN_POINT('Ctrl Pts',(-0.890059788636852,-0.101649918886749,
1.45630208793976));
#49245=CARTESIAN_POINT('Ctrl Pts',(-0.895520212222106,-0.123823518623745,
1.45296717977858));
#49246=CARTESIAN_POINT('Ctrl Pts',(-0.917859913453974,-0.192480977588835,
1.43904931717599));
#49247=CARTESIAN_POINT('Ctrl Pts',(-0.940896403863071,-0.236152929235937,
1.4243271592157));
#49248=CARTESIAN_POINT('Ctrl Pts',(-0.990027513266105,-0.303141259068211,
1.39055359345152));
#49249=CARTESIAN_POINT('Ctrl Pts',(-1.02199477007745,-0.335108247315848,
1.36743459453896));
#49250=CARTESIAN_POINT('Ctrl Pts',(-1.07446535104584,-0.373243761060364,
1.32643091652006));
#49251=CARTESIAN_POINT('Ctrl Pts',(-1.10126842659597,-0.387888272594439,
1.30441816675528));
#49252=CARTESIAN_POINT('Ctrl Pts',(-1.15530234155453,-0.407041111792943,
1.25681160160691));
#49253=CARTESIAN_POINT('Ctrl Pts',(-1.18251418313119,-0.411552957311693,
1.23119764287622));
#49254=CARTESIAN_POINT('Ctrl Pts',(-1.23119764287622,-0.411552957311693,
1.18251418313119));
#49255=CARTESIAN_POINT('Ctrl Pts',(-1.25681160160691,-0.407041111792943,
1.15530234155453));
#49256=CARTESIAN_POINT('Ctrl Pts',(-1.30441816675528,-0.387888272594439,
1.10126842659597));
#49257=CARTESIAN_POINT('Ctrl Pts',(-1.32643091652006,-0.373243761060365,
1.07446535104584));
#49258=CARTESIAN_POINT('Ctrl Pts',(-1.36743459453896,-0.335108247315849,
1.02199477007745));
#49259=CARTESIAN_POINT('Ctrl Pts',(-1.39055359345152,-0.303141259068212,
0.990027513266106));
#49260=CARTESIAN_POINT('Ctrl Pts',(-1.4243271592157,-0.236152929235938,
0.940896403863071));
#49261=CARTESIAN_POINT('Ctrl Pts',(-1.43904931717599,-0.192480977588836,
0.917859913453974));
#49262=CARTESIAN_POINT('Ctrl Pts',(-1.45296717977858,-0.123823518623746,
0.895520212222106));
#49263=CARTESIAN_POINT('Ctrl Pts',(-1.45630208793976,-0.101649918886749,
0.890059788636852));
#49264=CARTESIAN_POINT('Ctrl Pts',(-1.45861320581289,-0.0793800000000001,
0.886256117232623));
#49265=CARTESIAN_POINT('',(-1.65807299932179,-0.07938,0.404717578595295));
#49266=CARTESIAN_POINT('Origin',(0.,-0.07938,0.));
#49267=CARTESIAN_POINT('',(-1.706752,-0.411552957311693,2.08591827245526E-16));
#49268=CARTESIAN_POINT('Ctrl Pts',(-1.65807299932179,-0.0793800000000001,
0.404717578595296));
#49269=CARTESIAN_POINT('Ctrl Pts',(-1.65912839404491,-0.101649918886749,
0.400393769631747));
#49270=CARTESIAN_POINT('Ctrl Pts',(-1.66063136041479,-0.123823518623745,
0.394174530911058));
#49271=CARTESIAN_POINT('Ctrl Pts',(-1.66658649961961,-0.192480977588835,
0.368536561654407));
#49272=CARTESIAN_POINT('Ctrl Pts',(-1.67246562047521,-0.236152929235937,
0.341837165343982));
#49273=CARTESIAN_POINT('Ctrl Pts',(-1.68332504372461,-0.303141259068211,
0.283214707341173));
#49274=CARTESIAN_POINT('Ctrl Pts',(-1.68958170688653,-0.335108247315848,
0.244262842368623));
#49275=CARTESIAN_POINT('Ctrl Pts',(-1.69769003172132,-0.373243761060364,
0.178166559972324));
#49276=CARTESIAN_POINT('Ctrl Pts',(-1.70107730356824,-0.387888272594439,
0.143648558862931));
#49277=CARTESIAN_POINT('Ctrl Pts',(-1.70562212620408,-0.407041111792943,
0.0717778861362656));
#49278=CARTESIAN_POINT('Ctrl Pts',(-1.706752,-0.411552957311693,0.0344244045173313));
#49279=CARTESIAN_POINT('Ctrl Pts',(-1.706752,-0.411552957311693,2.08166817117217E-16));
#49280=CARTESIAN_POINT('',(-1.706752,-0.47628,2.09016837373834E-16));
#49281=CARTESIAN_POINT('',(-1.706752,-0.27783,2.09016837373834E-16));
#49282=CARTESIAN_POINT('Origin',(0.,-0.47628,0.));
#49283=CARTESIAN_POINT('',(-1.65807299932179,-0.07938,-0.404717578595296));
#49284=CARTESIAN_POINT('Ctrl Pts',(-1.706752,-0.411552957311693,2.0122792321331E-16));
#49285=CARTESIAN_POINT('Ctrl Pts',(-1.706752,-0.411552957311693,-0.0344244045173309));
#49286=CARTESIAN_POINT('Ctrl Pts',(-1.70562212620408,-0.407041111792943,
-0.0717778861362652));
#49287=CARTESIAN_POINT('Ctrl Pts',(-1.70107730356824,-0.387888272594439,
-0.143648558862931));
#49288=CARTESIAN_POINT('Ctrl Pts',(-1.69769003172132,-0.373243761060365,
-0.178166559972324));
#49289=CARTESIAN_POINT('Ctrl Pts',(-1.68958170688653,-0.335108247315849,
-0.244262842368623));
#49290=CARTESIAN_POINT('Ctrl Pts',(-1.68332504372461,-0.303141259068212,
-0.283214707341173));
#49291=CARTESIAN_POINT('Ctrl Pts',(-1.67246562047521,-0.236152929235938,
-0.341837165343982));
#49292=CARTESIAN_POINT('Ctrl Pts',(-1.66658649961961,-0.192480977588836,
-0.368536561654407));
#49293=CARTESIAN_POINT('Ctrl Pts',(-1.66063136041479,-0.123823518623745,
-0.394174530911059));
#49294=CARTESIAN_POINT('Ctrl Pts',(-1.65912839404491,-0.101649918886749,
-0.400393769631748));
#49295=CARTESIAN_POINT('Ctrl Pts',(-1.65807299932179,-0.0793800000000001,
-0.404717578595296));
#49296=CARTESIAN_POINT('',(-1.45861320581289,-0.07938,-0.886256117232623));
#49297=CARTESIAN_POINT('Origin',(0.,-0.07938,0.));
#49298=CARTESIAN_POINT('',(-0.886256117232623,-0.07938,-1.45861320581289));
#49299=CARTESIAN_POINT('Ctrl Pts',(-1.45861320581289,-0.0793800000000001,
-0.886256117232623));
#49300=CARTESIAN_POINT('Ctrl Pts',(-1.45630208793976,-0.101649918886749,
-0.890059788636852));
#49301=CARTESIAN_POINT('Ctrl Pts',(-1.45296717977858,-0.123823518623745,
-0.895520212222106));
#49302=CARTESIAN_POINT('Ctrl Pts',(-1.43904931717599,-0.192480977588835,
-0.917859913453974));
#49303=CARTESIAN_POINT('Ctrl Pts',(-1.4243271592157,-0.236152929235937,
-0.940896403863072));
#49304=CARTESIAN_POINT('Ctrl Pts',(-1.39055359345152,-0.303141259068212,
-0.990027513266106));
#49305=CARTESIAN_POINT('Ctrl Pts',(-1.36743459453896,-0.335108247315849,
-1.02199477007745));
#49306=CARTESIAN_POINT('Ctrl Pts',(-1.32643091652006,-0.373243761060364,
-1.07446535104584));
#49307=CARTESIAN_POINT('Ctrl Pts',(-1.30441816675528,-0.387888272594439,
-1.10126842659597));
#49308=CARTESIAN_POINT('Ctrl Pts',(-1.25681160160691,-0.407041111792943,
-1.15530234155453));
#49309=CARTESIAN_POINT('Ctrl Pts',(-1.23119764287622,-0.411552957311693,
-1.18251418313119));
#49310=CARTESIAN_POINT('Ctrl Pts',(-1.18251418313119,-0.411552957311693,
-1.23119764287622));
#49311=CARTESIAN_POINT('Ctrl Pts',(-1.15530234155453,-0.407041111792943,
-1.25681160160691));
#49312=CARTESIAN_POINT('Ctrl Pts',(-1.10126842659597,-0.387888272594439,
-1.30441816675528));
#49313=CARTESIAN_POINT('Ctrl Pts',(-1.07446535104584,-0.373243761060364,
-1.32643091652006));
#49314=CARTESIAN_POINT('Ctrl Pts',(-1.02199477007745,-0.335108247315848,
-1.36743459453896));
#49315=CARTESIAN_POINT('Ctrl Pts',(-0.990027513266105,-0.303141259068211,
-1.39055359345152));
#49316=CARTESIAN_POINT('Ctrl Pts',(-0.940896403863071,-0.236152929235936,
-1.42432715921571));
#49317=CARTESIAN_POINT('Ctrl Pts',(-0.917859913453974,-0.192480977588835,
-1.43904931717599));
#49318=CARTESIAN_POINT('Ctrl Pts',(-0.895520212222106,-0.123823518623745,
-1.45296717977858));
#49319=CARTESIAN_POINT('Ctrl Pts',(-0.890059788636851,-0.101649918886749,
-1.45630208793976));
#49320=CARTESIAN_POINT('Ctrl Pts',(-0.886256117232623,-0.0793800000000001,
-1.45861320581289));
#49321=CARTESIAN_POINT('',(-0.404717578595295,-0.07938,-1.65807299932179));
#49322=CARTESIAN_POINT('Origin',(0.,-0.07938,0.));
#49323=CARTESIAN_POINT('',(0.404717578595296,-0.07938,-1.65807299932179));
#49324=CARTESIAN_POINT('Ctrl Pts',(-0.404717578595296,-0.0793800000000001,
-1.65807299932179));
#49325=CARTESIAN_POINT('Ctrl Pts',(-0.400393769631747,-0.101649918886749,
-1.65912839404491));
#49326=CARTESIAN_POINT('Ctrl Pts',(-0.394174530911058,-0.123823518623746,
-1.66063136041479));
#49327=CARTESIAN_POINT('Ctrl Pts',(-0.368536561654407,-0.192480977588836,
-1.66658649961961));
#49328=CARTESIAN_POINT('Ctrl Pts',(-0.341837165343982,-0.236152929235938,
-1.67246562047521));
#49329=CARTESIAN_POINT('Ctrl Pts',(-0.283214707341173,-0.303141259068212,
-1.68332504372461));
#49330=CARTESIAN_POINT('Ctrl Pts',(-0.244262842368623,-0.335108247315849,
-1.68958170688653));
#49331=CARTESIAN_POINT('Ctrl Pts',(-0.178166559972324,-0.373243761060364,
-1.69769003172132));
#49332=CARTESIAN_POINT('Ctrl Pts',(-0.143648558862931,-0.387888272594439,
-1.70107730356824));
#49333=CARTESIAN_POINT('Ctrl Pts',(-0.0717778861362653,-0.407041111792943,
-1.70562212620408));
#49334=CARTESIAN_POINT('Ctrl Pts',(-0.034424404517331,-0.411552957311693,
-1.706752));
#49335=CARTESIAN_POINT('Ctrl Pts',(0.0344244045173312,-0.411552957311693,
-1.706752));
#49336=CARTESIAN_POINT('Ctrl Pts',(0.0717778861362655,-0.407041111792943,
-1.70562212620408));
#49337=CARTESIAN_POINT('Ctrl Pts',(0.143648558862931,-0.387888272594439,
-1.70107730356824));
#49338=CARTESIAN_POINT('Ctrl Pts',(0.178166559972324,-0.373243761060364,
-1.69769003172132));
#49339=CARTESIAN_POINT('Ctrl Pts',(0.244262842368623,-0.335108247315849,
-1.68958170688653));
#49340=CARTESIAN_POINT('Ctrl Pts',(0.283214707341173,-0.303141259068212,
-1.68332504372461));
#49341=CARTESIAN_POINT('Ctrl Pts',(0.341837165343982,-0.236152929235937,
-1.67246562047521));
#49342=CARTESIAN_POINT('Ctrl Pts',(0.368536561654407,-0.192480977588835,
-1.66658649961961));
#49343=CARTESIAN_POINT('Ctrl Pts',(0.394174530911059,-0.123823518623745,
-1.66063136041479));
#49344=CARTESIAN_POINT('Ctrl Pts',(0.400393769631748,-0.101649918886749,
-1.65912839404491));
#49345=CARTESIAN_POINT('Ctrl Pts',(0.404717578595296,-0.0793800000000001,
-1.65807299932179));
#49346=CARTESIAN_POINT('',(0.886256117232623,-0.07938,-1.45861320581289));
#49347=CARTESIAN_POINT('Origin',(0.,-0.07938,0.));
#49348=CARTESIAN_POINT('',(1.45861320581289,-0.07938,-0.886256117232623));
#49349=CARTESIAN_POINT('Ctrl Pts',(0.886256117232623,-0.0793800000000001,
-1.45861320581289));
#49350=CARTESIAN_POINT('Ctrl Pts',(0.890059788636852,-0.101649918886749,
-1.45630208793976));
#49351=CARTESIAN_POINT('Ctrl Pts',(0.895520212222106,-0.123823518623745,
-1.45296717977858));
#49352=CARTESIAN_POINT('Ctrl Pts',(0.917859913453974,-0.192480977588835,
-1.43904931717599));
#49353=CARTESIAN_POINT('Ctrl Pts',(0.940896403863072,-0.236152929235937,
-1.4243271592157));
#49354=CARTESIAN_POINT('Ctrl Pts',(0.990027513266106,-0.303141259068211,
-1.39055359345152));
#49355=CARTESIAN_POINT('Ctrl Pts',(1.02199477007745,-0.335108247315849,
-1.36743459453896));
#49356=CARTESIAN_POINT('Ctrl Pts',(1.07446535104584,-0.373243761060364,
-1.32643091652006));
#49357=CARTESIAN_POINT('Ctrl Pts',(1.10126842659597,-0.387888272594439,
-1.30441816675528));
#49358=CARTESIAN_POINT('Ctrl Pts',(1.15530234155453,-0.407041111792943,
-1.25681160160691));
#49359=CARTESIAN_POINT('Ctrl Pts',(1.18251418313119,-0.411552957311693,
-1.23119764287622));
#49360=CARTESIAN_POINT('Ctrl Pts',(1.23119764287622,-0.411552957311693,
-1.18251418313119));
#49361=CARTESIAN_POINT('Ctrl Pts',(1.25681160160691,-0.407041111792943,
-1.15530234155453));
#49362=CARTESIAN_POINT('Ctrl Pts',(1.30441816675528,-0.387888272594439,
-1.10126842659597));
#49363=CARTESIAN_POINT('Ctrl Pts',(1.32643091652006,-0.373243761060364,
-1.07446535104584));
#49364=CARTESIAN_POINT('Ctrl Pts',(1.36743459453896,-0.335108247315849,
-1.02199477007745));
#49365=CARTESIAN_POINT('Ctrl Pts',(1.39055359345152,-0.303141259068212,
-0.990027513266105));
#49366=CARTESIAN_POINT('Ctrl Pts',(1.4243271592157,-0.236152929235937,-0.940896403863071));
#49367=CARTESIAN_POINT('Ctrl Pts',(1.43904931717599,-0.192480977588835,
-0.917859913453974));
#49368=CARTESIAN_POINT('Ctrl Pts',(1.45296717977858,-0.123823518623745,
-0.895520212222106));
#49369=CARTESIAN_POINT('Ctrl Pts',(1.45630208793976,-0.101649918886749,
-0.890059788636852));
#49370=CARTESIAN_POINT('Ctrl Pts',(1.45861320581289,-0.0793800000000001,
-0.886256117232623));
#49371=CARTESIAN_POINT('',(1.65807299932179,-0.07938,-0.404717578595296));
#49372=CARTESIAN_POINT('Origin',(0.,-0.07938,0.));
#49373=CARTESIAN_POINT('',(1.65807299932179,-0.07938,0.404717578595296));
#49374=CARTESIAN_POINT('Ctrl Pts',(1.65807299932179,-0.0793800000000001,
-0.404717578595296));
#49375=CARTESIAN_POINT('Ctrl Pts',(1.65912839404491,-0.101649918886749,
-0.400393769631747));
#49376=CARTESIAN_POINT('Ctrl Pts',(1.66063136041479,-0.123823518623745,
-0.394174530911058));
#49377=CARTESIAN_POINT('Ctrl Pts',(1.66658649961961,-0.192480977588835,
-0.368536561654407));
#49378=CARTESIAN_POINT('Ctrl Pts',(1.67246562047521,-0.236152929235937,
-0.341837165343982));
#49379=CARTESIAN_POINT('Ctrl Pts',(1.68332504372461,-0.303141259068212,
-0.283214707341173));
#49380=CARTESIAN_POINT('Ctrl Pts',(1.68958170688653,-0.335108247315849,
-0.244262842368623));
#49381=CARTESIAN_POINT('Ctrl Pts',(1.69769003172132,-0.373243761060364,
-0.178166559972324));
#49382=CARTESIAN_POINT('Ctrl Pts',(1.70107730356824,-0.387888272594439,
-0.143648558862931));
#49383=CARTESIAN_POINT('Ctrl Pts',(1.70562212620408,-0.407041111792943,
-0.0717778861362655));
#49384=CARTESIAN_POINT('Ctrl Pts',(1.706752,-0.411552957311693,-0.0344244045173312));
#49385=CARTESIAN_POINT('Ctrl Pts',(1.706752,-0.411552957311693,0.0344244045173312));
#49386=CARTESIAN_POINT('Ctrl Pts',(1.70562212620408,-0.407041111792943,
0.0717778861362655));
#49387=CARTESIAN_POINT('Ctrl Pts',(1.70107730356824,-0.387888272594439,
0.143648558862931));
#49388=CARTESIAN_POINT('Ctrl Pts',(1.69769003172132,-0.373243761060364,
0.178166559972324));
#49389=CARTESIAN_POINT('Ctrl Pts',(1.68958170688653,-0.335108247315849,
0.244262842368623));
#49390=CARTESIAN_POINT('Ctrl Pts',(1.68332504372461,-0.303141259068212,
0.283214707341173));
#49391=CARTESIAN_POINT('Ctrl Pts',(1.67246562047521,-0.236152929235937,
0.341837165343982));
#49392=CARTESIAN_POINT('Ctrl Pts',(1.66658649961961,-0.192480977588835,
0.368536561654407));
#49393=CARTESIAN_POINT('Ctrl Pts',(1.66063136041479,-0.123823518623745,
0.394174530911058));
#49394=CARTESIAN_POINT('Ctrl Pts',(1.65912839404491,-0.101649918886749,
0.400393769631747));
#49395=CARTESIAN_POINT('Ctrl Pts',(1.65807299932179,-0.0793800000000001,
0.404717578595296));
#49396=CARTESIAN_POINT('Origin',(0.,-0.07938,0.));
#49397=CARTESIAN_POINT('Origin',(0.,-0.07938,0.));
#49398=CARTESIAN_POINT('',(0.397005914195118,-0.07938,1.59456899932179));
#49399=CARTESIAN_POINT('Origin',(0.,-0.07938,0.));
#49400=CARTESIAN_POINT('Origin',(-3.33066907387547E-16,-0.07938,1.675));
#49401=CARTESIAN_POINT('Origin',(-3.33066907387547E-16,0.,1.675));
#49402=CARTESIAN_POINT('',(-0.397005914195118,-0.07938,1.59456899932179));
#49403=CARTESIAN_POINT('Ctrl Pts',(-0.397005914195119,-0.0793800000000001,
1.59456899932179));
#49404=CARTESIAN_POINT('Ctrl Pts',(-0.3886265584581,-0.123401821157026,
1.59665523941937));
#49405=CARTESIAN_POINT('Ctrl Pts',(-0.373030350867485,-0.166543350814306,
1.60050712143809));
#49406=CARTESIAN_POINT('Ctrl Pts',(-0.333298652394954,-0.237231147975234,
1.60919314384089));
#49407=CARTESIAN_POINT('Ctrl Pts',(-0.311480544243687,-0.266264900654909,
1.61365775139403));
#49408=CARTESIAN_POINT('Ctrl Pts',(-0.261368388670537,-0.317195968905306,
1.62252828437015));
#49409=CARTESIAN_POINT('Ctrl Pts',(-0.233069203882014,-0.33909093068465,
1.62691869420078));
#49410=CARTESIAN_POINT('Ctrl Pts',(-0.174042761838764,-0.373586846396559,
1.63426473152765));
#49411=CARTESIAN_POINT('Ctrl Pts',(-0.14036578147155,-0.388086240756494,
1.63761964365402));
#49412=CARTESIAN_POINT('Ctrl Pts',(-0.0701778381840615,-0.407068917407805,
1.64212536811722));
#49413=CARTESIAN_POINT('Ctrl Pts',(-0.0336652739555918,-0.411552957311693,
1.643248));
#49414=CARTESIAN_POINT('Ctrl Pts',(0.0336652739555913,-0.411552957311693,
1.643248));
#49415=CARTESIAN_POINT('Ctrl Pts',(0.070177838184061,-0.407068917407805,
1.64212536811722));
#49416=CARTESIAN_POINT('Ctrl Pts',(0.140365781471549,-0.388086240756494,
1.63761964365402));
#49417=CARTESIAN_POINT('Ctrl Pts',(0.174042761838763,-0.373586846396559,
1.63426473152765));
#49418=CARTESIAN_POINT('Ctrl Pts',(0.233069203882014,-0.33909093068465,
1.62691869420078));
#49419=CARTESIAN_POINT('Ctrl Pts',(0.261368388670536,-0.317195968905306,
1.62252828437015));
#49420=CARTESIAN_POINT('Ctrl Pts',(0.311480544243686,-0.266264900654908,
1.61365775139403));
#49421=CARTESIAN_POINT('Ctrl Pts',(0.333298652394954,-0.237231147975234,
1.60919314384089));
#49422=CARTESIAN_POINT('Ctrl Pts',(0.373030350867484,-0.166543350814306,
1.60050712143809));
#49423=CARTESIAN_POINT('Ctrl Pts',(0.388626558458099,-0.123401821157026,
1.59665523941937));
#49424=CARTESIAN_POINT('Ctrl Pts',(0.397005914195118,-0.07938,1.59456899932179));
#49425=CARTESIAN_POINT('Origin',(-3.33066907387547E-16,-0.07938,1.675));
#49426=CARTESIAN_POINT('Origin',(0.,-0.07938,0.));
#49427=CARTESIAN_POINT('',(-0.846804978391754,-0.07938,1.40825612658882));
#49428=CARTESIAN_POINT('Origin',(0.,-0.07938,0.));
#49429=CARTESIAN_POINT('Origin',(-1.18440385848747,-0.07938,1.18440385848747));
#49430=CARTESIAN_POINT('Origin',(-1.18440385848747,0.,1.18440385848747));
#49431=CARTESIAN_POINT('',(-1.40825612658882,-0.07938,0.846804978391753));
#49432=CARTESIAN_POINT('Ctrl Pts',(-1.40825612658882,-0.0793800000000001,
0.846804978391753));
#49433=CARTESIAN_POINT('Ctrl Pts',(-1.40380622184538,-0.123401821157026,
0.854205272175555));
#49434=CARTESIAN_POINT('Ctrl Pts',(-1.39550172959303,-0.166543350814306,
0.867957148219442));
#49435=CARTESIAN_POINT('Ctrl Pts',(-1.3735491215176,-0.237231147975235,
0.902193646979983));
#49436=CARTESIAN_POINT('Ctrl Pts',(-1.36127834356734,-0.266264900654909,
0.920778333482565));
#49437=CARTESIAN_POINT('Ctrl Pts',(-1.33211611256184,-0.317195968905306,
0.962485392528369));
#49438=CARTESIAN_POINT('Ctrl Pts',(-1.31521005565926,-0.339090930684651,
0.985600426557816));
#49439=CARTESIAN_POINT('Ctrl Pts',(-1.27866649102984,-0.373586846396559,
1.03253285680459));
#49440=CARTESIAN_POINT('Ctrl Pts',(-1.25722555095714,-0.388086240756494,
1.05871835910697));
#49441=CARTESIAN_POINT('Ctrl Pts',(-1.2107812086231,-0.407068917407805,
1.11153475808518));
#49442=CARTESIAN_POINT('Ctrl Pts',(-1.18575674747573,-0.411552957311693,
1.13814686046673));
#49443=CARTESIAN_POINT('Ctrl Pts',(-1.13814686046673,-0.411552957311693,
1.18575674747573));
#49444=CARTESIAN_POINT('Ctrl Pts',(-1.11153475808518,-0.407068917407805,
1.2107812086231));
#49445=CARTESIAN_POINT('Ctrl Pts',(-1.05871835910697,-0.388086240756494,
1.25722555095714));
#49446=CARTESIAN_POINT('Ctrl Pts',(-1.03253285680459,-0.373586846396559,
1.27866649102984));
#49447=CARTESIAN_POINT('Ctrl Pts',(-0.985600426557816,-0.33909093068465,
1.31521005565926));
#49448=CARTESIAN_POINT('Ctrl Pts',(-0.962485392528369,-0.317195968905306,
1.33211611256184));
#49449=CARTESIAN_POINT('Ctrl Pts',(-0.920778333482565,-0.266264900654908,
1.36127834356734));
#49450=CARTESIAN_POINT('Ctrl Pts',(-0.902193646979983,-0.237231147975234,
1.3735491215176));
#49451=CARTESIAN_POINT('Ctrl Pts',(-0.867957148219442,-0.166543350814306,
1.39550172959303));
#49452=CARTESIAN_POINT('Ctrl Pts',(-0.854205272175555,-0.123401821157026,
1.40380622184538));
#49453=CARTESIAN_POINT('Ctrl Pts',(-0.846804978391753,-0.0793800000000001,
1.40825612658882));
#49454=CARTESIAN_POINT('Origin',(-1.18440385848747,-0.07938,1.18440385848747));
#49455=CARTESIAN_POINT('Origin',(0.,-0.07938,0.));
#49456=CARTESIAN_POINT('',(-1.59456899932179,-0.07938,0.397005914195118));
#49457=CARTESIAN_POINT('Origin',(0.,-0.07938,0.));
#49458=CARTESIAN_POINT('Origin',(-1.675,-0.07938,-2.22044604925031E-16));
#49459=CARTESIAN_POINT('Origin',(-1.675,0.,-2.22044604925031E-16));
#49460=CARTESIAN_POINT('',(-1.59456899932179,-0.07938,-0.397005914195118));
#49461=CARTESIAN_POINT('',(-1.643248,-0.411552957311693,3.47540551556327E-18));
#49462=CARTESIAN_POINT('Ctrl Pts',(-1.59456899932179,-0.0793800000000001,
-0.397005914195119));
#49463=CARTESIAN_POINT('Ctrl Pts',(-1.59665523941937,-0.123401821157026,
-0.388626558458099));
#49464=CARTESIAN_POINT('Ctrl Pts',(-1.60050712143809,-0.166543350814306,
-0.373030350867485));
#49465=CARTESIAN_POINT('Ctrl Pts',(-1.60919314384089,-0.237231147975234,
-0.333298652394954));
#49466=CARTESIAN_POINT('Ctrl Pts',(-1.61365775139403,-0.266264900654909,
-0.311480544243686));
#49467=CARTESIAN_POINT('Ctrl Pts',(-1.62252828437015,-0.317195968905306,
-0.261368388670537));
#49468=CARTESIAN_POINT('Ctrl Pts',(-1.62691869420078,-0.33909093068465,
-0.233069203882014));
#49469=CARTESIAN_POINT('Ctrl Pts',(-1.63426473152765,-0.373586846396559,
-0.174042761838764));
#49470=CARTESIAN_POINT('Ctrl Pts',(-1.63761964365402,-0.388086240756494,
-0.140365781471549));
#49471=CARTESIAN_POINT('Ctrl Pts',(-1.64212536811722,-0.407068917407805,
-0.0701778381840614));
#49472=CARTESIAN_POINT('Ctrl Pts',(-1.643248,-0.411552957311693,-0.0336652739555917));
#49473=CARTESIAN_POINT('Ctrl Pts',(-1.643248,-0.411552957311693,-2.0122792321331E-16));
#49474=CARTESIAN_POINT('Origin',(-1.675,-0.07938,-2.22044604925031E-16));
#49475=CARTESIAN_POINT('Ctrl Pts',(-1.643248,-0.411552957311693,-1.94289029309402E-16));
#49476=CARTESIAN_POINT('Ctrl Pts',(-1.643248,-0.411552957311693,0.0336652739555913));
#49477=CARTESIAN_POINT('Ctrl Pts',(-1.64212536811722,-0.407068917407805,
0.0701778381840609));
#49478=CARTESIAN_POINT('Ctrl Pts',(-1.63761964365402,-0.388086240756494,
0.140365781471549));
#49479=CARTESIAN_POINT('Ctrl Pts',(-1.63426473152765,-0.373586846396559,
0.174042761838763));
#49480=CARTESIAN_POINT('Ctrl Pts',(-1.62691869420078,-0.33909093068465,
0.233069203882014));
#49481=CARTESIAN_POINT('Ctrl Pts',(-1.62252828437015,-0.317195968905306,
0.261368388670536));
#49482=CARTESIAN_POINT('Ctrl Pts',(-1.61365775139403,-0.266264900654909,
0.311480544243686));
#49483=CARTESIAN_POINT('Ctrl Pts',(-1.60919314384089,-0.237231147975235,
0.333298652394954));
#49484=CARTESIAN_POINT('Ctrl Pts',(-1.60050712143809,-0.166543350814306,
0.373030350867484));
#49485=CARTESIAN_POINT('Ctrl Pts',(-1.59665523941937,-0.123401821157026,
0.388626558458099));
#49486=CARTESIAN_POINT('Ctrl Pts',(-1.59456899932179,-0.0793800000000001,
0.397005914195118));
#49487=CARTESIAN_POINT('Origin',(0.,-0.07938,0.));
#49488=CARTESIAN_POINT('',(-1.40825612658882,-0.07938,-0.846804978391753));
#49489=CARTESIAN_POINT('Origin',(0.,-0.07938,0.));
#49490=CARTESIAN_POINT('Origin',(-1.18440385848747,-0.07938,-1.18440385848747));
#49491=CARTESIAN_POINT('Origin',(-1.18440385848747,0.,-1.18440385848747));
#49492=CARTESIAN_POINT('',(-0.846804978391753,-0.07938,-1.40825612658882));
#49493=CARTESIAN_POINT('Ctrl Pts',(-0.846804978391753,-0.0793800000000001,
-1.40825612658882));
#49494=CARTESIAN_POINT('Ctrl Pts',(-0.854205272175555,-0.123401821157026,
-1.40380622184538));
#49495=CARTESIAN_POINT('Ctrl Pts',(-0.867957148219442,-0.166543350814306,
-1.39550172959303));
#49496=CARTESIAN_POINT('Ctrl Pts',(-0.902193646979982,-0.237231147975234,
-1.3735491215176));
#49497=CARTESIAN_POINT('Ctrl Pts',(-0.920778333482564,-0.266264900654908,
-1.36127834356734));
#49498=CARTESIAN_POINT('Ctrl Pts',(-0.962485392528368,-0.317195968905306,
-1.33211611256184));
#49499=CARTESIAN_POINT('Ctrl Pts',(-0.985600426557816,-0.33909093068465,
-1.31521005565926));
#49500=CARTESIAN_POINT('Ctrl Pts',(-1.03253285680459,-0.373586846396559,
-1.27866649102984));
#49501=CARTESIAN_POINT('Ctrl Pts',(-1.05871835910697,-0.388086240756494,
-1.25722555095714));
#49502=CARTESIAN_POINT('Ctrl Pts',(-1.11153475808518,-0.407068917407805,
-1.2107812086231));
#49503=CARTESIAN_POINT('Ctrl Pts',(-1.13814686046673,-0.411552957311693,
-1.18575674747573));
#49504=CARTESIAN_POINT('Ctrl Pts',(-1.18575674747573,-0.411552957311693,
-1.13814686046673));
#49505=CARTESIAN_POINT('Ctrl Pts',(-1.2107812086231,-0.407068917407805,
-1.11153475808518));
#49506=CARTESIAN_POINT('Ctrl Pts',(-1.25722555095714,-0.388086240756494,
-1.05871835910697));
#49507=CARTESIAN_POINT('Ctrl Pts',(-1.27866649102984,-0.373586846396559,
-1.03253285680459));
#49508=CARTESIAN_POINT('Ctrl Pts',(-1.31521005565926,-0.33909093068465,
-0.985600426557816));
#49509=CARTESIAN_POINT('Ctrl Pts',(-1.33211611256184,-0.317195968905306,
-0.962485392528369));
#49510=CARTESIAN_POINT('Ctrl Pts',(-1.36127834356734,-0.266264900654909,
-0.920778333482565));
#49511=CARTESIAN_POINT('Ctrl Pts',(-1.3735491215176,-0.237231147975234,
-0.902193646979983));
#49512=CARTESIAN_POINT('Ctrl Pts',(-1.39550172959303,-0.166543350814306,
-0.867957148219442));
#49513=CARTESIAN_POINT('Ctrl Pts',(-1.40380622184538,-0.123401821157026,
-0.854205272175555));
#49514=CARTESIAN_POINT('Ctrl Pts',(-1.40825612658882,-0.07938,-0.846804978391753));
#49515=CARTESIAN_POINT('Origin',(-1.18440385848747,-0.07938,-1.18440385848747));
#49516=CARTESIAN_POINT('Origin',(0.,-0.07938,0.));
#49517=CARTESIAN_POINT('',(-0.397005914195118,-0.07938,-1.59456899932179));
#49518=CARTESIAN_POINT('Origin',(0.,-0.07938,0.));
#49519=CARTESIAN_POINT('Origin',(1.11022302462516E-16,-0.07938,-1.675));
#49520=CARTESIAN_POINT('Origin',(1.11022302462516E-16,0.,-1.675));
#49521=CARTESIAN_POINT('',(0.397005914195118,-0.07938,-1.59456899932179));
#49522=CARTESIAN_POINT('Ctrl Pts',(0.397005914195119,-0.0793800000000001,
-1.59456899932179));
#49523=CARTESIAN_POINT('Ctrl Pts',(0.388626558458099,-0.123401821157026,
-1.59665523941937));
#49524=CARTESIAN_POINT('Ctrl Pts',(0.373030350867485,-0.166543350814306,
-1.60050712143809));
#49525=CARTESIAN_POINT('Ctrl Pts',(0.333298652394954,-0.237231147975234,
-1.60919314384089));
#49526=CARTESIAN_POINT('Ctrl Pts',(0.311480544243686,-0.266264900654909,
-1.61365775139403));
#49527=CARTESIAN_POINT('Ctrl Pts',(0.261368388670537,-0.317195968905306,
-1.62252828437015));
#49528=CARTESIAN_POINT('Ctrl Pts',(0.233069203882014,-0.33909093068465,
-1.62691869420078));
#49529=CARTESIAN_POINT('Ctrl Pts',(0.174042761838763,-0.373586846396559,
-1.63426473152765));
#49530=CARTESIAN_POINT('Ctrl Pts',(0.140365781471549,-0.388086240756494,
-1.63761964365402));
#49531=CARTESIAN_POINT('Ctrl Pts',(0.0701778381840612,-0.407068917407805,
-1.64212536811722));
#49532=CARTESIAN_POINT('Ctrl Pts',(0.0336652739555916,-0.411552957311693,
-1.643248));
#49533=CARTESIAN_POINT('Ctrl Pts',(-0.0336652739555915,-0.411552957311693,
-1.643248));
#49534=CARTESIAN_POINT('Ctrl Pts',(-0.0701778381840612,-0.407068917407805,
-1.64212536811722));
#49535=CARTESIAN_POINT('Ctrl Pts',(-0.140365781471549,-0.388086240756494,
-1.63761964365402));
#49536=CARTESIAN_POINT('Ctrl Pts',(-0.174042761838764,-0.373586846396559,
-1.63426473152765));
#49537=CARTESIAN_POINT('Ctrl Pts',(-0.233069203882014,-0.33909093068465,
-1.62691869420078));
#49538=CARTESIAN_POINT('Ctrl Pts',(-0.261368388670536,-0.317195968905306,
-1.62252828437015));
#49539=CARTESIAN_POINT('Ctrl Pts',(-0.311480544243686,-0.266264900654908,
-1.61365775139403));
#49540=CARTESIAN_POINT('Ctrl Pts',(-0.333298652394954,-0.237231147975234,
-1.60919314384089));
#49541=CARTESIAN_POINT('Ctrl Pts',(-0.373030350867485,-0.166543350814306,
-1.60050712143809));
#49542=CARTESIAN_POINT('Ctrl Pts',(-0.388626558458099,-0.123401821157026,
-1.59665523941937));
#49543=CARTESIAN_POINT('Ctrl Pts',(-0.397005914195118,-0.07938,-1.59456899932179));
#49544=CARTESIAN_POINT('Origin',(1.11022302462516E-16,-0.07938,-1.675));
#49545=CARTESIAN_POINT('Origin',(0.,-0.07938,0.));
#49546=CARTESIAN_POINT('',(0.846804978391753,-0.07938,-1.40825612658882));
#49547=CARTESIAN_POINT('Origin',(0.,-0.07938,0.));
#49548=CARTESIAN_POINT('Origin',(1.18440385848747,-0.07938,-1.18440385848747));
#49549=CARTESIAN_POINT('Origin',(1.18440385848747,0.,-1.18440385848747));
#49550=CARTESIAN_POINT('',(1.40825612658882,-0.07938,-0.846804978391753));
#49551=CARTESIAN_POINT('Ctrl Pts',(1.40825612658882,-0.0793800000000001,
-0.846804978391753));
#49552=CARTESIAN_POINT('Ctrl Pts',(1.40380622184538,-0.123401821157026,
-0.854205272175555));
#49553=CARTESIAN_POINT('Ctrl Pts',(1.39550172959303,-0.166543350814306,
-0.867957148219442));
#49554=CARTESIAN_POINT('Ctrl Pts',(1.3735491215176,-0.237231147975234,-0.902193646979983));
#49555=CARTESIAN_POINT('Ctrl Pts',(1.36127834356734,-0.266264900654908,
-0.920778333482565));
#49556=CARTESIAN_POINT('Ctrl Pts',(1.33211611256184,-0.317195968905306,
-0.962485392528369));
#49557=CARTESIAN_POINT('Ctrl Pts',(1.31521005565926,-0.33909093068465,-0.985600426557816));
#49558=CARTESIAN_POINT('Ctrl Pts',(1.27866649102984,-0.373586846396559,
-1.03253285680459));
#49559=CARTESIAN_POINT('Ctrl Pts',(1.25722555095714,-0.388086240756494,
-1.05871835910697));
#49560=CARTESIAN_POINT('Ctrl Pts',(1.2107812086231,-0.407068917407805,-1.11153475808518));
#49561=CARTESIAN_POINT('Ctrl Pts',(1.18575674747573,-0.411552957311693,
-1.13814686046673));
#49562=CARTESIAN_POINT('Ctrl Pts',(1.13814686046673,-0.411552957311693,
-1.18575674747573));
#49563=CARTESIAN_POINT('Ctrl Pts',(1.11153475808518,-0.407068917407805,
-1.2107812086231));
#49564=CARTESIAN_POINT('Ctrl Pts',(1.05871835910697,-0.388086240756494,
-1.25722555095714));
#49565=CARTESIAN_POINT('Ctrl Pts',(1.03253285680459,-0.373586846396559,
-1.27866649102984));
#49566=CARTESIAN_POINT('Ctrl Pts',(0.985600426557816,-0.33909093068465,
-1.31521005565926));
#49567=CARTESIAN_POINT('Ctrl Pts',(0.962485392528369,-0.317195968905306,
-1.33211611256184));
#49568=CARTESIAN_POINT('Ctrl Pts',(0.920778333482565,-0.266264900654909,
-1.36127834356734));
#49569=CARTESIAN_POINT('Ctrl Pts',(0.902193646979983,-0.237231147975234,
-1.3735491215176));
#49570=CARTESIAN_POINT('Ctrl Pts',(0.867957148219442,-0.166543350814306,
-1.39550172959303));
#49571=CARTESIAN_POINT('Ctrl Pts',(0.854205272175555,-0.123401821157026,
-1.40380622184538));
#49572=CARTESIAN_POINT('Ctrl Pts',(0.846804978391753,-0.0793800000000001,
-1.40825612658882));
#49573=CARTESIAN_POINT('Origin',(1.18440385848747,-0.07938,-1.18440385848747));
#49574=CARTESIAN_POINT('Origin',(0.,-0.27783,0.));
#49575=CARTESIAN_POINT('',(-1.643248,-0.47628,2.01239840340529E-16));
#49576=CARTESIAN_POINT('Origin',(0.,-0.47628,0.));
#49577=CARTESIAN_POINT('',(-1.643248,-0.27783,2.01239840340529E-16));
#49578=CARTESIAN_POINT('',(1.59456899932179,-0.07938,0.397005914195118));
#49579=CARTESIAN_POINT('Origin',(0.,-0.07938,0.));
#49580=CARTESIAN_POINT('',(1.59456899932179,-0.07938,-0.397005914195118));
#49581=CARTESIAN_POINT('Ctrl Pts',(1.59456899932179,-0.0793800000000001,
0.397005914195118));
#49582=CARTESIAN_POINT('Ctrl Pts',(1.59665523941937,-0.123401821157026,
0.388626558458099));
#49583=CARTESIAN_POINT('Ctrl Pts',(1.60050712143809,-0.166543350814306,
0.373030350867485));
#49584=CARTESIAN_POINT('Ctrl Pts',(1.60919314384089,-0.237231147975234,
0.333298652394954));
#49585=CARTESIAN_POINT('Ctrl Pts',(1.61365775139403,-0.266264900654909,
0.311480544243686));
#49586=CARTESIAN_POINT('Ctrl Pts',(1.62252828437015,-0.317195968905306,
0.261368388670537));
#49587=CARTESIAN_POINT('Ctrl Pts',(1.62691869420078,-0.33909093068465,0.233069203882014));
#49588=CARTESIAN_POINT('Ctrl Pts',(1.63426473152765,-0.373586846396559,
0.174042761838764));
#49589=CARTESIAN_POINT('Ctrl Pts',(1.63761964365402,-0.388086240756494,
0.140365781471549));
#49590=CARTESIAN_POINT('Ctrl Pts',(1.64212536811722,-0.407068917407805,
0.0701778381840612));
#49591=CARTESIAN_POINT('Ctrl Pts',(1.643248,-0.411552957311693,0.0336652739555916));
#49592=CARTESIAN_POINT('Ctrl Pts',(1.643248,-0.411552957311693,-0.0336652739555916));
#49593=CARTESIAN_POINT('Ctrl Pts',(1.64212536811722,-0.407068917407805,
-0.0701778381840612));
#49594=CARTESIAN_POINT('Ctrl Pts',(1.63761964365402,-0.388086240756494,
-0.140365781471549));
#49595=CARTESIAN_POINT('Ctrl Pts',(1.63426473152765,-0.373586846396559,
-0.174042761838764));
#49596=CARTESIAN_POINT('Ctrl Pts',(1.62691869420078,-0.33909093068465,-0.233069203882014));
#49597=CARTESIAN_POINT('Ctrl Pts',(1.62252828437015,-0.317195968905306,
-0.261368388670537));
#49598=CARTESIAN_POINT('Ctrl Pts',(1.61365775139403,-0.266264900654909,
-0.311480544243686));
#49599=CARTESIAN_POINT('Ctrl Pts',(1.60919314384089,-0.237231147975234,
-0.333298652394954));
#49600=CARTESIAN_POINT('Ctrl Pts',(1.60050712143809,-0.166543350814306,
-0.373030350867485));
#49601=CARTESIAN_POINT('Ctrl Pts',(1.59665523941937,-0.123401821157026,
-0.388626558458099));
#49602=CARTESIAN_POINT('Ctrl Pts',(1.59456899932179,-0.07938,-0.397005914195118));
#49603=CARTESIAN_POINT('Origin',(0.,-0.07938,0.));
#49604=CARTESIAN_POINT('Origin',(0.,-0.07938,0.));
#49605=CARTESIAN_POINT('Origin',(1.675,-0.07938,0.));
#49606=CARTESIAN_POINT('Origin',(1.675,0.,0.));
#49607=CARTESIAN_POINT('Origin',(1.675,-0.07938,0.));
#49608=CARTESIAN_POINT('Origin',(0.,-0.47628,0.));
#49609=CARTESIAN_POINT('Origin',(0.,-0.07938,0.));
#49610=CARTESIAN_POINT('',(0.,0.,0.));
#49611=CARTESIAN_POINT('Origin',(1.70469,0.695,0.));
#49612=CARTESIAN_POINT('',(-1.70469,0.695,-2.0876431520385E-16));
#49613=CARTESIAN_POINT('Origin',(0.,0.695,0.));
#49614=CARTESIAN_POINT('',(-1.65031,0.695,-2.02104685910087E-16));
#49615=CARTESIAN_POINT('Origin',(0.,0.695,0.));
#49616=CARTESIAN_POINT('Origin',(0.,0.6575,0.));
#49617=CARTESIAN_POINT('',(-1.70469,0.62,-2.0876431520385E-16));
#49618=CARTESIAN_POINT('Origin',(0.,0.62,0.));
#49619=CARTESIAN_POINT('',(-1.70469,0.6575,-2.0876431520385E-16));
#49620=CARTESIAN_POINT('Origin',(1.65031,0.62,0.));
#49621=CARTESIAN_POINT('',(-1.65031,0.62,-2.02104685910087E-16));
#49622=CARTESIAN_POINT('Origin',(0.,0.62,0.));
#49623=CARTESIAN_POINT('Origin',(0.,0.6575,0.));
#49624=CARTESIAN_POINT('',(-1.65031,0.6575,-2.02104685910087E-16));
#49625=CARTESIAN_POINT('Origin',(1.70469,-0.62,0.));
#49626=CARTESIAN_POINT('',(-1.70469,-0.62,-2.0876431520385E-16));
#49627=CARTESIAN_POINT('Origin',(0.,-0.62,0.));
#49628=CARTESIAN_POINT('',(-1.65031,-0.62,-2.02104685910087E-16));
#49629=CARTESIAN_POINT('Origin',(0.,-0.62,0.));
#49630=CARTESIAN_POINT('Origin',(0.,-0.6575,0.));
#49631=CARTESIAN_POINT('',(-1.70469,-0.695,-2.0876431520385E-16));
#49632=CARTESIAN_POINT('Origin',(0.,-0.695,0.));
#49633=CARTESIAN_POINT('',(-1.70469,-0.6575,-2.0876431520385E-16));
#49634=CARTESIAN_POINT('Origin',(1.65031,-0.695,0.));
#49635=CARTESIAN_POINT('',(-1.65031,-0.695,-2.02104685910087E-16));
#49636=CARTESIAN_POINT('Origin',(0.,-0.695,0.));
#49637=CARTESIAN_POINT('Origin',(0.,-0.6575,0.));
#49638=CARTESIAN_POINT('',(-1.65031,-0.6575,-2.02104685910087E-16));
#49639=CARTESIAN_POINT('',(0.,0.,0.));
#49640=CARTESIAN_POINT('',(0.,0.,0.));
#49641=CARTESIAN_POINT('',(0.,0.,0.));
#49642=CARTESIAN_POINT('',(0.,0.,0.));
#49643=CARTESIAN_POINT('',(0.,0.,0.));
#49644=CARTESIAN_POINT('',(0.,0.,0.));
#49645=CARTESIAN_POINT('Origin',(0.115470053837925,-0.5,-0.2));
#49646=CARTESIAN_POINT('',(0.23094010767585,-0.5,0.));
#49647=CARTESIAN_POINT('',(0.115470053837925,-0.5,-0.2));
#49648=CARTESIAN_POINT('',(0.23094010767585,-0.5,0.));
#49649=CARTESIAN_POINT('',(0.115470053837925,-0.8,-0.2));
#49650=CARTESIAN_POINT('',(0.115470053837925,-0.5,-0.2));
#49651=CARTESIAN_POINT('',(0.23094010767585,-0.8,0.));
#49652=CARTESIAN_POINT('',(0.23094010767585,-0.8,0.));
#49653=CARTESIAN_POINT('',(0.23094010767585,-0.5,0.));
#49654=CARTESIAN_POINT('Origin',(-0.115470053837925,-0.5,-0.2));
#49655=CARTESIAN_POINT('',(-0.115470053837925,-0.5,-0.2));
#49656=CARTESIAN_POINT('',(0.115470053837925,-0.5,-0.2));
#49657=CARTESIAN_POINT('',(-0.115470053837925,-0.8,-0.2));
#49658=CARTESIAN_POINT('',(-0.115470053837925,-0.5,-0.2));
#49659=CARTESIAN_POINT('',(0.115470053837925,-0.8,-0.2));
#49660=CARTESIAN_POINT('Origin',(-0.23094010767585,-0.5,-2.77555756156289E-17));
#49661=CARTESIAN_POINT('',(-0.23094010767585,-0.5,-2.82820063659975E-17));
#49662=CARTESIAN_POINT('',(-0.115470053837925,-0.5,-0.2));
#49663=CARTESIAN_POINT('',(-0.23094010767585,-0.8,-2.77555756156289E-17));
#49664=CARTESIAN_POINT('',(-0.23094010767585,-0.5,-2.82820063659975E-17));
#49665=CARTESIAN_POINT('',(-0.115470053837925,-0.8,-0.2));
#49666=CARTESIAN_POINT('Origin',(-0.115470053837925,-0.5,0.2));
#49667=CARTESIAN_POINT('',(-0.115470053837925,-0.5,0.2));
#49668=CARTESIAN_POINT('',(-0.23094010767585,-0.5,-2.82820063659975E-17));
#49669=CARTESIAN_POINT('',(-0.115470053837925,-0.8,0.2));
#49670=CARTESIAN_POINT('',(-0.115470053837925,-0.5,0.2));
#49671=CARTESIAN_POINT('',(-0.23094010767585,-0.8,-2.82820063659975E-17));
#49672=CARTESIAN_POINT('Origin',(0.115470053837925,-0.5,0.2));
#49673=CARTESIAN_POINT('',(0.115470053837925,-0.5,0.2));
#49674=CARTESIAN_POINT('',(-0.115470053837925,-0.5,0.2));
#49675=CARTESIAN_POINT('',(0.115470053837925,-0.8,0.2));
#49676=CARTESIAN_POINT('',(0.115470053837925,-0.5,0.2));
#49677=CARTESIAN_POINT('',(-0.115470053837925,-0.8,0.2));
#49678=CARTESIAN_POINT('Origin',(0.23094010767585,-0.5,0.));
#49679=CARTESIAN_POINT('',(0.115470053837925,-0.5,0.2));
#49680=CARTESIAN_POINT('',(0.115470053837925,-0.8,0.2));
#49681=CARTESIAN_POINT('Origin',(0.,-0.5,0.));
#49682=CARTESIAN_POINT('Origin',(0.,-0.8,0.));
#49683=CARTESIAN_POINT('Origin',(0.,-1.4,0.));
#49684=CARTESIAN_POINT('',(-0.24505,-1.4,3.00099698131059E-17));
#49685=CARTESIAN_POINT('Origin',(0.,-1.4,0.));
#49686=CARTESIAN_POINT('Origin',(0.375,0.5,0.));
#49687=CARTESIAN_POINT('',(-0.375,0.5,-4.59242549680257E-17));
#49688=CARTESIAN_POINT('Origin',(0.,0.5,0.));
#49689=CARTESIAN_POINT('Origin',(0.,0.475,0.));
#49690=CARTESIAN_POINT('',(-0.425,0.45,-5.20474889637625E-17));
#49691=CARTESIAN_POINT('Origin',(0.,0.45,0.));
#49692=CARTESIAN_POINT('',(-0.4,0.475,-4.89858719658941E-17));
#49693=CARTESIAN_POINT('Origin',(0.,0.24,0.));
#49694=CARTESIAN_POINT('',(-0.425,0.0299999999999998,-5.20474889637625E-17));
#49695=CARTESIAN_POINT('Origin',(0.,0.0299999999999998,0.));
#49696=CARTESIAN_POINT('',(-0.425,0.24,-5.20474889637625E-17));
#49697=CARTESIAN_POINT('Origin',(0.,0.0150000000000001,0.));
#49698=CARTESIAN_POINT('',(-0.395,4.85722573273506E-17,-4.83735485663204E-17));
#49699=CARTESIAN_POINT('Origin',(0.,0.,0.));
#49700=CARTESIAN_POINT('',(-0.41,0.0150000000000001,-5.02105187650415E-17));
#49701=CARTESIAN_POINT('Origin',(0.27,0.,0.));
#49702=CARTESIAN_POINT('',(-0.27,0.,-3.30654635769785E-17));
#49703=CARTESIAN_POINT('Origin',(0.,0.,0.));
#49704=CARTESIAN_POINT('Origin',(0.,-0.02,0.));
#49705=CARTESIAN_POINT('',(-0.24505,-0.0498999999999999,3.00099698131059E-17));
#49706=CARTESIAN_POINT('Origin',(0.,-0.0498999999999999,0.));
#49707=CARTESIAN_POINT('',(-0.26,-0.02,-3.18408167778312E-17));
#49708=CARTESIAN_POINT('Origin',(0.,-0.995,0.));
#49709=CARTESIAN_POINT('',(-0.24505,-0.995,-3.00099698131059E-17));
#49710=CARTESIAN_POINT('',(0.,0.,0.));
#49711=CARTESIAN_POINT('',(0.,0.,0.));
#49712=CARTESIAN_POINT('Origin',(15.,-7.9,5.1));
#49713=CARTESIAN_POINT('',(14.725,-7.9,5.2));
#49714=CARTESIAN_POINT('Origin',(15.,-7.9,5.2));
#49715=CARTESIAN_POINT('',(14.725,-7.9,6.));
#49716=CARTESIAN_POINT('',(14.725,-7.9,5.1));
#49717=CARTESIAN_POINT('Origin',(15.,-7.9,6.));
#49718=CARTESIAN_POINT('Origin',(12.,-4.1,5.1));
#49719=CARTESIAN_POINT('',(11.725,-4.1,5.2));
#49720=CARTESIAN_POINT('Origin',(12.,-4.1,5.2));
#49721=CARTESIAN_POINT('',(11.725,-4.1,6.));
#49722=CARTESIAN_POINT('',(11.725,-4.1,5.1));
#49723=CARTESIAN_POINT('Origin',(12.,-4.1,6.));
#49724=CARTESIAN_POINT('Origin',(12.,-7.9,5.1));
#49725=CARTESIAN_POINT('',(11.725,-7.9,5.2));
#49726=CARTESIAN_POINT('Origin',(12.,-7.9,5.2));
#49727=CARTESIAN_POINT('',(11.725,-7.9,6.));
#49728=CARTESIAN_POINT('',(11.725,-7.9,5.1));
#49729=CARTESIAN_POINT('Origin',(12.,-7.9,6.));
#49730=CARTESIAN_POINT('Origin',(15.,-4.1,5.1));
#49731=CARTESIAN_POINT('',(14.725,-4.1,5.2));
#49732=CARTESIAN_POINT('Origin',(15.,-4.1,5.2));
#49733=CARTESIAN_POINT('',(14.725,-4.1,6.));
#49734=CARTESIAN_POINT('',(14.725,-4.1,5.1));
#49735=CARTESIAN_POINT('Origin',(15.,-4.1,6.));
#49736=CARTESIAN_POINT('Origin',(16.6,-3.65,5.2));
#49737=CARTESIAN_POINT('',(16.6,-3.65,5.2));
#49738=CARTESIAN_POINT('',(10.4,-3.65,5.2));
#49739=CARTESIAN_POINT('',(16.6,-3.65,5.2));
#49740=CARTESIAN_POINT('',(10.4,-3.65,6.));
#49741=CARTESIAN_POINT('',(10.4,-3.65,5.2));
#49742=CARTESIAN_POINT('',(16.6,-3.65,6.));
#49743=CARTESIAN_POINT('',(16.6,-3.65,6.));
#49744=CARTESIAN_POINT('',(16.6,-3.65,5.2));
#49745=CARTESIAN_POINT('Origin',(16.6,-8.35,5.2));
#49746=CARTESIAN_POINT('',(16.6,-8.35,5.2));
#49747=CARTESIAN_POINT('',(16.6,-8.35,5.2));
#49748=CARTESIAN_POINT('',(16.6,-8.35,6.));
#49749=CARTESIAN_POINT('',(16.6,-8.35,6.));
#49750=CARTESIAN_POINT('',(16.6,-8.35,5.2));
#49751=CARTESIAN_POINT('Origin',(10.4,-8.35,5.2));
#49752=CARTESIAN_POINT('',(10.4,-8.35,5.2));
#49753=CARTESIAN_POINT('',(10.4,-8.35,5.2));
#49754=CARTESIAN_POINT('',(10.4,-8.35,6.));
#49755=CARTESIAN_POINT('',(10.4,-8.35,6.));
#49756=CARTESIAN_POINT('',(10.4,-8.35,5.2));
#49757=CARTESIAN_POINT('Origin',(10.4,-3.65,5.2));
#49758=CARTESIAN_POINT('',(10.4,-3.65,5.2));
#49759=CARTESIAN_POINT('',(10.4,-3.65,6.));
#49760=CARTESIAN_POINT('Origin',(13.5,-6.,6.));
#49761=CARTESIAN_POINT('Origin',(13.5,-6.,5.2));
#49762=CARTESIAN_POINT('',(0.,0.,0.));
#49763=CARTESIAN_POINT('Origin',(14.,-1.5,5.9));
#49764=CARTESIAN_POINT('',(13.725,-1.5,6.));
#49765=CARTESIAN_POINT('Origin',(14.,-1.5,6.));
#49766=CARTESIAN_POINT('',(13.725,-1.5,7.2));
#49767=CARTESIAN_POINT('',(13.725,-1.5,5.9));
#49768=CARTESIAN_POINT('Origin',(14.,-1.5,7.2));
#49769=CARTESIAN_POINT('Origin',(12.5,1.5,5.9));
#49770=CARTESIAN_POINT('',(12.225,1.5,6.));
#49771=CARTESIAN_POINT('Origin',(12.5,1.5,6.));
#49772=CARTESIAN_POINT('',(12.225,1.5,7.2));
#49773=CARTESIAN_POINT('',(12.225,1.5,5.9));
#49774=CARTESIAN_POINT('Origin',(12.5,1.5,7.2));
#49775=CARTESIAN_POINT('Origin',(12.5,-1.5,5.9));
#49776=CARTESIAN_POINT('',(12.225,-1.5,6.));
#49777=CARTESIAN_POINT('Origin',(12.5,-1.5,6.));
#49778=CARTESIAN_POINT('',(12.225,-1.5,7.2));
#49779=CARTESIAN_POINT('',(12.225,-1.5,5.9));
#49780=CARTESIAN_POINT('Origin',(12.5,-1.5,7.2));
#49781=CARTESIAN_POINT('Origin',(14.,1.5,5.9));
#49782=CARTESIAN_POINT('',(13.725,1.5,6.));
#49783=CARTESIAN_POINT('Origin',(14.,1.5,6.));
#49784=CARTESIAN_POINT('',(13.725,1.5,7.2));
#49785=CARTESIAN_POINT('',(13.725,1.5,5.9));
#49786=CARTESIAN_POINT('Origin',(14.,1.5,7.2));
#49787=CARTESIAN_POINT('Origin',(15.,-7.9,5.1));
#49788=CARTESIAN_POINT('',(14.725,-7.9,6.));
#49789=CARTESIAN_POINT('Origin',(15.,-7.9,6.));
#49790=CARTESIAN_POINT('',(14.725,-7.9,7.2));
#49791=CARTESIAN_POINT('',(14.725,-7.9,5.1));
#49792=CARTESIAN_POINT('Origin',(15.,-7.9,7.2));
#49793=CARTESIAN_POINT('Origin',(12.,-4.1,5.1));
#49794=CARTESIAN_POINT('',(11.725,-4.1,6.));
#49795=CARTESIAN_POINT('Origin',(12.,-4.1,6.));
#49796=CARTESIAN_POINT('',(11.725,-4.1,7.2));
#49797=CARTESIAN_POINT('',(11.725,-4.1,5.1));
#49798=CARTESIAN_POINT('Origin',(12.,-4.1,7.2));
#49799=CARTESIAN_POINT('Origin',(12.,-7.9,5.1));
#49800=CARTESIAN_POINT('',(11.725,-7.9,6.));
#49801=CARTESIAN_POINT('Origin',(12.,-7.9,6.));
#49802=CARTESIAN_POINT('',(11.725,-7.9,7.2));
#49803=CARTESIAN_POINT('',(11.725,-7.9,5.1));
#49804=CARTESIAN_POINT('Origin',(12.,-7.9,7.2));
#49805=CARTESIAN_POINT('Origin',(15.,-4.1,5.1));
#49806=CARTESIAN_POINT('',(14.725,-4.1,6.));
#49807=CARTESIAN_POINT('Origin',(15.,-4.1,6.));
#49808=CARTESIAN_POINT('',(14.725,-4.1,7.2));
#49809=CARTESIAN_POINT('',(14.725,-4.1,5.1));
#49810=CARTESIAN_POINT('Origin',(15.,-4.1,7.2));
#49811=CARTESIAN_POINT('Origin',(17.,2.5,6.));
#49812=CARTESIAN_POINT('',(17.,2.5,6.));
#49813=CARTESIAN_POINT('',(10.,2.5,6.));
#49814=CARTESIAN_POINT('',(17.,2.5,6.));
#49815=CARTESIAN_POINT('',(10.,2.5,7.2));
#49816=CARTESIAN_POINT('',(10.,2.5,6.));
#49817=CARTESIAN_POINT('',(17.,2.5,7.2));
#49818=CARTESIAN_POINT('',(17.,2.5,7.2));
#49819=CARTESIAN_POINT('',(17.,2.5,6.));
#49820=CARTESIAN_POINT('Origin',(17.,-10.,6.));
#49821=CARTESIAN_POINT('',(17.,-10.,6.));
#49822=CARTESIAN_POINT('',(17.,-10.,6.));
#49823=CARTESIAN_POINT('',(17.,-10.,7.2));
#49824=CARTESIAN_POINT('',(17.,-10.,7.2));
#49825=CARTESIAN_POINT('',(17.,-10.,6.));
#49826=CARTESIAN_POINT('Origin',(10.,-10.,6.));
#49827=CARTESIAN_POINT('',(10.,-10.,6.));
#49828=CARTESIAN_POINT('',(10.,-10.,6.));
#49829=CARTESIAN_POINT('',(10.,-10.,7.2));
#49830=CARTESIAN_POINT('',(10.,-10.,7.2));
#49831=CARTESIAN_POINT('',(10.,-10.,6.));
#49832=CARTESIAN_POINT('Origin',(10.,2.5,6.));
#49833=CARTESIAN_POINT('',(10.,2.5,6.));
#49834=CARTESIAN_POINT('',(10.,2.5,7.2));
#49835=CARTESIAN_POINT('Origin',(13.5,-3.75,7.2));
#49836=CARTESIAN_POINT('Origin',(13.5,-3.75,6.));
#49837=CARTESIAN_POINT('',(0.,0.,0.));
#49838=CARTESIAN_POINT('Origin',(14.,-1.5,5.1));
#49839=CARTESIAN_POINT('',(13.79,-1.5,5.1));
#49840=CARTESIAN_POINT('Origin',(14.,-1.5,5.1));
#49841=CARTESIAN_POINT('',(13.79,-1.5,6.));
#49842=CARTESIAN_POINT('',(13.79,-1.5,5.1));
#49843=CARTESIAN_POINT('Origin',(14.,-1.5,6.));
#49844=CARTESIAN_POINT('Origin',(14.,-1.5,5.1));
#49845=CARTESIAN_POINT('Origin',(12.5,1.5,5.1));
#49846=CARTESIAN_POINT('',(12.29,1.5,5.1));
#49847=CARTESIAN_POINT('Origin',(12.5,1.5,5.1));
#49848=CARTESIAN_POINT('',(12.29,1.5,6.));
#49849=CARTESIAN_POINT('',(12.29,1.5,5.1));
#49850=CARTESIAN_POINT('Origin',(12.5,1.5,6.));
#49851=CARTESIAN_POINT('Origin',(12.5,1.5,5.1));
#49852=CARTESIAN_POINT('Origin',(12.5,-1.5,5.1));
#49853=CARTESIAN_POINT('',(12.29,-1.5,5.1));
#49854=CARTESIAN_POINT('Origin',(12.5,-1.5,5.1));
#49855=CARTESIAN_POINT('',(12.29,-1.5,6.));
#49856=CARTESIAN_POINT('',(12.29,-1.5,5.1));
#49857=CARTESIAN_POINT('Origin',(12.5,-1.5,6.));
#49858=CARTESIAN_POINT('Origin',(12.5,-1.5,5.1));
#49859=CARTESIAN_POINT('Origin',(14.,1.5,5.1));
#49860=CARTESIAN_POINT('',(13.79,1.5,5.1));
#49861=CARTESIAN_POINT('Origin',(14.,1.5,5.1));
#49862=CARTESIAN_POINT('',(13.79,1.5,6.));
#49863=CARTESIAN_POINT('',(13.79,1.5,5.1));
#49864=CARTESIAN_POINT('Origin',(14.,1.5,6.));
#49865=CARTESIAN_POINT('Origin',(14.,1.5,5.1));
#49866=CARTESIAN_POINT('Origin',(12.9,-1.5,4.));
#49867=CARTESIAN_POINT('',(12.9,-1.5,4.165));
#49868=CARTESIAN_POINT('Origin',(12.9,-1.5,4.));
#49869=CARTESIAN_POINT('',(14.5,-1.5,4.165));
#49870=CARTESIAN_POINT('',(12.9,-1.5,4.165));
#49871=CARTESIAN_POINT('Origin',(14.5,-1.5,4.));
#49872=CARTESIAN_POINT('Origin',(12.9,-1.5,4.));
#49873=CARTESIAN_POINT('Origin',(12.9,1.5,4.));
#49874=CARTESIAN_POINT('',(12.9,1.5,4.165));
#49875=CARTESIAN_POINT('Origin',(12.9,1.5,4.));
#49876=CARTESIAN_POINT('',(14.5,1.5,4.165));
#49877=CARTESIAN_POINT('',(12.9,1.5,4.165));
#49878=CARTESIAN_POINT('Origin',(14.5,1.5,4.));
#49879=CARTESIAN_POINT('Origin',(12.9,1.5,4.));
#49880=CARTESIAN_POINT('Origin',(12.9,0.,5.5));
#49881=CARTESIAN_POINT('',(12.9,-2.02066721859313E-17,5.665));
#49882=CARTESIAN_POINT('Origin',(12.9,0.,5.5));
#49883=CARTESIAN_POINT('',(14.5,2.02066721859313E-17,5.665));
#49884=CARTESIAN_POINT('',(12.9,-2.02066721859313E-17,5.665));
#49885=CARTESIAN_POINT('Origin',(14.5,0.,5.5));
#49886=CARTESIAN_POINT('Origin',(12.9,0.,5.5));
#49887=CARTESIAN_POINT('Origin',(11.9,0.,4.));
#49888=CARTESIAN_POINT('',(12.,-1.35935794705356E-16,5.11));
#49889=CARTESIAN_POINT('Origin',(12.,0.,4.));
#49890=CARTESIAN_POINT('',(14.5,1.35935794705356E-16,5.11));
#49891=CARTESIAN_POINT('',(11.9,-1.35935794705356E-16,5.11));
#49892=CARTESIAN_POINT('Origin',(14.5,0.,4.));
#49893=CARTESIAN_POINT('Origin',(14.5,2.2,2.5));
#49894=CARTESIAN_POINT('',(14.5,2.2,2.5));
#49895=CARTESIAN_POINT('',(12.,2.2,2.5));
#49896=CARTESIAN_POINT('',(14.5,2.2,2.5));
#49897=CARTESIAN_POINT('',(12.,2.2,6.));
#49898=CARTESIAN_POINT('',(12.,2.2,2.5));
#49899=CARTESIAN_POINT('',(14.5,2.2,6.));
#49900=CARTESIAN_POINT('',(14.5,2.2,6.));
#49901=CARTESIAN_POINT('',(14.5,2.2,2.5));
#49902=CARTESIAN_POINT('Origin',(14.5,-2.2,2.5));
#49903=CARTESIAN_POINT('',(14.5,-2.2,2.5));
#49904=CARTESIAN_POINT('',(14.5,-2.2,2.5));
#49905=CARTESIAN_POINT('',(14.5,-2.2,6.));
#49906=CARTESIAN_POINT('',(14.5,-2.2,6.));
#49907=CARTESIAN_POINT('',(14.5,-2.2,2.5));
#49908=CARTESIAN_POINT('Origin',(12.,-2.2,2.5));
#49909=CARTESIAN_POINT('',(12.,-2.2,2.5));
#49910=CARTESIAN_POINT('',(12.,-2.2,2.5));
#49911=CARTESIAN_POINT('',(12.,-2.2,6.));
#49912=CARTESIAN_POINT('',(12.,-2.2,6.));
#49913=CARTESIAN_POINT('',(12.,-2.2,2.5));
#49914=CARTESIAN_POINT('Origin',(12.,2.2,2.5));
#49915=CARTESIAN_POINT('',(12.,2.2,2.5));
#49916=CARTESIAN_POINT('',(12.,2.2,6.));
#49917=CARTESIAN_POINT('Origin',(13.25,0.,6.));
#49918=CARTESIAN_POINT('Origin',(13.25,0.,2.5));
#49919=CARTESIAN_POINT('',(0.,0.,0.));
#49920=CARTESIAN_POINT('',(0.,0.,0.));
#49921=CARTESIAN_POINT('Origin',(1.5,-1.9,1.7));
#49922=CARTESIAN_POINT('',(1.56403124237433,-1.7,1.7));
#49923=CARTESIAN_POINT('',(1.43596875762567,-1.7,1.7));
#49924=CARTESIAN_POINT('',(0.75,-1.7,1.7));
#49925=CARTESIAN_POINT('Origin',(1.5,-1.9,1.7));
#49926=CARTESIAN_POINT('Origin',(1.5,-1.9,1.7));
#49927=CARTESIAN_POINT('',(1.56403124237433,-1.7,1.75));
#49928=CARTESIAN_POINT('',(1.56403124237433,-1.7,1.7));
#49929=CARTESIAN_POINT('',(1.29,-1.9,1.75));
#49930=CARTESIAN_POINT('Origin',(1.5,-1.9,1.75));
#49931=CARTESIAN_POINT('',(1.29,-1.9,2.4));
#49932=CARTESIAN_POINT('',(1.29,-1.9,1.7));
#49933=CARTESIAN_POINT('Origin',(1.5,-1.9,2.4));
#49934=CARTESIAN_POINT('',(1.43596875762567,-1.7,1.75));
#49935=CARTESIAN_POINT('Origin',(1.5,-1.9,1.75));
#49936=CARTESIAN_POINT('',(1.43596875762567,-1.7,1.7));
#49937=CARTESIAN_POINT('Origin',(-1.5,1.9,1.7));
#49938=CARTESIAN_POINT('',(-1.56403124237433,1.7,1.7));
#49939=CARTESIAN_POINT('',(-1.43596875762567,1.7,1.7));
#49940=CARTESIAN_POINT('',(-0.75,1.7,1.7));
#49941=CARTESIAN_POINT('Origin',(-1.5,1.9,1.7));
#49942=CARTESIAN_POINT('Origin',(-1.5,1.9,1.7));
#49943=CARTESIAN_POINT('',(-1.56403124237433,1.7,1.75));
#49944=CARTESIAN_POINT('',(-1.56403124237433,1.7,1.7));
#49945=CARTESIAN_POINT('',(-1.71,1.9,1.75));
#49946=CARTESIAN_POINT('Origin',(-1.5,1.9,1.75));
#49947=CARTESIAN_POINT('',(-1.71,1.9,2.4));
#49948=CARTESIAN_POINT('',(-1.71,1.9,1.7));
#49949=CARTESIAN_POINT('Origin',(-1.5,1.9,2.4));
#49950=CARTESIAN_POINT('',(-1.43596875762567,1.7,1.75));
#49951=CARTESIAN_POINT('Origin',(-1.5,1.9,1.75));
#49952=CARTESIAN_POINT('',(-1.43596875762567,1.7,1.7));
#49953=CARTESIAN_POINT('Origin',(-1.5,-1.9,1.7));
#49954=CARTESIAN_POINT('',(-1.43596875762567,-1.7,1.7));
#49955=CARTESIAN_POINT('',(-1.56403124237433,-1.7,1.7));
#49956=CARTESIAN_POINT('',(-0.75,-1.7,1.7));
#49957=CARTESIAN_POINT('Origin',(-1.5,-1.9,1.7));
#49958=CARTESIAN_POINT('Origin',(-1.5,-1.9,1.7));
#49959=CARTESIAN_POINT('',(-1.43596875762567,-1.7,1.75));
#49960=CARTESIAN_POINT('',(-1.43596875762567,-1.7,1.7));
#49961=CARTESIAN_POINT('',(-1.71,-1.9,1.75));
#49962=CARTESIAN_POINT('Origin',(-1.5,-1.9,1.75));
#49963=CARTESIAN_POINT('',(-1.71,-1.9,2.4));
#49964=CARTESIAN_POINT('',(-1.71,-1.9,1.7));
#49965=CARTESIAN_POINT('Origin',(-1.5,-1.9,2.4));
#49966=CARTESIAN_POINT('',(-1.56403124237433,-1.7,1.75));
#49967=CARTESIAN_POINT('Origin',(-1.5,-1.9,1.75));
#49968=CARTESIAN_POINT('',(-1.56403124237433,-1.7,1.7));
#49969=CARTESIAN_POINT('Origin',(1.5,1.9,1.7));
#49970=CARTESIAN_POINT('',(1.43596875762567,1.7,1.7));
#49971=CARTESIAN_POINT('',(1.56403124237433,1.7,1.7));
#49972=CARTESIAN_POINT('',(0.75,1.7,1.7));
#49973=CARTESIAN_POINT('Origin',(1.5,1.9,1.7));
#49974=CARTESIAN_POINT('Origin',(1.5,1.9,1.7));
#49975=CARTESIAN_POINT('',(1.43596875762567,1.7,1.75));
#49976=CARTESIAN_POINT('',(1.43596875762567,1.7,1.7));
#49977=CARTESIAN_POINT('',(1.29,1.9,1.75));
#49978=CARTESIAN_POINT('Origin',(1.5,1.9,1.75));
#49979=CARTESIAN_POINT('',(1.29,1.9,2.4));
#49980=CARTESIAN_POINT('',(1.29,1.9,1.7));
#49981=CARTESIAN_POINT('Origin',(1.5,1.9,2.4));
#49982=CARTESIAN_POINT('',(1.56403124237433,1.7,1.75));
#49983=CARTESIAN_POINT('Origin',(1.5,1.9,1.75));
#49984=CARTESIAN_POINT('',(1.56403124237433,1.7,1.7));
#49985=CARTESIAN_POINT('Origin',(0.,-1.7,1.75));
#49986=CARTESIAN_POINT('',(0.,-1.7,1.75));
#49987=CARTESIAN_POINT('',(-1.97,-1.7,1.75));
#49988=CARTESIAN_POINT('',(0.,-1.7,1.75));
#49989=CARTESIAN_POINT('',(-1.97,-1.7,0.43));
#49990=CARTESIAN_POINT('',(-1.97,-1.7,1.75));
#49991=CARTESIAN_POINT('',(1.97,-1.7,0.43));
#49992=CARTESIAN_POINT('',(0.,-1.7,0.43));
#49993=CARTESIAN_POINT('',(1.97,-1.7,1.75));
#49994=CARTESIAN_POINT('',(1.97,-1.7,1.75));
#49995=CARTESIAN_POINT('',(0.,-1.7,1.75));
#49996=CARTESIAN_POINT('Origin',(0.,1.7,0.43));
#49997=CARTESIAN_POINT('',(0.,1.7,1.75));
#49998=CARTESIAN_POINT('',(1.97,1.7,1.75));
#49999=CARTESIAN_POINT('',(0.,1.7,1.75));
#50000=CARTESIAN_POINT('',(1.97,1.7,0.43));
#50001=CARTESIAN_POINT('',(1.97,1.7,0.43));
#50002=CARTESIAN_POINT('',(-1.97,1.7,0.43));
#50003=CARTESIAN_POINT('',(0.,1.7,0.43));
#50004=CARTESIAN_POINT('',(-1.97,1.7,1.75));
#50005=CARTESIAN_POINT('',(-1.97,1.7,0.43));
#50006=CARTESIAN_POINT('',(0.,1.7,1.75));
#50007=CARTESIAN_POINT('Origin',(-1.97,0.,1.415));
#50008=CARTESIAN_POINT('',(-1.97,-2.35,1.75));
#50009=CARTESIAN_POINT('',(-1.97,-2.35,1.75));
#50010=CARTESIAN_POINT('',(-1.97,-2.35,2.4));
#50011=CARTESIAN_POINT('',(-1.97,-2.35,2.4));
#50012=CARTESIAN_POINT('',(-1.97,2.35,2.4));
#50013=CARTESIAN_POINT('',(-1.97,2.35,2.4));
#50014=CARTESIAN_POINT('',(-1.97,2.35,1.75));
#50015=CARTESIAN_POINT('',(-1.97,2.35,1.75));
#50016=CARTESIAN_POINT('',(-1.97,1.7,1.75));
#50017=CARTESIAN_POINT('',(-1.97,0.78,0.43));
#50018=CARTESIAN_POINT('',(-1.97,0.78,0.43));
#50019=CARTESIAN_POINT('',(-1.97,0.78,1.55));
#50020=CARTESIAN_POINT('',(-1.97,0.78,1.55));
#50021=CARTESIAN_POINT('',(-1.97,-0.78,1.55));
#50022=CARTESIAN_POINT('',(-1.97,-0.78,1.55));
#50023=CARTESIAN_POINT('',(-1.97,-0.78,0.43));
#50024=CARTESIAN_POINT('',(-1.97,-0.78,0.43));
#50025=CARTESIAN_POINT('',(-1.97,-1.7,0.43));
#50026=CARTESIAN_POINT('Origin',(0.,-2.35,1.75));
#50027=CARTESIAN_POINT('',(1.97,-2.35,1.75));
#50028=CARTESIAN_POINT('',(1.97,-2.35,1.75));
#50029=CARTESIAN_POINT('',(0.,-2.35,1.75));
#50030=CARTESIAN_POINT('Origin',(0.,-2.35,2.4));
#50031=CARTESIAN_POINT('',(1.97,-2.35,2.4));
#50032=CARTESIAN_POINT('',(1.97,-2.35,2.4));
#50033=CARTESIAN_POINT('',(0.,-2.35,2.4));
#50034=CARTESIAN_POINT('Origin',(0.,2.35,2.4));
#50035=CARTESIAN_POINT('',(1.97,2.35,2.4));
#50036=CARTESIAN_POINT('',(1.97,2.35,2.4));
#50037=CARTESIAN_POINT('',(0.,2.35,2.4));
#50038=CARTESIAN_POINT('Origin',(0.,2.35,1.75));
#50039=CARTESIAN_POINT('',(1.97,2.35,1.75));
#50040=CARTESIAN_POINT('',(1.97,2.35,1.75));
#50041=CARTESIAN_POINT('',(0.,2.35,1.75));
#50042=CARTESIAN_POINT('Origin',(0.,1.7,1.75));
#50043=CARTESIAN_POINT('',(1.97,1.7,1.75));
#50044=CARTESIAN_POINT('Origin',(0.,0.78,0.43));
#50045=CARTESIAN_POINT('',(1.97,0.78,0.43));
#50046=CARTESIAN_POINT('',(1.97,0.78,0.43));
#50047=CARTESIAN_POINT('',(0.,0.78,0.43));
#50048=CARTESIAN_POINT('Origin',(0.,0.78,1.55));
#50049=CARTESIAN_POINT('',(1.97,0.78,1.55));
#50050=CARTESIAN_POINT('',(1.97,0.78,1.55));
#50051=CARTESIAN_POINT('',(0.,0.78,1.55));
#50052=CARTESIAN_POINT('Origin',(0.,-0.78,1.55));
#50053=CARTESIAN_POINT('',(1.97,-0.78,1.55));
#50054=CARTESIAN_POINT('',(1.97,-0.78,1.55));
#50055=CARTESIAN_POINT('',(0.,-0.78,1.55));
#50056=CARTESIAN_POINT('Origin',(0.,-0.78,0.43));
#50057=CARTESIAN_POINT('',(1.97,-0.78,0.43));
#50058=CARTESIAN_POINT('',(1.97,-0.78,0.43));
#50059=CARTESIAN_POINT('',(0.,-0.78,0.43));
#50060=CARTESIAN_POINT('Origin',(0.,-1.7,0.43));
#50061=CARTESIAN_POINT('',(1.97,-1.7,0.43));
#50062=CARTESIAN_POINT('Origin',(1.97,0.,1.415));
#50063=CARTESIAN_POINT('',(0.,0.,0.));
#50064=CARTESIAN_POINT('Origin',(1.97,1.7,2.3));
#50065=CARTESIAN_POINT('',(1.97,1.7,2.3));
#50066=CARTESIAN_POINT('',(1.97,-1.7,2.3));
#50067=CARTESIAN_POINT('',(1.97,1.7,2.3));
#50068=CARTESIAN_POINT('',(3.07,-1.7,2.3));
#50069=CARTESIAN_POINT('',(1.97,-1.7,2.3));
#50070=CARTESIAN_POINT('',(3.07,1.7,2.3));
#50071=CARTESIAN_POINT('',(3.07,1.7,2.3));
#50072=CARTESIAN_POINT('',(1.97,1.7,2.3));
#50073=CARTESIAN_POINT('Origin',(1.97,1.7,0.46));
#50074=CARTESIAN_POINT('',(1.97,1.7,0.46));
#50075=CARTESIAN_POINT('',(1.97,1.7,0.46));
#50076=CARTESIAN_POINT('',(3.07,1.7,0.46));
#50077=CARTESIAN_POINT('',(3.07,1.7,0.46));
#50078=CARTESIAN_POINT('',(1.97,1.7,0.46));
#50079=CARTESIAN_POINT('Origin',(1.97,0.78,0.46));
#50080=CARTESIAN_POINT('',(1.97,0.78,0.46));
#50081=CARTESIAN_POINT('',(1.97,0.78,0.46));
#50082=CARTESIAN_POINT('',(3.07,0.78,0.46));
#50083=CARTESIAN_POINT('',(3.07,0.78,0.46));
#50084=CARTESIAN_POINT('',(1.97,0.78,0.46));
#50085=CARTESIAN_POINT('Origin',(1.97,0.78,1.55));
#50086=CARTESIAN_POINT('',(1.97,0.78,1.55));
#50087=CARTESIAN_POINT('',(1.97,0.78,1.55));
#50088=CARTESIAN_POINT('',(3.07,0.78,1.55));
#50089=CARTESIAN_POINT('',(3.07,0.78,1.55));
#50090=CARTESIAN_POINT('',(1.97,0.78,1.55));
#50091=CARTESIAN_POINT('Origin',(1.97,-0.78,1.55));
#50092=CARTESIAN_POINT('',(1.97,-0.78,1.55));
#50093=CARTESIAN_POINT('',(1.97,-0.78,1.55));
#50094=CARTESIAN_POINT('',(3.07,-0.78,1.55));
#50095=CARTESIAN_POINT('',(3.07,-0.78,1.55));
#50096=CARTESIAN_POINT('',(1.97,-0.78,1.55));
#50097=CARTESIAN_POINT('Origin',(1.97,-0.78,0.46));
#50098=CARTESIAN_POINT('',(1.97,-0.78,0.46));
#50099=CARTESIAN_POINT('',(1.97,-0.78,0.46));
#50100=CARTESIAN_POINT('',(3.07,-0.78,0.46));
#50101=CARTESIAN_POINT('',(3.07,-0.78,0.46));
#50102=CARTESIAN_POINT('',(1.97,-0.78,0.46));
#50103=CARTESIAN_POINT('Origin',(1.97,-1.7,0.46));
#50104=CARTESIAN_POINT('',(1.97,-1.7,0.46));
#50105=CARTESIAN_POINT('',(1.97,-1.7,0.46));
#50106=CARTESIAN_POINT('',(3.07,-1.7,0.46));
#50107=CARTESIAN_POINT('',(3.07,-1.7,0.46));
#50108=CARTESIAN_POINT('',(1.97,-1.7,0.46));
#50109=CARTESIAN_POINT('Origin',(1.97,-1.7,2.3));
#50110=CARTESIAN_POINT('',(1.97,-1.7,2.3));
#50111=CARTESIAN_POINT('',(3.07,-1.7,2.3));
#50112=CARTESIAN_POINT('Origin',(3.07,0.,1.38));
#50113=CARTESIAN_POINT('Origin',(1.97,0.,1.38));
#50114=CARTESIAN_POINT('',(0.,0.,0.));
#50115=CARTESIAN_POINT('Origin',(-1.97,-0.78,0.46));
#50116=CARTESIAN_POINT('',(-1.97,-1.7,0.46));
#50117=CARTESIAN_POINT('',(-1.97,-0.78,0.46));
#50118=CARTESIAN_POINT('',(-1.97,-1.7,0.46));
#50119=CARTESIAN_POINT('',(-3.07,-1.7,0.46));
#50120=CARTESIAN_POINT('',(-1.97,-1.7,0.46));
#50121=CARTESIAN_POINT('',(-3.07,-0.78,0.46));
#50122=CARTESIAN_POINT('',(-3.07,-1.7,0.46));
#50123=CARTESIAN_POINT('',(-1.97,-0.78,0.46));
#50124=CARTESIAN_POINT('Origin',(-1.97,-0.78,1.55));
#50125=CARTESIAN_POINT('',(-1.97,-0.78,1.55));
#50126=CARTESIAN_POINT('',(-1.97,-0.78,0.46));
#50127=CARTESIAN_POINT('',(-3.07,-0.78,1.55));
#50128=CARTESIAN_POINT('',(-3.07,-0.78,0.46));
#50129=CARTESIAN_POINT('',(-1.97,-0.78,1.55));
#50130=CARTESIAN_POINT('Origin',(-1.97,0.78,1.55));
#50131=CARTESIAN_POINT('',(-1.97,0.78,1.55));
#50132=CARTESIAN_POINT('',(-1.97,-0.78,1.55));
#50133=CARTESIAN_POINT('',(-3.07,0.78,1.55));
#50134=CARTESIAN_POINT('',(-3.07,-0.78,1.55));
#50135=CARTESIAN_POINT('',(-1.97,0.78,1.55));
#50136=CARTESIAN_POINT('Origin',(-1.97,0.78,0.46));
#50137=CARTESIAN_POINT('',(-1.97,0.78,0.46));
#50138=CARTESIAN_POINT('',(-1.97,0.78,1.55));
#50139=CARTESIAN_POINT('',(-3.07,0.78,0.46));
#50140=CARTESIAN_POINT('',(-3.07,0.78,1.55));
#50141=CARTESIAN_POINT('',(-1.97,0.78,0.46));
#50142=CARTESIAN_POINT('Origin',(-1.97,1.7,0.46));
#50143=CARTESIAN_POINT('',(-1.97,1.7,0.46));
#50144=CARTESIAN_POINT('',(-1.97,0.78,0.46));
#50145=CARTESIAN_POINT('',(-3.07,1.7,0.46));
#50146=CARTESIAN_POINT('',(-3.07,0.78,0.46));
#50147=CARTESIAN_POINT('',(-1.97,1.7,0.46));
#50148=CARTESIAN_POINT('Origin',(-1.97,1.7,2.3));
#50149=CARTESIAN_POINT('',(-1.97,1.7,2.3));
#50150=CARTESIAN_POINT('',(-1.97,1.7,0.46));
#50151=CARTESIAN_POINT('',(-3.07,1.7,2.3));
#50152=CARTESIAN_POINT('',(-3.07,1.7,0.46));
#50153=CARTESIAN_POINT('',(-1.97,1.7,2.3));
#50154=CARTESIAN_POINT('Origin',(-1.97,-1.7,2.3));
#50155=CARTESIAN_POINT('',(-1.97,-1.7,2.3));
#50156=CARTESIAN_POINT('',(-1.97,1.7,2.3));
#50157=CARTESIAN_POINT('',(-3.07,-1.7,2.3));
#50158=CARTESIAN_POINT('',(-3.07,1.7,2.3));
#50159=CARTESIAN_POINT('',(-1.97,-1.7,2.3));
#50160=CARTESIAN_POINT('Origin',(-1.97,-1.7,0.46));
#50161=CARTESIAN_POINT('',(-1.97,-1.7,2.3));
#50162=CARTESIAN_POINT('',(-3.07,-1.7,2.3));
#50163=CARTESIAN_POINT('Origin',(-1.97,0.,1.38));
#50164=CARTESIAN_POINT('Origin',(-3.07,0.,1.38));
#50165=CARTESIAN_POINT('',(0.,0.,0.));
#50166=CARTESIAN_POINT('',(0.,0.,0.));
#50167=CARTESIAN_POINT('',(0.,0.,0.));
#50168=CARTESIAN_POINT('',(0.,0.,0.));
#50169=CARTESIAN_POINT('Origin',(0.,0.09,0.));
#50170=CARTESIAN_POINT('',(-0.285,0.1,3.49024337756996E-17));
#50171=CARTESIAN_POINT('Origin',(0.,0.1,0.));
#50172=CARTESIAN_POINT('',(-0.265,0.08,-3.24531401774049E-17));
#50173=CARTESIAN_POINT('',(-0.275,0.09,3.36777869765522E-17));
#50174=CARTESIAN_POINT('Origin',(0.,0.08,0.));
#50175=CARTESIAN_POINT('Origin',(0.,0.,0.));
#50176=CARTESIAN_POINT('',(-0.265,0.,3.24531401774049E-17));
#50177=CARTESIAN_POINT('',(-0.265,0.,3.24531401774049E-17));
#50178=CARTESIAN_POINT('Origin',(0.,0.,0.));
#50179=CARTESIAN_POINT('Origin',(0.,0.1,0.));
#50180=CARTESIAN_POINT('',(-0.5,0.1,6.12323399573677E-17));
#50181=CARTESIAN_POINT('Origin',(0.,0.1,0.));
#50182=CARTESIAN_POINT('Origin',(0.,0.,0.));
#50183=CARTESIAN_POINT('',(-0.5,0.,6.12323399573677E-17));
#50184=CARTESIAN_POINT('',(-0.5,0.,6.12323399573677E-17));
#50185=CARTESIAN_POINT('Origin',(0.,0.,0.));
#50186=CARTESIAN_POINT('Origin',(0.,0.,0.));
#50187=CARTESIAN_POINT('',(0.,0.,0.));
#50188=CARTESIAN_POINT('Origin',(0.115470053837925,-0.5,-0.2));
#50189=CARTESIAN_POINT('',(0.23094010767585,-0.5,0.));
#50190=CARTESIAN_POINT('',(0.115470053837925,-0.5,-0.2));
#50191=CARTESIAN_POINT('',(0.23094010767585,-0.5,0.));
#50192=CARTESIAN_POINT('',(0.115470053837925,-0.8,-0.2));
#50193=CARTESIAN_POINT('',(0.115470053837925,-0.5,-0.2));
#50194=CARTESIAN_POINT('',(0.23094010767585,-0.8,0.));
#50195=CARTESIAN_POINT('',(0.23094010767585,-0.8,0.));
#50196=CARTESIAN_POINT('',(0.23094010767585,-0.5,0.));
#50197=CARTESIAN_POINT('Origin',(-0.115470053837925,-0.5,-0.2));
#50198=CARTESIAN_POINT('',(-0.115470053837925,-0.5,-0.2));
#50199=CARTESIAN_POINT('',(0.115470053837925,-0.5,-0.2));
#50200=CARTESIAN_POINT('',(-0.115470053837925,-0.8,-0.2));
#50201=CARTESIAN_POINT('',(-0.115470053837925,-0.5,-0.2));
#50202=CARTESIAN_POINT('',(0.115470053837925,-0.8,-0.2));
#50203=CARTESIAN_POINT('Origin',(-0.23094010767585,-0.5,-2.77555756156289E-17));
#50204=CARTESIAN_POINT('',(-0.23094010767585,-0.5,-2.82820063659975E-17));
#50205=CARTESIAN_POINT('',(-0.115470053837925,-0.5,-0.2));
#50206=CARTESIAN_POINT('',(-0.23094010767585,-0.8,-2.77555756156289E-17));
#50207=CARTESIAN_POINT('',(-0.23094010767585,-0.5,-2.82820063659975E-17));
#50208=CARTESIAN_POINT('',(-0.115470053837925,-0.8,-0.2));
#50209=CARTESIAN_POINT('Origin',(-0.115470053837925,-0.5,0.2));
#50210=CARTESIAN_POINT('',(-0.115470053837925,-0.5,0.2));
#50211=CARTESIAN_POINT('',(-0.23094010767585,-0.5,-2.82820063659975E-17));
#50212=CARTESIAN_POINT('',(-0.115470053837925,-0.8,0.2));
#50213=CARTESIAN_POINT('',(-0.115470053837925,-0.5,0.2));
#50214=CARTESIAN_POINT('',(-0.23094010767585,-0.8,-2.82820063659975E-17));
#50215=CARTESIAN_POINT('Origin',(0.115470053837925,-0.5,0.2));
#50216=CARTESIAN_POINT('',(0.115470053837925,-0.5,0.2));
#50217=CARTESIAN_POINT('',(-0.115470053837925,-0.5,0.2));
#50218=CARTESIAN_POINT('',(0.115470053837925,-0.8,0.2));
#50219=CARTESIAN_POINT('',(0.115470053837925,-0.5,0.2));
#50220=CARTESIAN_POINT('',(-0.115470053837925,-0.8,0.2));
#50221=CARTESIAN_POINT('Origin',(0.23094010767585,-0.5,0.));
#50222=CARTESIAN_POINT('',(0.115470053837925,-0.5,0.2));
#50223=CARTESIAN_POINT('',(0.115470053837925,-0.8,0.2));
#50224=CARTESIAN_POINT('Origin',(0.,-0.5,0.));
#50225=CARTESIAN_POINT('Origin',(0.,-0.8,0.));
#50226=CARTESIAN_POINT('Origin',(0.,-1.9,0.));
#50227=CARTESIAN_POINT('',(-0.25,-1.9,3.06161699786838E-17));
#50228=CARTESIAN_POINT('Origin',(0.,-1.9,0.));
#50229=CARTESIAN_POINT('',(-0.24505,-1.9,3.00099698131059E-17));
#50230=CARTESIAN_POINT('Origin',(0.,-1.9,0.));
#50231=CARTESIAN_POINT('Origin',(0.,-3.,0.));
#50232=CARTESIAN_POINT('',(-0.25,-3.,3.06161699786838E-17));
#50233=CARTESIAN_POINT('',(-0.25,-3.,3.06161699786838E-17));
#50234=CARTESIAN_POINT('Origin',(0.,-3.,0.));
#50235=CARTESIAN_POINT('Origin',(0.,-3.,0.));
#50236=CARTESIAN_POINT('Origin',(0.375,0.5,0.));
#50237=CARTESIAN_POINT('',(-0.375,0.5,-4.59242549680257E-17));
#50238=CARTESIAN_POINT('Origin',(0.,0.5,0.));
#50239=CARTESIAN_POINT('Origin',(0.,0.475,0.));
#50240=CARTESIAN_POINT('',(-0.425,0.45,-5.20474889637625E-17));
#50241=CARTESIAN_POINT('Origin',(0.,0.45,0.));
#50242=CARTESIAN_POINT('',(-0.4,0.475,-4.89858719658941E-17));
#50243=CARTESIAN_POINT('Origin',(0.,0.24,0.));
#50244=CARTESIAN_POINT('',(-0.425,0.0299999999999998,-5.20474889637625E-17));
#50245=CARTESIAN_POINT('Origin',(0.,0.0299999999999998,0.));
#50246=CARTESIAN_POINT('',(-0.425,0.24,-5.20474889637625E-17));
#50247=CARTESIAN_POINT('Origin',(0.,0.0150000000000001,0.));
#50248=CARTESIAN_POINT('',(-0.395,4.85722573273506E-17,-4.83735485663204E-17));
#50249=CARTESIAN_POINT('Origin',(0.,0.,0.));
#50250=CARTESIAN_POINT('',(-0.41,0.0150000000000001,-5.02105187650415E-17));
#50251=CARTESIAN_POINT('Origin',(0.27,0.,0.));
#50252=CARTESIAN_POINT('',(-0.27,0.,-3.30654635769785E-17));
#50253=CARTESIAN_POINT('Origin',(0.,0.,0.));
#50254=CARTESIAN_POINT('Origin',(0.,-0.02,0.));
#50255=CARTESIAN_POINT('',(-0.24505,-0.0498999999999999,3.00099698131059E-17));
#50256=CARTESIAN_POINT('Origin',(0.,-0.0498999999999999,0.));
#50257=CARTESIAN_POINT('',(-0.26,-0.02,-3.18408167778312E-17));
#50258=CARTESIAN_POINT('Origin',(0.,-0.995,0.));
#50259=CARTESIAN_POINT('',(-0.24505,-0.995,-3.00099698131059E-17));
#50260=CARTESIAN_POINT('',(0.,0.,0.));
#50261=CARTESIAN_POINT('Origin',(12.5,0.,4.));
#50262=CARTESIAN_POINT('',(12.7800042915148,-1.13874042544416E-5,4.45787212683272));
#50263=CARTESIAN_POINT('',(12.6699957084852,1.09516003635735E-5,4.45788309353564));
#50264=CARTESIAN_POINT('',(12.5,-5.60735153159594E-17,4.457875));
#50265=CARTESIAN_POINT('',(12.5,-0.186196943290586,3.58169363627331));
#50266=CARTESIAN_POINT('Ctrl Pts',(12.6699957084852,1.09516003635735E-5,
4.45788309353564));
#50267=CARTESIAN_POINT('Ctrl Pts',(12.6684300766731,0.0150239422001319,
4.45789815019349));
#50268=CARTESIAN_POINT('Ctrl Pts',(12.6668644448611,0.0300354905662504,
4.45717403092565));
#50269=CARTESIAN_POINT('Ctrl Pts',(12.6652988130491,0.0449730203321769,
4.45569984746698));
#50270=CARTESIAN_POINT('Ctrl Pts',(12.6574274409991,0.120072959788606,4.44828824124903));
#50271=CARTESIAN_POINT('Ctrl Pts',(12.6495560689492,0.193301947984492,4.42191743369942));
#50272=CARTESIAN_POINT('Ctrl Pts',(12.6416846968992,0.255884660534875,4.37974732787395));
#50273=CARTESIAN_POINT('Ctrl Pts',(12.6338133248492,0.318467373085258,4.33757722204849));
#50274=CARTESIAN_POINT('Ctrl Pts',(12.6259419527993,0.370403809990138,4.27960781794716));
#50275=CARTESIAN_POINT('Ctrl Pts',(12.6180705807493,0.405471379329245,4.2127856577826));
#50276=CARTESIAN_POINT('Ctrl Pts',(12.6101992086994,0.440538948668352,4.14596349761803));
#50277=CARTESIAN_POINT('Ctrl Pts',(12.6023278366494,0.458737650441686,4.07028858139023));
#50278=CARTESIAN_POINT('Ctrl Pts',(12.5944564645995,0.457884906392306,3.99482861029462));
#50279=CARTESIAN_POINT('Ctrl Pts',(12.5865850925495,0.457032162342926,3.91936863919901));
#50280=CARTESIAN_POINT('Ctrl Pts',(12.5787137204996,0.437127972470831,3.84412361323559));
#50281=CARTESIAN_POINT('Ctrl Pts',(12.5708423484496,0.400561475243013,3.77811083326841));
#50282=CARTESIAN_POINT('Ctrl Pts',(12.5629709763996,0.363994978015195,3.71209805330123));
#50283=CARTESIAN_POINT('Ctrl Pts',(12.5550996043497,0.310766173431653,3.6553175193303));
#50284=CARTESIAN_POINT('Ctrl Pts',(12.5472282322997,0.247245050961511,3.61457214242492));
#50285=CARTESIAN_POINT('Ctrl Pts',(12.5393568602498,0.183723928491369,3.57382676551955));
#50286=CARTESIAN_POINT('Ctrl Pts',(12.5314854881998,0.109910488134627,3.54911654567973));
#50287=CARTESIAN_POINT('Ctrl Pts',(12.5236141161499,0.034670519197381,3.5434092666393));
#50288=CARTESIAN_POINT('Ctrl Pts',(12.5157427440999,-0.0405694497398647,
3.53770198759887));
#50289=CARTESIAN_POINT('Ctrl Pts',(12.50787137205,-0.117235947257613,3.55099764935784));
#50290=CARTESIAN_POINT('Ctrl Pts',(12.5,-0.186196943290592,3.58169363627332));
#50291=CARTESIAN_POINT('',(12.5,-0.186217277007329,4.41832740439831));
#50292=CARTESIAN_POINT('Origin',(12.5,0.,4.));
#50293=CARTESIAN_POINT('Ctrl Pts',(12.5,-0.186217277007329,4.41832740439831));
#50294=CARTESIAN_POINT('Ctrl Pts',(12.5008157411716,-0.193365324225124,
4.41515241707318));
#50295=CARTESIAN_POINT('Ctrl Pts',(12.5016314823431,-0.200430783441492,
4.4117927098014));
#50296=CARTESIAN_POINT('Ctrl Pts',(12.5024472235147,-0.207403505574881,
4.40825058102053));
#50297=CARTESIAN_POINT('Ctrl Pts',(12.5103185955646,-0.274685741688951,
4.37407134077235));
#50298=CARTESIAN_POINT('Ctrl Pts',(12.5181899676146,-0.333333232193243,
4.32290684204764));
#50299=CARTESIAN_POINT('Ctrl Pts',(12.5260613396645,-0.376326743005614,
4.26088786252735));
#50300=CARTESIAN_POINT('Ctrl Pts',(12.5339327117145,-0.419320253817985,
4.19886888300706));
#50301=CARTESIAN_POINT('Ctrl Pts',(12.5418040837645,-0.446659784938435,
4.12599542269119));
#50302=CARTESIAN_POINT('Ctrl Pts',(12.5496754558144,-0.455065168373522,
4.05100019606997));
#50303=CARTESIAN_POINT('Ctrl Pts',(12.5575468278644,-0.463470551808608,
3.97600496944875));
#50304=CARTESIAN_POINT('Ctrl Pts',(12.5654181999143,-0.452941787558331,
3.89888797652218));
#50305=CARTESIAN_POINT('Ctrl Pts',(12.5732895719643,-0.424742400952558,
3.82888990513641));
#50306=CARTESIAN_POINT('Ctrl Pts',(12.5811609440142,-0.396543014346786,
3.75889183375065));
#50307=CARTESIAN_POINT('Ctrl Pts',(12.5890323160642,-0.350673005385519,
3.69601268390568));
#50308=CARTESIAN_POINT('Ctrl Pts',(12.5969036881141,-0.292628022669152,
3.64778723809593));
#50309=CARTESIAN_POINT('Ctrl Pts',(12.6047750601641,-0.234583039952784,
3.59956179228618));
#50310=CARTESIAN_POINT('Ctrl Pts',(12.6126464322141,-0.164363083481316,
3.56599005051166));
#50311=CARTESIAN_POINT('Ctrl Pts',(12.620517804264,-0.0903829156297007,
3.55109483330951));
#50312=CARTESIAN_POINT('Ctrl Pts',(12.628389176314,-0.0164027477780855,
3.53619961610736));
#50313=CARTESIAN_POINT('Ctrl Pts',(12.6362605483639,0.0613376314536766,
3.53998092347757));
#50314=CARTESIAN_POINT('Ctrl Pts',(12.6441319204139,0.13352290298843,3.56198566164487));
#50315=CARTESIAN_POINT('Ctrl Pts',(12.6520032924638,0.205708174523184,3.58399039981218));
#50316=CARTESIAN_POINT('Ctrl Pts',(12.6598746645138,0.272338338360929,3.62421856877658));
#50317=CARTESIAN_POINT('Ctrl Pts',(12.6677460365637,0.325429113408527,3.67784968145944));
#50318=CARTESIAN_POINT('Ctrl Pts',(12.6756174086137,0.378519888456125,3.7314807941423));
#50319=CARTESIAN_POINT('Ctrl Pts',(12.6834887806637,0.418071274713577,3.79851485054363));
#50320=CARTESIAN_POINT('Ctrl Pts',(12.6913601527136,0.439343931585728,3.87091926467948));
#50321=CARTESIAN_POINT('Ctrl Pts',(12.6992315247636,0.460616588457879,3.94332367881533));
#50322=CARTESIAN_POINT('Ctrl Pts',(12.7071028968135,0.46361051594473,4.02109845068571));
#50323=CARTESIAN_POINT('Ctrl Pts',(12.7149742688635,0.447966936692366,4.09492394607626));
#50324=CARTESIAN_POINT('Ctrl Pts',(12.7228456409134,0.432323357440003,4.16874944146681));
#50325=CARTESIAN_POINT('Ctrl Pts',(12.7307170129634,0.398042271448426,4.23862566037754));
#50326=CARTESIAN_POINT('Ctrl Pts',(12.7385883850133,0.349231538304918,4.29617944234672));
#50327=CARTESIAN_POINT('Ctrl Pts',(12.7464597570633,0.300420805161409,4.35373322431589));
#50328=CARTESIAN_POINT('Ctrl Pts',(12.7543311291133,0.237080424865968,4.39896456934351));
#50329=CARTESIAN_POINT('Ctrl Pts',(12.7622025011632,0.166800374688878,4.42645347375649));
#50330=CARTESIAN_POINT('Ctrl Pts',(12.7681364312804,0.113818899065861,4.4471763206439));
#50331=CARTESIAN_POINT('Ctrl Pts',(12.7740703613976,0.056893551674301,4.45781599184163));
#50332=CARTESIAN_POINT('Ctrl Pts',(12.7800042915148,-1.13874042544416E-5,
4.45787212683272));
#50333=CARTESIAN_POINT('Origin',(12.5,0.,4.));
#50334=CARTESIAN_POINT('',(13.0800042915148,2.8196954984682E-6,4.45783894202495));
#50335=CARTESIAN_POINT('',(12.9699957084852,-6.90274666573233E-6,4.45790451736119));
#50336=CARTESIAN_POINT('',(12.5,-5.60735153159594E-17,4.457875));
#50337=CARTESIAN_POINT('Ctrl Pts',(12.9699957084852,-6.90274666573233E-6,
4.45790451736119));
#50338=CARTESIAN_POINT('Ctrl Pts',(12.9628865412726,0.0681543496286777,
4.45785453236543));
#50339=CARTESIAN_POINT('Ctrl Pts',(12.95577737406,0.136337475731944,4.44242789501186));
#50340=CARTESIAN_POINT('Ctrl Pts',(12.9486682068475,0.197807532932104,4.41298560914613));
#50341=CARTESIAN_POINT('Ctrl Pts',(12.9407968347975,0.265868063186489,4.38038668734267));
#50342=CARTESIAN_POINT('Ctrl Pts',(12.9329254627476,0.325698883531032,4.33060565060516));
#50343=CARTESIAN_POINT('Ctrl Pts',(12.9250540906976,0.370130557623211,4.26960768492436));
#50344=CARTESIAN_POINT('Ctrl Pts',(12.9171827186476,0.41456223171539,4.20860971924356));
#50345=CARTESIAN_POINT('Ctrl Pts',(12.9093113465977,0.443594759555206,4.13639482461947));
#50346=CARTESIAN_POINT('Ctrl Pts',(12.9014399745477,0.453749217534713,4.06161640217293));
#50347=CARTESIAN_POINT('Ctrl Pts',(12.8935686024978,0.463903675514219,3.9868379797264));
#50348=CARTESIAN_POINT('Ctrl Pts',(12.8856972304478,0.455180063633418,3.90949602945742));
#50349=CARTESIAN_POINT('Ctrl Pts',(12.8778258583979,0.428623718850503,3.83885831972366));
#50350=CARTESIAN_POINT('Ctrl Pts',(12.8699544863479,0.402067374067587,3.7682206099899));
#50351=CARTESIAN_POINT('Ctrl Pts',(12.862083114298,0.357678296382559,3.70428714079136));
#50352=CARTESIAN_POINT('Ctrl Pts',(12.854211742248,0.300775561959983,3.65471896268111));
#50353=CARTESIAN_POINT('Ctrl Pts',(12.846340370198,0.243872827537407,3.60515078457087));
#50354=CARTESIAN_POINT('Ctrl Pts',(12.8384689981481,0.174456436377283,3.56994789754891));
#50355=CARTESIAN_POINT('Ctrl Pts',(12.8305976260981,0.100844448250471,3.55332860992135));
#50356=CARTESIAN_POINT('Ctrl Pts',(12.8227262540482,0.0272324601236582,
3.53670932229378));
#50357=CARTESIAN_POINT('Ctrl Pts',(12.8148548819982,-0.0505751249698428,
3.53867363406062));
#50358=CARTESIAN_POINT('Ctrl Pts',(12.8069835099483,-0.123254740362562,
3.558986165072));
#50359=CARTESIAN_POINT('Ctrl Pts',(12.7991121378983,-0.195934355755281,
3.57929869608338));
#50360=CARTESIAN_POINT('Ctrl Pts',(12.7912407658484,-0.263486001447217,
3.6179594463393));
#50361=CARTESIAN_POINT('Ctrl Pts',(12.7833693937984,-0.317815070570116,
3.67033575613656));
#50362=CARTESIAN_POINT('Ctrl Pts',(12.7754980217484,-0.372144139693014,
3.72271206593382));
#50363=CARTESIAN_POINT('Ctrl Pts',(12.7676266496985,-0.413250632246875,
3.78880393527241));
#50364=CARTESIAN_POINT('Ctrl Pts',(12.7597552776485,-0.43620881068128,3.86069167744737));
#50365=CARTESIAN_POINT('Ctrl Pts',(12.7518839055986,-0.459166989115684,
3.93257941962233));
#50366=CARTESIAN_POINT('Ctrl Pts',(12.7440125335486,-0.463976853430633,
4.01026303463365));
#50367=CARTESIAN_POINT('Ctrl Pts',(12.7361411614987,-0.450062064178823,
4.08443380953254));
#50368=CARTESIAN_POINT('Ctrl Pts',(12.7282697894487,-0.436147274927012,
4.15860458443143));
#50369=CARTESIAN_POINT('Ctrl Pts',(12.7203984173988,-0.403507832108441,
4.22926251921788));
#50370=CARTESIAN_POINT('Ctrl Pts',(12.7125270453488,-0.356054829243877,
4.28794078818664));
#50371=CARTESIAN_POINT('Ctrl Pts',(12.7046556732988,-0.308601826379312,
4.3466190571554));
#50372=CARTESIAN_POINT('Ctrl Pts',(12.6967843012489,-0.246335263468753,
4.39331766030646));
#50373=CARTESIAN_POINT('Ctrl Pts',(12.6889129291989,-0.176716536654988,
4.42244075943884));
#50374=CARTESIAN_POINT('Ctrl Pts',(12.682607188961,-0.120945115332726,4.44577121528397));
#50375=CARTESIAN_POINT('Ctrl Pts',(12.6763014487231,-0.0604553842193124,
4.45782245132557));
#50376=CARTESIAN_POINT('Ctrl Pts',(12.6699957084852,1.09516003635735E-5,
4.45788309353564));
#50377=CARTESIAN_POINT('Ctrl Pts',(12.7800042915148,-1.13874042544416E-5,
4.45787212683272));
#50378=CARTESIAN_POINT('Ctrl Pts',(12.7819417334476,-0.0185909818676029,
4.45789045503738));
#50379=CARTESIAN_POINT('Ctrl Pts',(12.7838791753803,-0.0371684007279871,
4.45678053845584));
#50380=CARTESIAN_POINT('Ctrl Pts',(12.7858166173131,-0.0556056617636943,
4.45452496135198));
#50381=CARTESIAN_POINT('Ctrl Pts',(12.793687989363,-0.130511927980435,4.44536108073615));
#50382=CARTESIAN_POINT('Ctrl Pts',(12.801559361413,-0.203104740355178,4.41728685570614));
#50383=CARTESIAN_POINT('Ctrl Pts',(12.8094307334629,-0.264685413403174,
4.37366637792357));
#50384=CARTESIAN_POINT('Ctrl Pts',(12.8173021055129,-0.32626608645117,4.33004590014099));
#50385=CARTESIAN_POINT('Ctrl Pts',(12.8251734775629,-0.37683462017242,4.27087916960585));
#50386=CARTESIAN_POINT('Ctrl Pts',(12.8330448496128,-0.410331463567461,
4.20325604577686));
#50387=CARTESIAN_POINT('Ctrl Pts',(12.8409162216628,-0.443828306962503,
4.13563292194788));
#50388=CARTESIAN_POINT('Ctrl Pts',(12.8487875937127,-0.460253460031337,
4.05955340482505));
#50389=CARTESIAN_POINT('Ctrl Pts',(12.8566589657627,-0.457638721839564,
3.98413398734005));
#50390=CARTESIAN_POINT('Ctrl Pts',(12.8645303378126,-0.45502398364779,3.90871456985506));
#50391=CARTESIAN_POINT('Ctrl Pts',(12.8724017098626,-0.433369354195409,
3.8339552520079));
#50392=CARTESIAN_POINT('Ctrl Pts',(12.8802730819125,-0.395269674734573,
3.76881432927916));
#50393=CARTESIAN_POINT('Ctrl Pts',(12.8881444539625,-0.357169995273737,
3.70367340655041));
#50394=CARTESIAN_POINT('Ctrl Pts',(12.8960158260125,-0.302625265804445,
3.64815087894007));
#50395=CARTESIAN_POINT('Ctrl Pts',(12.9038871980624,-0.238171498431664,
3.6088999265713));
#50396=CARTESIAN_POINT('Ctrl Pts',(12.9117585701124,-0.173717731058884,
3.56964897420252));
#50397=CARTESIAN_POINT('Ctrl Pts',(12.9196299421623,-0.0993549257826154,
3.5466695970753));
#50398=CARTESIAN_POINT('Ctrl Pts',(12.9275013142123,-0.023993864556795,
3.54271537903906));
#50399=CARTESIAN_POINT('Ctrl Pts',(12.9353726862622,0.0513671966690251,
3.53876116100282));
#50400=CARTESIAN_POINT('Ctrl Pts',(12.9432440583122,0.127726513844396,3.55383210205756));
#50401=CARTESIAN_POINT('Ctrl Pts',(12.9511154303621,0.195934065997641,3.58612227423372));
#50402=CARTESIAN_POINT('Ctrl Pts',(12.9589868024121,0.264141618150887,3.61841244640988));
#50403=CARTESIAN_POINT('Ctrl Pts',(12.9668581744621,0.324197405282005,3.66792184970745));
#50404=CARTESIAN_POINT('Ctrl Pts',(12.974729546512,0.368905033668178,3.72871784755079));
#50405=CARTESIAN_POINT('Ctrl Pts',(12.982600918562,0.41361266205435,3.78951384539413));
#50406=CARTESIAN_POINT('Ctrl Pts',(12.9904722906119,0.442972131695578,3.86159643778324));
#50407=CARTESIAN_POINT('Ctrl Pts',(12.9983436626619,0.453465341949404,3.93632807718928));
#50408=CARTESIAN_POINT('Ctrl Pts',(13.0062150347118,0.46395855220323,4.01105971659532));
#50409=CARTESIAN_POINT('Ctrl Pts',(13.0140864067618,0.455585503069655,4.0884404030183));
#50410=CARTESIAN_POINT('Ctrl Pts',(13.0219577788117,0.429349524305901,4.15919772637108));
#50411=CARTESIAN_POINT('Ctrl Pts',(13.0298291508617,0.403113545542148,4.22995504972387));
#50412=CARTESIAN_POINT('Ctrl Pts',(13.0377005229117,0.359014637148215,4.29408901000646));
#50413=CARTESIAN_POINT('Ctrl Pts',(13.0455718949616,0.302337104315659,4.34391453219887));
#50414=CARTESIAN_POINT('Ctrl Pts',(13.0534432670116,0.245659571483104,4.39374005439127));
#50415=CARTESIAN_POINT('Ctrl Pts',(13.0613146390615,0.176403414211925,4.4292571384935));
#50416=CARTESIAN_POINT('Ctrl Pts',(13.0691860111115,0.102867492605122,4.44620982627979));
#50417=CARTESIAN_POINT('Ctrl Pts',(13.0727921045793,0.0691786509558273,
4.45397632191734));
#50418=CARTESIAN_POINT('Ctrl Pts',(13.076398198047,0.0345915681853763,4.45784650391406));
#50419=CARTESIAN_POINT('Ctrl Pts',(13.0800042915148,2.8196954984682E-6,
4.45783894202495));
#50420=CARTESIAN_POINT('Origin',(12.5,0.,4.));
#50421=CARTESIAN_POINT('',(13.3800042915148,1.00338821889499E-5,4.45789143379912));
#50422=CARTESIAN_POINT('',(13.2699957084852,-6.83105689078257E-6,4.45784477598907));
#50423=CARTESIAN_POINT('',(12.5,-5.60735153159594E-17,4.457875));
#50424=CARTESIAN_POINT('Ctrl Pts',(13.2699957084852,-6.83105689078257E-6,
4.45784477598907));
#50425=CARTESIAN_POINT('Ctrl Pts',(13.265214377922,0.0458528260712244,4.45782008288951));
#50426=CARTESIAN_POINT('Ctrl Pts',(13.2604330473589,0.091719698604501,4.45096974854549));
#50427=CARTESIAN_POINT('Ctrl Pts',(13.2556517167957,0.135506404234727,4.43740478719402));
#50428=CARTESIAN_POINT('Ctrl Pts',(13.2477803447458,0.207591244700251,4.41507316710824));
#50429=CARTESIAN_POINT('Ctrl Pts',(13.2399089726958,0.274038390871736,4.37454348113122));
#50430=CARTESIAN_POINT('Ctrl Pts',(13.2320376006459,0.326885582178656,4.32067233995558));
#50431=CARTESIAN_POINT('Ctrl Pts',(13.2241662285959,0.379732773485576,4.26680119877995));
#50432=CARTESIAN_POINT('Ctrl Pts',(13.2162948565459,0.418980009927931,4.19958860240569));
#50433=CARTESIAN_POINT('Ctrl Pts',(13.208423484496,0.439924354792367,4.12708853413817));
#50434=CARTESIAN_POINT('Ctrl Pts',(13.200552112446,0.460868699656804,4.05458846587065));
#50435=CARTESIAN_POINT('Ctrl Pts',(13.1926807403961,0.463510152943321,3.97680092570987));
#50436=CARTESIAN_POINT('Ctrl Pts',(13.1848093683461,0.447532193317848,3.90304707640827));
#50437=CARTESIAN_POINT('Ctrl Pts',(13.1769379962962,0.431554233692375,3.82929322710668));
#50438=CARTESIAN_POINT('Ctrl Pts',(13.1690666242462,0.396956861154912,3.75957306866428));
#50439=CARTESIAN_POINT('Ctrl Pts',(13.1611952521963,0.347885826291745,3.70224106173923));
#50440=CARTESIAN_POINT('Ctrl Pts',(13.1533238801463,0.298814791428577,3.64490905481418));
#50441=CARTESIAN_POINT('Ctrl Pts',(13.1454525080963,0.235270094239705,3.59996519940648));
#50442=CARTESIAN_POINT('Ctrl Pts',(13.1375811360464,0.164866199243897,3.57279504942506));
#50443=CARTESIAN_POINT('Ctrl Pts',(13.1297097639964,0.0944623042480882,
3.54562489944363));
#50444=CARTESIAN_POINT('Ctrl Pts',(13.1218383919465,0.0171992114453437,
3.53622845488849));
#50445=CARTESIAN_POINT('Ctrl Pts',(13.1139670198965,-0.0576647601420857,
3.54573167743434));
#50446=CARTESIAN_POINT('Ctrl Pts',(13.1060956478466,-0.132528731729515,
3.55523489998019));
#50447=CARTESIAN_POINT('Ctrl Pts',(13.0982242757966,-0.204993582101629,
3.58363778962703));
#50448=CARTESIAN_POINT('Ctrl Pts',(13.0903529037467,-0.266375958336211,
3.62753687126191));
#50449=CARTESIAN_POINT('Ctrl Pts',(13.0824815316967,-0.327758334570793,
3.67143595289679));
#50450=CARTESIAN_POINT('Ctrl Pts',(13.0746101596467,-0.378058236667844,
3.73083122651971));
#50451=CARTESIAN_POINT('Ctrl Pts',(13.0667387875968,-0.411248303781717,
3.79860544673343));
#50452=CARTESIAN_POINT('Ctrl Pts',(13.0588674155468,-0.444438370895591,
3.86637966694714));
#50453=CARTESIAN_POINT('Ctrl Pts',(13.0509960434969,-0.460518603026287,
3.94253283375165));
#50454=CARTESIAN_POINT('Ctrl Pts',(13.0431246714469,-0.457562130387816,
4.0179396288708));
#50455=CARTESIAN_POINT('Ctrl Pts',(13.035253299397,-0.454605657749345,4.09334642398995));
#50456=CARTESIAN_POINT('Ctrl Pts',(13.027381927347,-0.432612480341706,4.16800684742375));
#50457=CARTESIAN_POINT('Ctrl Pts',(13.0195105552971,-0.394218007200806,
4.23297445406563));
#50458=CARTESIAN_POINT('Ctrl Pts',(13.0116391832471,-0.355823534059905,
4.29794206070751));
#50459=CARTESIAN_POINT('Ctrl Pts',(13.0037678111972,-0.301027765185743,
4.35321685055749));
#50460=CARTESIAN_POINT('Ctrl Pts',(12.9958964391472,-0.236396794305188,
4.39217532952931));
#50461=CARTESIAN_POINT('Ctrl Pts',(12.9880250670972,-0.171765823424632,
4.43113380850113));
#50462=CARTESIAN_POINT('Ctrl Pts',(12.9801536950473,-0.0972996505376846,
4.45377597659478));
#50463=CARTESIAN_POINT('Ctrl Pts',(12.9722823229973,-0.0219214440120968,
4.4573886572069));
#50464=CARTESIAN_POINT('Ctrl Pts',(12.9715201181599,-0.014622381881285,
4.45773848219561));
#50465=CARTESIAN_POINT('Ctrl Pts',(12.9707579133226,-0.00731476803234869,
4.45790987647069));
#50466=CARTESIAN_POINT('Ctrl Pts',(12.9699957084852,-6.90274666573233E-6,
4.45790451736119));
#50467=CARTESIAN_POINT('Ctrl Pts',(13.0800042915148,2.8196954984682E-6,
4.45783894202495));
#50468=CARTESIAN_POINT('Ctrl Pts',(13.084269570097,-0.0409086678841046,
4.4578299978409));
#50469=CARTESIAN_POINT('Ctrl Pts',(13.0885348486792,-0.0818224858219862,
4.45239605085009));
#50470=CARTESIAN_POINT('Ctrl Pts',(13.0928001272613,-0.121255029803553,
4.44156782927524));
#50471=CARTESIAN_POINT('Ctrl Pts',(13.1006714993113,-0.194025944662995,
4.42158485301405));
#50472=CARTESIAN_POINT('Ctrl Pts',(13.1085428713613,-0.261752088439453,
4.3832306090213));
#50473=CARTESIAN_POINT('Ctrl Pts',(13.1164142434112,-0.31631794022257,4.33110102808186));
#50474=CARTESIAN_POINT('Ctrl Pts',(13.1242856154612,-0.370883792005687,
4.27897144714243));
#50475=CARTESIAN_POINT('Ctrl Pts',(13.1321569875111,-0.412289351795463,
4.21306652925631));
#50476=CARTESIAN_POINT('Ctrl Pts',(13.1400283595611,-0.435573054271055,
4.14128356060242));
#50477=CARTESIAN_POINT('Ctrl Pts',(13.147899731611,-0.458856756746647,4.06950059194853));
#50478=CARTESIAN_POINT('Ctrl Pts',(13.155771103661,-0.464018601908056,3.99183957252686));
#50479=CARTESIAN_POINT('Ctrl Pts',(13.1636424757109,-0.45044005369213,3.91760650430194));
#50480=CARTESIAN_POINT('Ctrl Pts',(13.1715138477609,-0.436861505476204,
3.84337343607703));
#50481=CARTESIAN_POINT('Ctrl Pts',(13.1793852198109,-0.404542563882944,
3.77256831904885));
#50482=CARTESIAN_POINT('Ctrl Pts',(13.1872565918608,-0.357355958580309,
3.7136756228145));
#50483=CARTESIAN_POINT('Ctrl Pts',(13.1951279639108,-0.310169353277673,
3.65478292658016));
#50484=CARTESIAN_POINT('Ctrl Pts',(13.2029993359607,-0.248115084265664,
3.60780265113964));
#50485=CARTESIAN_POINT('Ctrl Pts',(13.2108707080107,-0.178629020319019,
3.57836437152041));
#50486=CARTESIAN_POINT('Ctrl Pts',(13.2187420800606,-0.109142956372374,
3.54892609190117));
#50487=CARTESIAN_POINT('Ctrl Pts',(13.2266134521106,-0.0322250974910928,
3.53702980810322));
#50488=CARTESIAN_POINT('Ctrl Pts',(13.2344848241605,0.0429076061587562,
3.54410103373967));
#50489=CARTESIAN_POINT('Ctrl Pts',(13.2423561962105,0.118040309808605,3.55117225937612));
#50490=CARTESIAN_POINT('Ctrl Pts',(13.2502275682605,0.191387858227023,3.57721099444696));
#50491=CARTESIAN_POINT('Ctrl Pts',(13.2580989403104,0.254161126126225,3.61909705689013));
#50492=CARTESIAN_POINT('Ctrl Pts',(13.2659703123604,0.316934394025428,3.66098311933329));
#50493=CARTESIAN_POINT('Ctrl Pts',(13.2738416844103,0.369133381405416,3.71871650914877));
#50494=CARTESIAN_POINT('Ctrl Pts',(13.2817130564603,0.404503162915977,3.78537912195109));
#50495=CARTESIAN_POINT('Ctrl Pts',(13.2895844285102,0.43987294442654,3.85204173475342));
#50496=CARTESIAN_POINT('Ctrl Pts',(13.2974558005602,0.458413520067676,3.92763357054259));
#50497=CARTESIAN_POINT('Ctrl Pts',(13.3053271726101,0.457903200829578,4.00309657448501));
#50498=CARTESIAN_POINT('Ctrl Pts',(13.3131985446601,0.457392881591479,4.07855957842742));
#50499=CARTESIAN_POINT('Ctrl Pts',(13.3210699167101,0.437831667474148,4.15389375052308));
#50500=CARTESIAN_POINT('Ctrl Pts',(13.32894128876,0.401563549045306,4.22007191138728));
#50501=CARTESIAN_POINT('Ctrl Pts',(13.33681266081,0.365295430616463,4.28625007225149));
#50502=CARTESIAN_POINT('Ctrl Pts',(13.3446840328599,0.31232040787611,4.34327222188425));
#50503=CARTESIAN_POINT('Ctrl Pts',(13.3525554049099,0.248986397312635,4.38430548273058));
#50504=CARTESIAN_POINT('Ctrl Pts',(13.3604267769598,0.185652386749161,4.42533874357692));
#50505=CARTESIAN_POINT('Ctrl Pts',(13.3682981490098,0.111959388362564,4.45038311563682));
#50506=CARTESIAN_POINT('Ctrl Pts',(13.3761695210597,0.0367379221854645,
4.45643756985705));
#50507=CARTESIAN_POINT('Ctrl Pts',(13.3774477778781,0.024522472144774,4.45742077168506));
#50508=CARTESIAN_POINT('Ctrl Pts',(13.3787260346965,0.0122667140672706,
4.45790318029249));
#50509=CARTESIAN_POINT('Ctrl Pts',(13.3800042915148,1.00338821889499E-5,
4.45789143379912));
#50510=CARTESIAN_POINT('Origin',(12.5,0.,4.));
#50511=CARTESIAN_POINT('',(13.6800042915148,-8.85210990424201E-6,4.45789764648838));
#50512=CARTESIAN_POINT('',(13.5699957084852,1.03170790782398E-5,4.4578580083501));
#50513=CARTESIAN_POINT('',(12.5,-5.60735153159594E-17,4.457875));
#50514=CARTESIAN_POINT('Ctrl Pts',(13.5699957084852,1.03170790782398E-5,
4.4578580083501));
#50515=CARTESIAN_POINT('Ctrl Pts',(13.5675422145714,0.0235408097699949,
4.45787795556699));
#50516=CARTESIAN_POINT('Ctrl Pts',(13.5650887206577,0.0470683081483061,
4.45609516914004));
#50517=CARTESIAN_POINT('Ctrl Pts',(13.562635226744,0.0703115975725277,4.45248338388903));
#50518=CARTESIAN_POINT('Ctrl Pts',(13.554763854694,0.144881409096958,4.44089594716616));
#50519=CARTESIAN_POINT('Ctrl Pts',(13.5468924826441,0.21652593236894,4.41048310506186));
#50520=CARTESIAN_POINT('Ctrl Pts',(13.5390211105941,0.276660113016528,4.36488918223832));
#50521=CARTESIAN_POINT('Ctrl Pts',(13.5311497385442,0.336794293664116,4.31929525941478));
#50522=CARTESIAN_POINT('Ctrl Pts',(13.5232783664942,0.385418131687311,4.25852025587201));
#50523=CARTESIAN_POINT('Ctrl Pts',(13.5154069944443,0.416705106451492,4.18984674794718));
#50524=CARTESIAN_POINT('Ctrl Pts',(13.5075356223943,0.447992081215673,4.12117324002235));
#50525=CARTESIAN_POINT('Ctrl Pts',(13.4996642503443,0.461942192720839,4.04460122771548));
#50526=CARTESIAN_POINT('Ctrl Pts',(13.4917928782944,0.456883820300162,3.96930621892307));
#50527=CARTESIAN_POINT('Ctrl Pts',(13.4839215062444,0.451825447879485,3.89401121013066));
#50528=CARTESIAN_POINT('Ctrl Pts',(13.4760501341945,0.427758591532965,3.81999320485271));
#50529=CARTESIAN_POINT('Ctrl Pts',(13.4681787621445,0.387567146091087,3.75612166820384));
#50530=CARTESIAN_POINT('Ctrl Pts',(13.4603073900946,0.347375700649209,3.69225013155497));
#50531=CARTESIAN_POINT('Ctrl Pts',(13.4524360180446,0.291059666111973,3.63852506353517));
#50532=CARTESIAN_POINT('Ctrl Pts',(13.4445646459947,0.225367307335285,3.60138425741911));
#50533=CARTESIAN_POINT('Ctrl Pts',(13.4366932739447,0.159674948558598,3.56424345130305));
#50534=CARTESIAN_POINT('Ctrl Pts',(13.4288219018947,0.0846062655424597,
3.54368690709073));
#50535=CARTESIAN_POINT('Ctrl Pts',(13.4209505298448,0.00915662451852634,
3.54217788424291));
#50536=CARTESIAN_POINT('Ctrl Pts',(13.4130791577948,-0.0662930165054059,
3.54066886139509));
#50537=CARTESIAN_POINT('Ctrl Pts',(13.4052077857449,-0.142123615537132,
3.55820735991178));
#50538=CARTESIAN_POINT('Ctrl Pts',(13.3973364136949,-0.209248507106454,
3.5926917681625));
#50539=CARTESIAN_POINT('Ctrl Pts',(13.389465041645,-0.276373398675776,3.62717617641322));
#50540=CARTESIAN_POINT('Ctrl Pts',(13.381593669595,-0.334792582782693,3.67860649439798));
#50541=CARTESIAN_POINT('Ctrl Pts',(13.3737222975451,-0.377505777353741,
3.74081990525232));
#50542=CARTESIAN_POINT('Ctrl Pts',(13.3658509254951,-0.420218971924789,
3.80303331610666));
#50543=CARTESIAN_POINT('Ctrl Pts',(13.3579795534451,-0.44722617695997,3.87602981983059));
#50544=CARTESIAN_POINT('Ctrl Pts',(13.3501081813952,-0.455291160112798,
3.95106235628872));
#50545=CARTESIAN_POINT('Ctrl Pts',(13.3422368093452,-0.463356143265626,
4.02609489274685));
#50546=CARTESIAN_POINT('Ctrl Pts',(13.3343654372953,-0.452478904536101,
4.10316346193917));
#50547=CARTESIAN_POINT('Ctrl Pts',(13.3264940652453,-0.423962846915058,
4.17303305431203));
#50548=CARTESIAN_POINT('Ctrl Pts',(13.3186226931954,-0.395446789294015,
4.24290264668488));
#50549=CARTESIAN_POINT('Ctrl Pts',(13.3107513211454,-0.349291912781453,
4.30557326223827));
#50550=CARTESIAN_POINT('Ctrl Pts',(13.3028799490955,-0.291028886105345,
4.35353517632783));
#50551=CARTESIAN_POINT('Ctrl Pts',(13.2950085770455,-0.232765859429236,
4.4014970904174));
#50552=CARTESIAN_POINT('Ctrl Pts',(13.2871372049956,-0.162394682589579,
4.43475030304313));
#50553=CARTESIAN_POINT('Ctrl Pts',(13.2792658329456,-0.0883478267899694,
4.44931013225873));
#50554=CARTESIAN_POINT('Ctrl Pts',(13.2761757914588,-0.059279469337623,
4.4550258417985));
#50555=CARTESIAN_POINT('Ctrl Pts',(13.273085749972,-0.0296446570187532,
4.45786073445524));
#50556=CARTESIAN_POINT('Ctrl Pts',(13.2699957084852,-6.83105689078257E-6,
4.45784477598907));
#50557=CARTESIAN_POINT('Ctrl Pts',(13.3800042915148,1.00338821889499E-5,
4.45789143379912));
#50558=CARTESIAN_POINT('Ctrl Pts',(13.3865974067464,-0.0632086430349686,
4.45783084661254));
#50559=CARTESIAN_POINT('Ctrl Pts',(13.393190521978,-0.12645185159805,4.44462381290384));
#50560=CARTESIAN_POINT('Ctrl Pts',(13.3997836372096,-0.184315051738561,
4.41918121595096));
#50561=CARTESIAN_POINT('Ctrl Pts',(13.4076550092596,-0.253396625517876,
4.3888058714441));
#50562=CARTESIAN_POINT('Ctrl Pts',(13.4155263813095,-0.314809839108902,
4.34099064604983));
#50563=CARTESIAN_POINT('Ctrl Pts',(13.4233977533595,-0.361195640434018,
4.28146516557999));
#50564=CARTESIAN_POINT('Ctrl Pts',(13.4312691254094,-0.407581441759134,
4.22193968511016));
#50565=CARTESIAN_POINT('Ctrl Pts',(13.4391404974594,-0.438939830818339,
4.15070394956476));
#50566=CARTESIAN_POINT('Ctrl Pts',(13.4470118695093,-0.451513179494438,
4.07629402890356));
#50567=CARTESIAN_POINT('Ctrl Pts',(13.4548832415593,-0.464086528170537,
4.00188410824235));
#50568=CARTESIAN_POINT('Ctrl Pts',(13.4627546136093,-0.457874836463529,
3.92430000246534));
#50569=CARTESIAN_POINT('Ctrl Pts',(13.4706259856592,-0.433622441953051,
3.85283849709185));
#50570=CARTESIAN_POINT('Ctrl Pts',(13.4784973577092,-0.409370047442573,
3.78137699171835));
#50571=CARTESIAN_POINT('Ctrl Pts',(13.4863687297591,-0.367076950128625,
3.71603808674838));
#50572=CARTESIAN_POINT('Ctrl Pts',(13.4942401018091,-0.311811067605128,
3.66465124389307));
#50573=CARTESIAN_POINT('Ctrl Pts',(13.502111473859,-0.25654518508163,3.61326440103776));
#50574=CARTESIAN_POINT('Ctrl Pts',(13.509982845909,-0.188306517348584,3.5758296202971));
#50575=CARTESIAN_POINT('Ctrl Pts',(13.5178542179589,-0.115272000283325,
3.55683265457144));
#50576=CARTESIAN_POINT('Ctrl Pts',(13.5257255900089,-0.0422374832180674,
3.53783568884578));
#50577=CARTESIAN_POINT('Ctrl Pts',(13.5335969620589,0.035592883179403,3.53727653813511));
#50578=CARTESIAN_POINT('Ctrl Pts',(13.5414683341088,0.108892804353757,3.55522220461956));
#50579=CARTESIAN_POINT('Ctrl Pts',(13.5493397061588,0.182192725528112,3.573167871104));
#50580=CARTESIAN_POINT('Ctrl Pts',(13.5572110782087,0.250962201479351,3.60961835478357));
#50581=CARTESIAN_POINT('Ctrl Pts',(13.5650824502587,0.306960690387823,3.66020584957927));
#50582=CARTESIAN_POINT('Ctrl Pts',(13.5729538223086,0.362959179296295,3.71079334437498));
#50583=CARTESIAN_POINT('Ctrl Pts',(13.5808251943586,0.406186681162,3.77551785028682));
#50584=CARTESIAN_POINT('Ctrl Pts',(13.5886965664085,0.431463310113251,3.84662352810933));
#50585=CARTESIAN_POINT('Ctrl Pts',(13.5965679384585,0.456739939064502,3.91772920593184));
#50586=CARTESIAN_POINT('Ctrl Pts',(13.6044393105085,0.464065695101298,3.99521605566501));
#50587=CARTESIAN_POINT('Ctrl Pts',(13.6123106825584,0.452562744007997,4.06979894583348));
#50588=CARTESIAN_POINT('Ctrl Pts',(13.6201820546084,0.441059792914696,4.14438183600196));
#50589=CARTESIAN_POINT('Ctrl Pts',(13.6280534266583,0.410728134691299,4.21606076660573));
#50590=CARTESIAN_POINT('Ctrl Pts',(13.6359247987083,0.365202365858889,4.27624656029457));
#50591=CARTESIAN_POINT('Ctrl Pts',(13.6437961707582,0.319676597026479,4.33643235398341));
#50592=CARTESIAN_POINT('Ctrl Pts',(13.6516675428082,0.258956717585058,4.38512501075732));
#50593=CARTESIAN_POINT('Ctrl Pts',(13.6595389148581,0.190318698434502,4.41648976353532));
#50594=CARTESIAN_POINT('Ctrl Pts',(13.666360707077,0.130832969391341,4.44367229602021));
#50595=CARTESIAN_POINT('Ctrl Pts',(13.6731824992959,0.065399948454096,4.45783988979956));
#50596=CARTESIAN_POINT('Ctrl Pts',(13.6800042915148,-8.85210990424201E-6,
4.45789764648838));
#50597=CARTESIAN_POINT('Origin',(12.5,0.,4.));
#50598=CARTESIAN_POINT('',(13.9800042915148,-4.68615130337092E-6,4.45784092071359));
#50599=CARTESIAN_POINT('',(13.8699957084852,1.23414887176878E-6,4.4579133809027));
#50600=CARTESIAN_POINT('',(12.5,-5.60735153159594E-17,4.457875));
#50601=CARTESIAN_POINT('Ctrl Pts',(13.8699957084852,1.23414887176878E-6,
4.4579133809027));
#50602=CARTESIAN_POINT('Ctrl Pts',(13.8698700512209,0.00120594270822336,
4.45791357044259));
#50603=CARTESIAN_POINT('Ctrl Pts',(13.8697443939566,0.00241064979645091,
4.45790891401425));
#50604=CARTESIAN_POINT('Ctrl Pts',(13.8696187366923,0.00361531855258033,
4.45789940262096));
#50605=CARTESIAN_POINT('Ctrl Pts',(13.8617473646423,0.0790776965455978,
4.45730359373015));
#50606=CARTESIAN_POINT('Ctrl Pts',(13.8538759925924,0.154389660535011,4.43765704798318));
#50607=CARTESIAN_POINT('Ctrl Pts',(13.8460046205424,0.22052669229976,4.40131398110731));
#50608=CARTESIAN_POINT('Ctrl Pts',(13.8381332484924,0.286663724064511,4.36497091423144));
#50609=CARTESIAN_POINT('Ctrl Pts',(13.8302618764425,0.343625823604597,4.31193132622667));
#50610=CARTESIAN_POINT('Ctrl Pts',(13.8223905043925,0.384587309076409,4.24855087033892));
#50611=CARTESIAN_POINT('Ctrl Pts',(13.8145191323426,0.42554879454822,4.18517041445118));
#50612=CARTESIAN_POINT('Ctrl Pts',(13.8066477602926,0.450509665951756,4.11144909068046));
#50613=CARTESIAN_POINT('Ctrl Pts',(13.7987763882427,0.456478899990553,4.03622081324714));
#50614=CARTESIAN_POINT('Ctrl Pts',(13.7909050161927,0.46244813402935,3.96099253581381));
#50615=CARTESIAN_POINT('Ctrl Pts',(13.7830336441427,0.449425730703409,3.88425730471787));
#50616=CARTESIAN_POINT('Ctrl Pts',(13.7751622720928,0.418972144817937,3.81521018611534));
#50617=CARTESIAN_POINT('Ctrl Pts',(13.7672909000428,0.388518558932466,3.74616306751281));
#50618=CARTESIAN_POINT('Ctrl Pts',(13.7594195279929,0.340633790487464,3.68480406140369));
#50619=CARTESIAN_POINT('Ctrl Pts',(13.7515481559429,0.281055798532888,3.6384857242654));
#50620=CARTESIAN_POINT('Ctrl Pts',(13.743676783893,0.221477806578313,3.59216738712712));
#50621=CARTESIAN_POINT('Ctrl Pts',(13.735805411843,0.150206591114165,3.56088971895966));
#50622=CARTESIAN_POINT('Ctrl Pts',(13.7279340397931,0.0757824736049535,
3.54840067521841));
#50623=CARTESIAN_POINT('Ctrl Pts',(13.7200626677431,0.00135835609574232,
3.53591163147717));
#50624=CARTESIAN_POINT('Ctrl Pts',(13.7121912956931,-0.0762186634585312,
3.54221121216214));
#50625=CARTESIAN_POINT('Ctrl Pts',(13.7043199236432,-0.14765264866984,3.56654454809098));
#50626=CARTESIAN_POINT('Ctrl Pts',(13.6964485515932,-0.219086633881149,
3.59087788401983));
#50627=CARTESIAN_POINT('Ctrl Pts',(13.6885771795433,-0.284377584749494,
3.63324497519255));
#50628=CARTESIAN_POINT('Ctrl Pts',(13.6807058074933,-0.335701785830877,
3.68856903744356));
#50629=CARTESIAN_POINT('Ctrl Pts',(13.6728344354434,-0.38702598691226,3.74389309969457));
#50630=CARTESIAN_POINT('Ctrl Pts',(13.6649630633934,-0.424383438206683,
3.81217413302386));
#50631=CARTESIAN_POINT('Ctrl Pts',(13.6570916913435,-0.443297653083863,
3.88523012494906));
#50632=CARTESIAN_POINT('Ctrl Pts',(13.6492203192935,-0.462211867961044,
3.95828611687427));
#50633=CARTESIAN_POINT('Ctrl Pts',(13.6413489472436,-0.462682846420982,
4.03611706739538));
#50634=CARTESIAN_POINT('Ctrl Pts',(13.6334775751936,-0.444654151830396,
4.10939661196244));
#50635=CARTESIAN_POINT('Ctrl Pts',(13.6256062031436,-0.42662545723981,4.18267615652949));
#50636=CARTESIAN_POINT('Ctrl Pts',(13.6177348310937,-0.3900970895987,4.25140429514248));
#50637=CARTESIAN_POINT('Ctrl Pts',(13.6098634590437,-0.339446187702822,
4.3073454393722));
#50638=CARTESIAN_POINT('Ctrl Pts',(13.6019920869938,-0.288795285806945,
4.36328658360191));
#50639=CARTESIAN_POINT('Ctrl Pts',(13.5941207149438,-0.224021849656302,
4.40644073344835));
#50640=CARTESIAN_POINT('Ctrl Pts',(13.5862493428939,-0.152887581692542,
4.43163679270085));
#50641=CARTESIAN_POINT('Ctrl Pts',(13.5808314647576,-0.103925749791867,
4.44897928111035));
#50642=CARTESIAN_POINT('Ctrl Pts',(13.5754135866214,-0.0519504158054226,
4.45781396031326));
#50643=CARTESIAN_POINT('Ctrl Pts',(13.5699957084852,1.03170790782398E-5,
4.4578580083501));
#50644=CARTESIAN_POINT('Ctrl Pts',(13.6800042915148,-8.85210990424201E-6,
4.45789764648838));
#50645=CARTESIAN_POINT('Ctrl Pts',(13.6810538713459,-0.010072447664127,
4.45790653275371));
#50646=CARTESIAN_POINT('Ctrl Pts',(13.6821034511769,-0.0201354698749596,
4.45758141170421));
#50647=CARTESIAN_POINT('Ctrl Pts',(13.683153031008,-0.0301761699425476,
4.45691829561871));
#50648=CARTESIAN_POINT('Ctrl Pts',(13.691024403058,-0.105476860309351,4.45194522614199));
#50649=CARTESIAN_POINT('Ctrl Pts',(13.6988957751079,-0.179522082183268,
4.42796223840642));
#50650=CARTESIAN_POINT('Ctrl Pts',(13.7067671471579,-0.24343910912634,4.38784317739428));
#50651=CARTESIAN_POINT('Ctrl Pts',(13.7146385192078,-0.307356136069411,
4.34772411638213));
#50652=CARTESIAN_POINT('Ctrl Pts',(13.7225098912578,-0.361144968081636,
4.2914689820934));
#50653=CARTESIAN_POINT('Ctrl Pts',(13.7303812633077,-0.398360171146024,
4.22581874179975));
#50654=CARTESIAN_POINT('Ctrl Pts',(13.7382526353577,-0.435575374210412,
4.1601685015061));
#50655=CARTESIAN_POINT('Ctrl Pts',(13.7461240074077,-0.456216948326962,
4.08512315520753));
#50656=CARTESIAN_POINT('Ctrl Pts',(13.7539953794576,-0.457811445030669,
4.00967527273228));
#50657=CARTESIAN_POINT('Ctrl Pts',(13.7618667515076,-0.459405941734377,
3.93422739025703));
#50658=CARTESIAN_POINT('Ctrl Pts',(13.7697381235575,-0.441953361025241,
3.85837697160509));
#50659=CARTESIAN_POINT('Ctrl Pts',(13.7776094956075,-0.407545019133394,
3.79121305720166));
#50660=CARTESIAN_POINT('Ctrl Pts',(13.7854808676574,-0.373136677241547,
3.72404914279823));
#50661=CARTESIAN_POINT('Ctrl Pts',(13.7933522397074,-0.321772574166988,
3.6655717326433));
#50662=CARTESIAN_POINT('Ctrl Pts',(13.8012236117573,-0.259607592342073,
3.6227880859492));
#50663=CARTESIAN_POINT('Ctrl Pts',(13.8090949838073,-0.19744261051716,3.5800044392551));
#50664=CARTESIAN_POINT('Ctrl Pts',(13.8169663558573,-0.124476749941891,
3.55291455602183));
#50665=CARTESIAN_POINT('Ctrl Pts',(13.8248377279072,-0.0494533988297167,
3.54476457579874));
#50666=CARTESIAN_POINT('Ctrl Pts',(13.8327090999572,0.0255699522824598,
3.53661459557564));
#50667=CARTESIAN_POINT('Ctrl Pts',(13.8405804720071,0.102650793931542,3.54740451836272));
#50668=CARTESIAN_POINT('Ctrl Pts',(13.8484518440571,0.172552645974024,3.57584140410587));
#50669=CARTESIAN_POINT('Ctrl Pts',(13.856323216107,0.242454498016503,3.60427828984902));
#50670=CARTESIAN_POINT('Ctrl Pts',(13.864194588157,0.305177360452382,3.65036213854823));
#50671=CARTESIAN_POINT('Ctrl Pts',(13.8720659602069,0.353205247972751,3.70857079263049));
#50672=CARTESIAN_POINT('Ctrl Pts',(13.8799373322569,0.40123313549312,3.76677944671275));
#50673=CARTESIAN_POINT('Ctrl Pts',(13.8878087043068,0.434566048097978,3.83711290617806));
#50674=CARTESIAN_POINT('Ctrl Pts',(13.8956800763568,0.44920975351361,3.9111432194385));
#50675=CARTESIAN_POINT('Ctrl Pts',(13.9035514484068,0.463853458929242,3.98517353269893));
#50676=CARTESIAN_POINT('Ctrl Pts',(13.9114228204567,0.459807957155645,4.06290069975448));
#50677=CARTESIAN_POINT('Ctrl Pts',(13.9192941925067,0.437558014523894,4.13501079227018));
#50678=CARTESIAN_POINT('Ctrl Pts',(13.9271655645566,0.415308071892144,4.20712088478587));
#50679=CARTESIAN_POINT('Ctrl Pts',(13.9350369366066,0.374853688402242,4.27361390276169));
#50680=CARTESIAN_POINT('Ctrl Pts',(13.9429083086565,0.321042451364188,4.32652208887851));
#50681=CARTESIAN_POINT('Ctrl Pts',(13.9507796807065,0.267231214326134,4.37943027499533));
#50682=CARTESIAN_POINT('Ctrl Pts',(13.9586510527564,0.200063123739928,4.41875362925314));
#50683=CARTESIAN_POINT('Ctrl Pts',(13.9665224248064,0.127586829849962,4.43978009385641));
#50684=CARTESIAN_POINT('Ctrl Pts',(13.9710163803759,0.086208370984788,4.45178460807712));
#50685=CARTESIAN_POINT('Ctrl Pts',(13.9755103359454,0.0430996806131821,
4.45782517307841));
#50686=CARTESIAN_POINT('Ctrl Pts',(13.9800042915148,-4.68615130337092E-6,
4.45784092071359));
#50687=CARTESIAN_POINT('Origin',(12.5,0.,4.));
#50688=CARTESIAN_POINT('',(14.2800042915148,1.11332528513013E-5,4.45786561359635));
#50689=CARTESIAN_POINT('',(14.1699957084852,-1.10604184835328E-5,4.4578646218584));
#50690=CARTESIAN_POINT('',(12.5,-5.60735153159594E-17,4.457875));
#50691=CARTESIAN_POINT('Ctrl Pts',(14.1699957084852,-1.10604184835328E-5,
4.4578646218584));
#50692=CARTESIAN_POINT('Ctrl Pts',(14.1643265158203,0.0543576752587709,
4.45781404039958));
#50693=CARTESIAN_POINT('Ctrl Pts',(14.1586573231555,0.108743966382031,4.44812254260427));
#50694=CARTESIAN_POINT('Ctrl Pts',(14.1529881304907,0.159684023833442,4.42916890146099));
#50695=CARTESIAN_POINT('Ctrl Pts',(14.1451167584407,0.230411580321883,4.40285278028461));
#50696=CARTESIAN_POINT('Ctrl Pts',(14.1372453863907,0.294495541512382,4.358681244225));
#50697=CARTESIAN_POINT('Ctrl Pts',(14.1293740143408,0.344256823700223,4.30194730133701));
#50698=CARTESIAN_POINT('Ctrl Pts',(14.1215026422908,0.394018105888063,4.24521335844902));
#50699=CARTESIAN_POINT('Ctrl Pts',(14.1136312702409,0.429456709073245,4.17591700873265));
#50700=CARTESIAN_POINT('Ctrl Pts',(14.1057598981909,0.446326079279053,4.10236192849032));
#50701=CARTESIAN_POINT('Ctrl Pts',(14.097888526141,0.46319544948486,4.02880684824799));
#50702=CARTESIAN_POINT('Ctrl Pts',(14.090017154091,0.461495586711293,3.95099303747972));
#50703=CARTESIAN_POINT('Ctrl Pts',(14.0821457820411,0.441430182931853,3.87824480690492));
#50704=CARTESIAN_POINT('Ctrl Pts',(14.0742744099911,0.421364779152413,3.80549657633012));
#50705=CARTESIAN_POINT('Ctrl Pts',(14.0664030379411,0.3829338343671,3.73781392594881));
#50706=CARTESIAN_POINT('Ctrl Pts',(14.0585316658912,0.330742470300218,3.68330716492384));
#50707=CARTESIAN_POINT('Ctrl Pts',(14.0506602938412,0.278551106233337,3.62880040389886));
#50708=CARTESIAN_POINT('Ctrl Pts',(14.0427889217913,0.212599322884887,3.58746953223022));
#50709=CARTESIAN_POINT('Ctrl Pts',(14.0349175497413,0.140790022250932,3.5642671654747));
#50710=CARTESIAN_POINT('Ctrl Pts',(14.0270461776914,0.0689807216169763,
3.54106479871918));
#50711=CARTESIAN_POINT('Ctrl Pts',(14.0191748056414,-0.00868609630248519,
3.53599093687678));
#50712=CARTESIAN_POINT('Ctrl Pts',(14.0113034335915,-0.0829037347177578,
3.5496535731032));
#50713=CARTESIAN_POINT('Ctrl Pts',(14.0034320615415,-0.15712137313303,3.56331620932962));
#50714=CARTESIAN_POINT('Ctrl Pts',(13.9955606894916,-0.227889832044114,
3.59571534362485));
#50715=CARTESIAN_POINT('Ctrl Pts',(13.9876893174416,-0.286729034540398,
3.64296863695132));
#50716=CARTESIAN_POINT('Ctrl Pts',(13.9798179453916,-0.345568237036683,
3.69022193027778));
#50717=CARTESIAN_POINT('Ctrl Pts',(13.9719465733417,-0.392478183118168,
3.75232938263547));
#50718=CARTESIAN_POINT('Ctrl Pts',(13.9640752012917,-0.421837725217638,
3.82184875237013));
#50719=CARTESIAN_POINT('Ctrl Pts',(13.9562038292418,-0.451197267317109,
3.8913681221048));
#50720=CARTESIAN_POINT('Ctrl Pts',(13.9483324571918,-0.463006405434566,
3.96829940921644));
#50721=CARTESIAN_POINT('Ctrl Pts',(13.9404610851419,-0.455850068491383,
4.04342405445454));
#50722=CARTESIAN_POINT('Ctrl Pts',(13.9325897130919,-0.448693731548199,
4.11854869969265));
#50723=CARTESIAN_POINT('Ctrl Pts',(13.924718341042,-0.422571919544373,4.19186670305722));
#50724=CARTESIAN_POINT('Ctrl Pts',(13.916846968992,-0.38061476952465,4.25459247959939));
#50725=CARTESIAN_POINT('Ctrl Pts',(13.908975596942,-0.338657619504927,4.31731825614156));
#50726=CARTESIAN_POINT('Ctrl Pts',(13.9011042248921,-0.280865131469307,
4.36945180586132));
#50727=CARTESIAN_POINT('Ctrl Pts',(13.8932328528421,-0.214162491453186,
4.40474604470388));
#50728=CARTESIAN_POINT('Ctrl Pts',(13.8854871380565,-0.148524681204106,
4.43947685223224));
#50729=CARTESIAN_POINT('Ctrl Pts',(13.8777414232708,-0.0742589286223064,
4.45790169736071));
#50730=CARTESIAN_POINT('Ctrl Pts',(13.8699957084852,1.23414887176878E-6,
4.4579133809027));
#50731=CARTESIAN_POINT('Ctrl Pts',(13.9800042915148,-4.68615130337092E-6,
4.45784092071359));
#50732=CARTESIAN_POINT('Ctrl Pts',(13.9833817079953,-0.0323996211791616,
4.45785275579335));
#50733=CARTESIAN_POINT('Ctrl Pts',(13.9867591244758,-0.064792114138131,
4.45446164082457));
#50734=CARTESIAN_POINT('Ctrl Pts',(13.9901365409563,-0.0964458636128916,
4.44764173788363));
#50735=CARTESIAN_POINT('Ctrl Pts',(13.9980079130062,-0.170217765992045,
4.43174734235885));
#50736=CARTESIAN_POINT('Ctrl Pts',(14.0058792850562,-0.239977073556624,
4.39722897636055));
#50737=CARTESIAN_POINT('Ctrl Pts',(14.0137506571061,-0.297364634468633,
4.34822292324149));
#50738=CARTESIAN_POINT('Ctrl Pts',(14.0216220291561,-0.354752195380644,
4.29921687012243));
#50739=CARTESIAN_POINT('Ctrl Pts',(14.0294934012061,-0.399768009640084,
4.23572312988262));
#50740=CARTESIAN_POINT('Ctrl Pts',(14.037364773256,-0.427017900618165,4.16535006094698));
#50741=CARTESIAN_POINT('Ctrl Pts',(14.045236145306,-0.454267791596245,4.09497699201134));
#50742=CARTESIAN_POINT('Ctrl Pts',(14.0531075173559,-0.463751759292965,
4.01772459437987));
#50743=CARTESIAN_POINT('Ctrl Pts',(14.0609788894059,-0.45433335426851,3.94284990548881));
#50744=CARTESIAN_POINT('Ctrl Pts',(14.0688502614558,-0.444914949244056,
3.86797521659775));
#50745=CARTESIAN_POINT('Ctrl Pts',(14.0767216335058,-0.416594171498428,
3.7954782364471));
#50746=CARTESIAN_POINT('Ctrl Pts',(14.0845930055557,-0.372764656800254,
3.7340461680214));
#50747=CARTESIAN_POINT('Ctrl Pts',(14.0924643776057,-0.328935142102078,
3.67261409959569));
#50748=CARTESIAN_POINT('Ctrl Pts',(14.1003357496557,-0.269596890451354,
3.62224694289495));
#50749=CARTESIAN_POINT('Ctrl Pts',(14.1082071217056,-0.201860314388951,
3.58898011778223));
#50750=CARTESIAN_POINT('Ctrl Pts',(14.1160784937556,-0.134123738326549,
3.55571329266952));
#50751=CARTESIAN_POINT('Ctrl Pts',(14.1239498658055,-0.0579888378524715,
3.53954679914483));
#50752=CARTESIAN_POINT('Ctrl Pts',(14.1318212378555,0.0174212575835846,
3.54241784356498));
#50753=CARTESIAN_POINT('Ctrl Pts',(14.1396926099054,0.0928313530196406,
3.54528888798513));
#50754=CARTESIAN_POINT('Ctrl Pts',(14.1475639819554,0.167516643417675,3.56719747035013));
#50755=CARTESIAN_POINT('Ctrl Pts',(14.1554353540053,0.232527703900953,3.60551831852155));
#50756=CARTESIAN_POINT('Ctrl Pts',(14.1633067260553,0.297538764384231,3.64383916669297));
#50757=CARTESIAN_POINT('Ctrl Pts',(14.1711780981053,0.352875594952755,3.69857228067082));
#50758=CARTESIAN_POINT('Ctrl Pts',(14.1790494701552,0.391907267274456,3.76315907456484));
#50759=CARTESIAN_POINT('Ctrl Pts',(14.1869208422052,0.430938939596158,3.82774586845886));
#50760=CARTESIAN_POINT('Ctrl Pts',(14.1947922142551,0.453665453671035,3.90218634226906));
#50761=CARTESIAN_POINT('Ctrl Pts',(14.2026635863051,0.45736352584659,3.97756040711846));
#50762=CARTESIAN_POINT('Ctrl Pts',(14.210534958355,0.461061598022145,4.05293447196787));
#50763=CARTESIAN_POINT('Ctrl Pts',(14.218406330405,0.445731228298378,4.12924212785648));
#50764=CARTESIAN_POINT('Ctrl Pts',(14.2262777024549,0.413209431587385,4.19733954431574));
#50765=CARTESIAN_POINT('Ctrl Pts',(14.2341490745049,0.380687634876391,4.265436960775));
#50766=CARTESIAN_POINT('Ctrl Pts',(14.2420204465549,0.330974411178171,4.32532413780492));
#50767=CARTESIAN_POINT('Ctrl Pts',(14.2498918186048,0.270026820557645,4.36982488597043));
#50768=CARTESIAN_POINT('Ctrl Pts',(14.2577631906548,0.209079229937118,4.41432563413594));
#50769=CARTESIAN_POINT('Ctrl Pts',(14.2656345627047,0.136897272394287,4.44343995343705));
#50770=CARTESIAN_POINT('Ctrl Pts',(14.2735059347547,0.0621304022332317,
4.45367911922619));
#50771=CARTESIAN_POINT('Ctrl Pts',(14.2756720536747,0.0415553447945806,
4.4564968301158));
#50772=CARTESIAN_POINT('Ctrl Pts',(14.2778381725948,0.020784533837212,4.45788513960506));
#50773=CARTESIAN_POINT('Ctrl Pts',(14.2800042915148,1.11332528513013E-5,
4.45786561359635));
#50774=CARTESIAN_POINT('Origin',(12.5,0.,4.));
#50775=CARTESIAN_POINT('',(14.5800042915148,-1.58578451148518E-6,4.45791318879952));
#50776=CARTESIAN_POINT('',(14.4699957084852,4.96934848862042E-6,4.4578413260902));
#50777=CARTESIAN_POINT('',(12.5,-5.60735153159594E-17,4.457875));
#50778=CARTESIAN_POINT('Ctrl Pts',(14.4699957084852,4.96934848862042E-6,
4.4578413260902));
#50779=CARTESIAN_POINT('Ctrl Pts',(14.4666543524698,0.0320539454002899,
4.45785375637851));
#50780=CARTESIAN_POINT('Ctrl Pts',(14.4633129964543,0.0641003838712636,
4.45453523052653));
#50781=CARTESIAN_POINT('Ctrl Pts',(14.4599716404389,0.0954313752779353,
4.44785911407655));
#50782=CARTESIAN_POINT('Ctrl Pts',(14.452100268389,0.169239101517837,4.43213190746217));
#50783=CARTESIAN_POINT('Ctrl Pts',(14.444228896339,0.2390764403586,4.39777168651743));
#50784=CARTESIAN_POINT('Ctrl Pts',(14.4363575242891,0.296574889592956,4.34889578431359));
#50785=CARTESIAN_POINT('Ctrl Pts',(14.4284861522391,0.354073338827311,4.30001988210975));
#50786=CARTESIAN_POINT('Ctrl Pts',(14.4206147801891,0.39923289845526,4.2366282986468));
#50787=CARTESIAN_POINT('Ctrl Pts',(14.4127434081392,0.4266421670589,4.16631715105832));
#50788=CARTESIAN_POINT('Ctrl Pts',(14.4048720360892,0.454051435662541,4.09600600346984));
#50789=CARTESIAN_POINT('Ctrl Pts',(14.3970006640393,0.463710413241873,4.01877529175582));
#50790=CARTESIAN_POINT('Ctrl Pts',(14.3891292919893,0.454461679188747,3.94387945476197));
#50791=CARTESIAN_POINT('Ctrl Pts',(14.3812579199394,0.445212945135621,3.86898361776811));
#50792=CARTESIAN_POINT('Ctrl Pts',(14.3733865478894,0.417056499450037,3.79642265549441));
#50793=CARTESIAN_POINT('Ctrl Pts',(14.3655151758395,0.373366286239542,3.73489143780602));
#50794=CARTESIAN_POINT('Ctrl Pts',(14.3576438037895,0.329676073029047,3.67336022011762));
#50795=CARTESIAN_POINT('Ctrl Pts',(14.3497724317395,0.270452092293641,3.62285874701452));
#50796=CARTESIAN_POINT('Ctrl Pts',(14.3419010596896,0.202791063664024,3.58943853329022));
#50797=CARTESIAN_POINT('Ctrl Pts',(14.3340296876396,0.135130035034407,3.55601831956592));
#50798=CARTESIAN_POINT('Ctrl Pts',(14.3261583155897,0.0590319585105798,
3.53967936522043));
#50799=CARTESIAN_POINT('Ctrl Pts',(14.3182869435397,-0.0163844490157649,
3.54237954232867));
#50800=CARTESIAN_POINT('Ctrl Pts',(14.3104155714898,-0.0918008565421096,
3.54507971943691));
#50801=CARTESIAN_POINT('Ctrl Pts',(14.3025441994398,-0.166535595070972,
3.56681902799889));
#50802=CARTESIAN_POINT('Ctrl Pts',(14.2946728273899,-0.231633314431234,
3.60499247969884));
#50803=CARTESIAN_POINT('Ctrl Pts',(14.2868014553399,-0.296731033791496,
3.64316593139879));
#50804=CARTESIAN_POINT('Ctrl Pts',(14.2789300832899,-0.352191733983158,
3.6977735262367));
#50805=CARTESIAN_POINT('Ctrl Pts',(14.27105871124,-0.391369643565407,3.76227171909014));
#50806=CARTESIAN_POINT('Ctrl Pts',(14.26318733919,-0.430547553147657,3.82676991194359));
#50807=CARTESIAN_POINT('Ctrl Pts',(14.2553159671401,-0.453442672120494,
3.90115870281258));
#50808=CARTESIAN_POINT('Ctrl Pts',(14.2474445950901,-0.457311513162664,
3.97652419590847));
#50809=CARTESIAN_POINT('Ctrl Pts',(14.2395732230402,-0.461180354204834,
4.05188968900435));
#50810=CARTESIAN_POINT('Ctrl Pts',(14.2317018509902,-0.446022917316338,
4.12823188432714));
#50811=CARTESIAN_POINT('Ctrl Pts',(14.2238304789403,-0.413655495130362,
4.19640281260034));
#50812=CARTESIAN_POINT('Ctrl Pts',(14.2159591068903,-0.381288072944386,
4.26457374087354));
#50813=CARTESIAN_POINT('Ctrl Pts',(14.2080877348403,-0.33171066546093,4.32457340209717));
#50814=CARTESIAN_POINT('Ctrl Pts',(14.2002163627904,-0.270864058094251,
4.36921212802613));
#50815=CARTESIAN_POINT('Ctrl Pts',(14.1923449907404,-0.210017450727571,
4.41385085395509));
#50816=CARTESIAN_POINT('Ctrl Pts',(14.1844736186905,-0.137901643477669,
4.44312864458938));
#50817=CARTESIAN_POINT('Ctrl Pts',(14.1766022466405,-0.0631581639595259,
4.45353718675995));
#50818=CARTESIAN_POINT('Ctrl Pts',(14.1744000672554,-0.0422471272657682,
4.45644919204336));
#50819=CARTESIAN_POINT('Ctrl Pts',(14.1721978878703,-0.021130418320356,
4.45788427006097));
#50820=CARTESIAN_POINT('Ctrl Pts',(14.1699957084852,-1.10604184835328E-5,
4.4578646218584));
#50821=CARTESIAN_POINT('Ctrl Pts',(14.2800042915148,1.11332528513013E-5,
4.45786561359635));
#50822=CARTESIAN_POINT('Ctrl Pts',(14.2857095446447,-0.0547030874695854,
4.45781418483069));
#50823=CARTESIAN_POINT('Ctrl Pts',(14.2914147977746,-0.109435272994953,
4.44799629651036));
#50824=CARTESIAN_POINT('Ctrl Pts',(14.2971200509045,-0.16065599949712,4.42880599334559));
#50825=CARTESIAN_POINT('Ctrl Pts',(14.3049914229545,-0.231323748287136,
4.40232968939868));
#50826=CARTESIAN_POINT('Ctrl Pts',(14.3128627950045,-0.295307463087888,
4.35801306922771));
#50827=CARTESIAN_POINT('Ctrl Pts',(14.3207341670544,-0.344940072567234,
4.30116652609615));
#50828=CARTESIAN_POINT('Ctrl Pts',(14.3286055391044,-0.394572682046581,
4.24431998296459));
#50829=CARTESIAN_POINT('Ctrl Pts',(14.3364769111543,-0.429854186204522,
4.17494351687244));
#50830=CARTESIAN_POINT('Ctrl Pts',(14.3443482832043,-0.446556856002091,
4.10135040434572));
#50831=CARTESIAN_POINT('Ctrl Pts',(14.3522196552542,-0.46325952579966,4.027757291819));
#50832=CARTESIAN_POINT('Ctrl Pts',(14.3600910273042,-0.461383361236856,
3.9499475328577));
#50833=CARTESIAN_POINT('Ctrl Pts',(14.3679623993541,-0.441153180262727,
3.87724495265939));
#50834=CARTESIAN_POINT('Ctrl Pts',(14.3758337714041,-0.420922999288597,
3.80454237246108));
#50835=CARTESIAN_POINT('Ctrl Pts',(14.383705143454,-0.382338801903142,3.73694697102576));
#50836=CARTESIAN_POINT('Ctrl Pts',(14.391576515504,-0.330024073856894,3.68255860260764));
#50837=CARTESIAN_POINT('Ctrl Pts',(14.399447887554,-0.277709345810648,3.62817023418952));
#50838=CARTESIAN_POINT('Ctrl Pts',(14.4073192596039,-0.21166408710361,3.58698889878861));
#50839=CARTESIAN_POINT('Ctrl Pts',(14.4151906316539,-0.139802400742051,
3.56394929325792));
#50840=CARTESIAN_POINT('Ctrl Pts',(14.4230620037038,-0.0679407143804897,
3.54090968772722));
#50841=CARTESIAN_POINT('Ctrl Pts',(14.4309333757538,0.00973739963559066,
3.53601181206673));
#50842=CARTESIAN_POINT('Ctrl Pts',(14.4388047478037,0.0839238909224197,
3.54984257127538));
#50843=CARTESIAN_POINT('Ctrl Pts',(14.4466761198537,0.158110382209248,3.56367333048403));
#50844=CARTESIAN_POINT('Ctrl Pts',(14.4545474919037,0.228805250766822,3.59623272456181));
#50845=CARTESIAN_POINT('Ctrl Pts',(14.4624188639536,0.287537237904754,3.64361921078484));
#50846=CARTESIAN_POINT('Ctrl Pts',(14.4702902360036,0.346269225042686,3.69100569700788));
#50847=CARTESIAN_POINT('Ctrl Pts',(14.4781616080535,0.393038330760977,3.75321927537615));
#50848=CARTESIAN_POINT('Ctrl Pts',(14.4860329801035,0.422240284179214,3.8228049873169));
#50849=CARTESIAN_POINT('Ctrl Pts',(14.4939043521534,0.451442237597453,3.89239069925764));
#50850=CARTESIAN_POINT('Ctrl Pts',(14.5017757242034,0.463077038715637,3.96934854477086));
#50851=CARTESIAN_POINT('Ctrl Pts',(14.5096470962533,0.45575050699275,4.04445678215295));
#50852=CARTESIAN_POINT('Ctrl Pts',(14.5175184683033,0.448423975269863,4.11956501953505));
#50853=CARTESIAN_POINT('Ctrl Pts',(14.5253898403532,0.422136110705906,4.19282364878603));
#50854=CARTESIAN_POINT('Ctrl Pts',(14.5332612124032,0.380036948171907,4.2554541996672));
#50855=CARTESIAN_POINT('Ctrl Pts',(14.5411325844532,0.337937785637909,4.31808475054837));
#50856=CARTESIAN_POINT('Ctrl Pts',(14.5490039565031,0.28002732513387,4.37008722305972));
#50857=CARTESIAN_POINT('Ctrl Pts',(14.5568753285531,0.213244889156206,4.40523023992844));
#50858=CARTESIAN_POINT('Ctrl Pts',(14.5645849828737,0.147834501639678,4.43965124177167));
#50859=CARTESIAN_POINT('Ctrl Pts',(14.5722946371942,0.0739129441497101,
4.45789842831743));
#50860=CARTESIAN_POINT('Ctrl Pts',(14.5800042915148,-1.58578451148518E-6,
4.45791318879952));
#50861=CARTESIAN_POINT('Origin',(12.5,0.,4.));
#50862=CARTESIAN_POINT('',(14.8800042915148,-1.01702808208336E-5,4.45785711824254));
#50863=CARTESIAN_POINT('',(14.7699957084852,8.6346448269735E-6,4.45789857801605));
#50864=CARTESIAN_POINT('',(12.5,-5.60735153159594E-17,4.457875));
#50865=CARTESIAN_POINT('Ctrl Pts',(14.7699957084852,8.6346448269735E-6,
4.45789857801605));
#50866=CARTESIAN_POINT('Ctrl Pts',(14.7689821891192,0.00972641784825355,
4.45790700998655));
#50867=CARTESIAN_POINT('Ctrl Pts',(14.7679686697532,0.01944367562558,4.45760386164098));
#50868=CARTESIAN_POINT('Ctrl Pts',(14.7669551503872,0.0291408329004781,
4.45698549795522));
#50869=CARTESIAN_POINT('Ctrl Pts',(14.7590837783372,0.104452598317788,4.45218305332902));
#50870=CARTESIAN_POINT('Ctrl Pts',(14.7512124062873,0.178551969979598,4.4283678943965));
#50871=CARTESIAN_POINT('Ctrl Pts',(14.7433410342373,0.242559732875008,4.38839375563686));
#50872=CARTESIAN_POINT('Ctrl Pts',(14.7354696621874,0.30656749577042,4.34841961687722));
#50873=CARTESIAN_POINT('Ctrl Pts',(14.7275982901374,0.360483649899433,4.29228649829047));
#50874=CARTESIAN_POINT('Ctrl Pts',(14.7197269180875,0.397847504376097,4.22672074611392));
#50875=CARTESIAN_POINT('Ctrl Pts',(14.7118555460375,0.435211358852761,4.16115499393738));
#50876=CARTESIAN_POINT('Ctrl Pts',(14.7039841739875,0.456022913677073,4.08615660817103));
#50877=CARTESIAN_POINT('Ctrl Pts',(14.6961128019376,0.457788351878884,4.01071253147039));
#50878=CARTESIAN_POINT('Ctrl Pts',(14.6882414298876,0.459553790080695,3.93526845476975));
#50879=CARTESIAN_POINT('Ctrl Pts',(14.6803700578377,0.442273111660005,3.85937868713481));
#50880=CARTESIAN_POINT('Ctrl Pts',(14.6724986857877,0.408017034045316,3.79213698410258));
#50881=CARTESIAN_POINT('Ctrl Pts',(14.6646273137378,0.373760956430627,3.72489528107034));
#50882=CARTESIAN_POINT('Ctrl Pts',(14.6567559416878,0.32252947962194,3.6663016426408));
#50883=CARTESIAN_POINT('Ctrl Pts',(14.6488845696379,0.260461593653079,3.6233772554918));
#50884=CARTESIAN_POINT('Ctrl Pts',(14.6410131975879,0.198393707684219,3.5804528683428));
#50885=CARTESIAN_POINT('Ctrl Pts',(14.6331418255379,0.125489412555185,3.55319773247434));
#50886=CARTESIAN_POINT('Ctrl Pts',(14.625270453488,0.0504847191830214,3.54487778940425));
#50887=CARTESIAN_POINT('Ctrl Pts',(14.617399081438,-0.0245199741891427,
3.53655784633416));
#50888=CARTESIAN_POINT('Ctrl Pts',(14.6095277093881,-0.101625065804437,
3.54717309606245));
#50889=CARTESIAN_POINT('Ctrl Pts',(14.6016563373381,-0.171591169681571,
3.57545152934398));
#50890=CARTESIAN_POINT('Ctrl Pts',(14.5937849652882,-0.241557273558703,
3.6037299626255));
#50891=CARTESIAN_POINT('Ctrl Pts',(14.5859135932382,-0.304384389697674,
3.64967157946028));
#50892=CARTESIAN_POINT('Ctrl Pts',(14.5780422211883,-0.352544040227279,
3.70777126570269));
#50893=CARTESIAN_POINT('Ctrl Pts',(14.5701708491383,-0.400703690756885,
3.7658709519451));
#50894=CARTESIAN_POINT('Ctrl Pts',(14.5622994770883,-0.434195875677124,
3.83612870759516));
#50895=CARTESIAN_POINT('Ctrl Pts',(14.5544281050384,-0.449007277354457,
3.91012565253846));
#50896=CARTESIAN_POINT('Ctrl Pts',(14.5465567329884,-0.46381867903179,3.98412259748177));
#50897=CARTESIAN_POINT('Ctrl Pts',(14.5386853609385,-0.459949297466218,
4.06185873171832));
#50898=CARTESIAN_POINT('Ctrl Pts',(14.5308139888885,-0.437862794771992,
4.13401905238929));
#50899=CARTESIAN_POINT('Ctrl Pts',(14.5229426168386,-0.415776292077766,
4.20617937306026));
#50900=CARTESIAN_POINT('Ctrl Pts',(14.5150712447886,-0.375472668254887,
4.27276388016565));
#50901=CARTESIAN_POINT('Ctrl Pts',(14.5071998727387,-0.321781445311454,
4.32579385338299));
#50902=CARTESIAN_POINT('Ctrl Pts',(14.4993285006887,-0.26809022236802,4.37882382660034));
#50903=CARTESIAN_POINT('Ctrl Pts',(14.4914571286387,-0.201011400304033,
4.41829926592964));
#50904=CARTESIAN_POINT('Ctrl Pts',(14.4835857565888,-0.128582932452519,
4.43948988945229));
#50905=CARTESIAN_POINT('Ctrl Pts',(14.4790557405542,-0.0868999680795747,
4.45168520479633));
#50906=CARTESIAN_POINT('Ctrl Pts',(14.4745257245197,-0.0434451672832877,
4.45782447382869));
#50907=CARTESIAN_POINT('Ctrl Pts',(14.4699957084852,4.96934848862042E-6,
4.4578413260902));
#50908=CARTESIAN_POINT('Ctrl Pts',(14.5800042915148,-1.58578451148518E-6,
4.45791318879952));
#50909=CARTESIAN_POINT('Ctrl Pts',(14.5801660092442,-0.00155201715944126,
4.45791349841543));
#50910=CARTESIAN_POINT('Ctrl Pts',(14.5803277269736,-0.00310244544229786,
4.45790578589721));
#50911=CARTESIAN_POINT('Ctrl Pts',(14.5804894447029,-0.0046527920161852,
4.45789003224535));
#50912=CARTESIAN_POINT('Ctrl Pts',(14.5883608167529,-0.0801136257596197,
4.45712324646747));
#50913=CARTESIAN_POINT('Ctrl Pts',(14.5962321888029,-0.155380881795201,
4.43730611368561));
#50914=CARTESIAN_POINT('Ctrl Pts',(14.6041035608528,-0.22143539919095,4.4008132908088));
#50915=CARTESIAN_POINT('Ctrl Pts',(14.6119749329028,-0.287489916586699,
4.36432046793199));
#50916=CARTESIAN_POINT('Ctrl Pts',(14.6198463049527,-0.344331695342615,
4.31115195496024));
#50917=CARTESIAN_POINT('Ctrl Pts',(14.6277176770027,-0.38514947146564,4.24767885402976));
#50918=CARTESIAN_POINT('Ctrl Pts',(14.6355890490526,-0.425967247588666,
4.18420575309928));
#50919=CARTESIAN_POINT('Ctrl Pts',(14.6434604211026,-0.4507610210788,4.11042806421008));
#50920=CARTESIAN_POINT('Ctrl Pts',(14.6513317931525,-0.45655979174196,4.03518645571321));
#50921=CARTESIAN_POINT('Ctrl Pts',(14.6592031652025,-0.462358562405121,
3.95994484721634));
#50922=CARTESIAN_POINT('Ctrl Pts',(14.6670745372524,-0.449162330241309,
3.8832393191118));
#50923=CARTESIAN_POINT('Ctrl Pts',(14.6749459093024,-0.41855237967279,3.81426137832517));
#50924=CARTESIAN_POINT('Ctrl Pts',(14.6828172813524,-0.387942429104271,
3.74528343753854));
#50925=CARTESIAN_POINT('Ctrl Pts',(14.6906886534023,-0.339918760131043,
3.68403308406983));
#50926=CARTESIAN_POINT('Ctrl Pts',(14.6985600254523,-0.280235976103336,
3.63784985464301));
#50927=CARTESIAN_POINT('Ctrl Pts',(14.7064313975022,-0.220553192075631,
3.5916666252162));
#50928=CARTESIAN_POINT('Ctrl Pts',(14.7143027695522,-0.149211292993445,
3.5605505198313));
#50929=CARTESIAN_POINT('Ctrl Pts',(14.7221741416021,-0.0747590701011626,
3.54823013427646));
#50930=CARTESIAN_POINT('Ctrl Pts',(14.7300455136521,-0.000306847208877067,
3.53590974872161));
#50931=CARTESIAN_POINT('Ctrl Pts',(14.737916885702,0.0772556994935079,3.54238508299684));
#50932=CARTESIAN_POINT('Ctrl Pts',(14.745788257752,0.148634367597872,3.5668802073009));
#50933=CARTESIAN_POINT('Ctrl Pts',(14.753659629802,0.220013035702235,3.59137533160497));
#50934=CARTESIAN_POINT('Ctrl Pts',(14.7615310018519,0.285207825208577,3.63389024593787));
#50935=CARTESIAN_POINT('Ctrl Pts',(14.7694023739019,0.336406544142474,3.68933045342307));
#50936=CARTESIAN_POINT('Ctrl Pts',(14.7772737459518,0.387605263076371,3.74477066090827));
#50937=CARTESIAN_POINT('Ctrl Pts',(14.7851451180018,0.424807911437823,3.81313616154577));
#50938=CARTESIAN_POINT('Ctrl Pts',(14.7930164900517,0.443556551112275,3.88623481973509));
#50939=CARTESIAN_POINT('Ctrl Pts',(14.8008878621017,0.462305190786727,3.9593334779244));
#50940=CARTESIAN_POINT('Ctrl Pts',(14.8087592341516,0.462599821774179,4.03716529366552));
#50941=CARTESIAN_POINT('Ctrl Pts',(14.8166306062016,0.444405141642572,4.11040380200553));
#50942=CARTESIAN_POINT('Ctrl Pts',(14.8245019782516,0.426210461510966,4.18364231034555));
#50943=CARTESIAN_POINT('Ctrl Pts',(14.8323733503015,0.389526470260302,4.25228751128446));
#50944=CARTESIAN_POINT('Ctrl Pts',(14.8402447223515,0.338748948932789,4.3081137476731));
#50945=CARTESIAN_POINT('Ctrl Pts',(14.8481160944014,0.287971427605278,4.36393998406173));
#50946=CARTESIAN_POINT('Ctrl Pts',(14.8559874664514,0.22310037620092,4.40694725590009));
#50947=CARTESIAN_POINT('Ctrl Pts',(14.8638588385013,0.151909206873508,4.43198208217373));
#50948=CARTESIAN_POINT('Ctrl Pts',(14.8692406561725,0.103234351881841,4.44909890368578));
#50949=CARTESIAN_POINT('Ctrl Pts',(14.8746224738437,0.0516050086776526,
4.45781408155485));
#50950=CARTESIAN_POINT('Ctrl Pts',(14.8800042915148,-1.01702808208336E-5,
4.45785711824254));
#50951=CARTESIAN_POINT('Origin',(12.5,0.,4.));
#50952=CARTESIAN_POINT('',(15.1,-5.60735153159594E-17,4.457875));
#50953=CARTESIAN_POINT('',(15.0699957084852,-1.05870731373636E-5,4.45788944868556));
#50954=CARTESIAN_POINT('',(12.5,-5.60735153159594E-17,4.457875));
#50955=CARTESIAN_POINT('',(15.1,-0.269165465906718,4.37040446485999));
#50956=CARTESIAN_POINT('Origin',(15.1,0.,4.));
#50957=CARTESIAN_POINT('Ctrl Pts',(15.1,-0.269173508333955,4.37043259773194));
#50958=CARTESIAN_POINT('Ctrl Pts',(15.0991842588284,-0.262849866117432,
4.37503549456412));
#50959=CARTESIAN_POINT('Ctrl Pts',(15.0983685176569,-0.256407545646713,
4.37947450812006));
#50960=CARTESIAN_POINT('Ctrl Pts',(15.0975527764853,-0.249853611926923,
4.38374199825787));
#50961=CARTESIAN_POINT('Ctrl Pts',(15.0896814044354,-0.186612411779406,
4.42492050409441));
#50962=CARTESIAN_POINT('Ctrl Pts',(15.0818100323854,-0.112978907049287,
4.45012847221118));
#50963=CARTESIAN_POINT('Ctrl Pts',(15.0739386603355,-0.0377721395608013,
4.45635245505497));
#50964=CARTESIAN_POINT('Ctrl Pts',(15.072624343052,-0.0252145379490987,
4.45739170058566));
#50965=CARTESIAN_POINT('Ctrl Pts',(15.0713100257686,-0.0126130730861363,
4.45790166433459));
#50966=CARTESIAN_POINT('Ctrl Pts',(15.0699957084852,-1.05870731373636E-5,
4.45788944868556));
#50967=CARTESIAN_POINT('Origin',(11.8752146997001,0.,4.));
#50968=CARTESIAN_POINT('',(14.9247853002999,-1.38824472118437E-5,4.62497559137666));
#50969=CARTESIAN_POINT('',(15.0252146997001,-1.44513692928093E-5,4.62501972247551));
#50970=CARTESIAN_POINT('',(11.8752146997001,-1.68747709936658E-14,4.625));
#50971=CARTESIAN_POINT('',(15.1,-0.624993681275899,4.00281040303151));
#50972=CARTESIAN_POINT('Ctrl Pts',(15.0252146997001,-1.44513692928189E-5,
4.62501972247551));
#50973=CARTESIAN_POINT('Ctrl Pts',(15.0265290169835,-0.017216861979444,
4.62503639685311));
#50974=CARTESIAN_POINT('Ctrl Pts',(15.0357147063169,-0.137433797398843,
4.62017138475037));
#50975=CARTESIAN_POINT('Ctrl Pts',(15.0527717677003,-0.355236031271534,
4.54560815721762));
#50976=CARTESIAN_POINT('Ctrl Pts',(15.0763858838501,-0.571652475026301,
4.31158258982903));
#50977=CARTESIAN_POINT('Ctrl Pts',(15.09212862795,-0.624530364890795,4.10584538053252));
#50978=CARTESIAN_POINT('Ctrl Pts',(15.1,-0.624993681275899,4.00281040303152));
#50979=CARTESIAN_POINT('',(15.1,0.314930721058197,3.46014479632612));
#50980=CARTESIAN_POINT('Origin',(15.1,0.,4.));
#50981=CARTESIAN_POINT('Ctrl Pts',(14.9247853002999,-1.38824472118368E-5,
4.62497559137666));
#50982=CARTESIAN_POINT('Ctrl Pts',(14.9272748546787,-0.0326052931943186,
4.62500276606431));
#50983=CARTESIAN_POINT('Ctrl Pts',(14.9376357811074,-0.168225686180582,
4.61457389311938));
#50984=CARTESIAN_POINT('Ctrl Pts',(14.9558680795861,-0.394527586443172,
4.517903766532));
#50985=CARTESIAN_POINT('Ctrl Pts',(14.979482195736,-0.593077772790822,4.26857965265179));
#50986=CARTESIAN_POINT('Ctrl Pts',(15.0030963118859,-0.649493436571599,
3.95488773069898));
#50987=CARTESIAN_POINT('Ctrl Pts',(15.0267104280357,-0.550252000240565,
3.65200904506483));
#50988=CARTESIAN_POINT('Ctrl Pts',(15.0503245441856,-0.319142060764588,
3.43252503194012));
#50989=CARTESIAN_POINT('Ctrl Pts',(15.0739386603355,-0.0115409051696555,
3.34904846156061));
#50990=CARTESIAN_POINT('Ctrl Pts',(15.0904971456069,0.20608092381284,3.39989411918499));
#50991=CARTESIAN_POINT('Ctrl Pts',(15.0991842588284,0.305720220830039,3.45471854406458));
#50992=CARTESIAN_POINT('Ctrl Pts',(15.1,0.314937815442301,3.46010549098218));
#50993=CARTESIAN_POINT('Origin',(11.8752146997001,0.,4.));
#50994=CARTESIAN_POINT('',(14.6247853002999,-2.16459804047719E-6,4.62505212776347));
#50995=CARTESIAN_POINT('',(14.7252146997001,1.17863019661874E-5,4.62503218402409));
#50996=CARTESIAN_POINT('',(11.8752146997001,-1.68747709936658E-14,4.625));
#50997=CARTESIAN_POINT('Ctrl Pts',(14.7252146997001,1.17863019662174E-5,
4.62503218402409));
#50998=CARTESIAN_POINT('Ctrl Pts',(14.7320725523841,-0.0897427467603322,
4.62495430540108));
#50999=CARTESIAN_POINT('Ctrl Pts',(14.746801777118,-0.282587126126967,4.58296482291278));
#51000=CARTESIAN_POINT('Ctrl Pts',(14.7694023739019,-0.520130285395982,
4.39158760667368));
#51001=CARTESIAN_POINT('Ctrl Pts',(14.7930164900517,-0.64367318065081,4.09778141619902));
#51002=CARTESIAN_POINT('Ctrl Pts',(14.8166306062016,-0.612955311082805,
3.78054123783642));
#51003=CARTESIAN_POINT('Ctrl Pts',(14.8402447223515,-0.435338447621071,
3.51589585985611));
#51004=CARTESIAN_POINT('Ctrl Pts',(14.8638588385013,-0.153389665944836,
3.36726945127358));
#51005=CARTESIAN_POINT('Ctrl Pts',(14.8874729546512,0.165319955489652,3.37028123293502));
#51006=CARTESIAN_POINT('Ctrl Pts',(14.9110870708011,0.444409630539555,3.52420969451069));
#51007=CARTESIAN_POINT('Ctrl Pts',(14.9347011869509,0.616993161964042,3.79216419995926));
#51008=CARTESIAN_POINT('Ctrl Pts',(14.9583153031008,0.641710593195818,4.10992889087348));
#51009=CARTESIAN_POINT('Ctrl Pts',(14.9819294192507,0.512636325700993,4.40134645341462));
#51010=CARTESIAN_POINT('Ctrl Pts',(15.0042292181171,0.274729866520086,4.58571614948967));
#51011=CARTESIAN_POINT('Ctrl Pts',(15.0186576449336,0.0858074045169303,
4.62493653494651));
#51012=CARTESIAN_POINT('Ctrl Pts',(15.0252146997001,-1.44513692928189E-5,
4.62501972247551));
#51013=CARTESIAN_POINT('Ctrl Pts',(14.6247853002999,-2.16459804049194E-6,
4.62505212776347));
#51014=CARTESIAN_POINT('Ctrl Pts',(14.6249470180292,-0.00211850554115318,
4.62505255038961));
#51015=CARTESIAN_POINT('Ctrl Pts',(14.6329801078086,-0.107244412024774,
4.62452960748548));
#51016=CARTESIAN_POINT('Ctrl Pts',(14.6488845696379,-0.314835022974042,
4.56987302880665));
#51017=CARTESIAN_POINT('Ctrl Pts',(14.6724986857877,-0.547602339746838,
4.35214775046202));
#51018=CARTESIAN_POINT('Ctrl Pts',(14.6961128019376,-0.649132943719538,
4.05002781234082));
#51019=CARTESIAN_POINT('Ctrl Pts',(14.7197269180875,-0.595094318970103,
3.73591836064326));
#51020=CARTESIAN_POINT('Ctrl Pts',(14.7433410342373,-0.398437197867616,
3.48509791236843));
#51021=CARTESIAN_POINT('Ctrl Pts',(14.7669551503872,-0.1062918289807,3.35767733339665));
#51022=CARTESIAN_POINT('Ctrl Pts',(14.7905692665371,0.211327117384507,3.38419385377023));
#51023=CARTESIAN_POINT('Ctrl Pts',(14.8141833826869,0.478300047385911,3.5582926020622));
#51024=CARTESIAN_POINT('Ctrl Pts',(14.8377974988368,0.630645044771057,3.83824960712979));
#51025=CARTESIAN_POINT('Ctrl Pts',(14.8614116149867,0.631851559871185,4.15697121131127));
#51026=CARTESIAN_POINT('Ctrl Pts',(14.8850257311365,0.481630465478622,4.4380735902585));
#51027=CARTESIAN_POINT('Ctrl Pts',(14.9061502929076,0.243989509668873,4.59562135563586));
#51028=CARTESIAN_POINT('Ctrl Pts',(14.9194034826287,0.0704409072858971,
4.62491684623921));
#51029=CARTESIAN_POINT('Ctrl Pts',(14.9247853002999,-1.38824472118368E-5,
4.62497559137666));
#51030=CARTESIAN_POINT('Origin',(11.8752146997001,0.,4.));
#51031=CARTESIAN_POINT('',(14.3247853002999,1.51969053300144E-5,4.6249871875462));
#51032=CARTESIAN_POINT('',(14.4252146997001,6.78316748347314E-6,4.62495403506715));
#51033=CARTESIAN_POINT('',(11.8752146997001,-1.68747709936658E-14,4.625));
#51034=CARTESIAN_POINT('Ctrl Pts',(14.4252146997001,6.78316748347826E-6,
4.62495403506715));
#51035=CARTESIAN_POINT('Ctrl Pts',(14.4297447157347,-0.0593027126443913,
4.62493103170719));
#51036=CARTESIAN_POINT('Ctrl Pts',(14.4421461038192,-0.221686029527806,
4.60198961095629));
#51037=CARTESIAN_POINT('Ctrl Pts',(14.4624188639536,-0.457506203155893,
4.46321101183598));
#51038=CARTESIAN_POINT('Ctrl Pts',(14.4860329801035,-0.622549707754089,
4.19054718257559));
#51039=CARTESIAN_POINT('Ctrl Pts',(14.5096470962533,-0.63839484111024,3.87221739454711));
#51040=CARTESIAN_POINT('Ctrl Pts',(14.5332612124032,-0.501244206711231,
3.58451159745434));
#51041=CARTESIAN_POINT('Ctrl Pts',(14.5568753285531,-0.243966908844842,
3.39638048838484));
#51042=CARTESIAN_POINT('Ctrl Pts',(14.5804894447029,0.0717787570654544,
3.35291099727801));
#51043=CARTESIAN_POINT('Ctrl Pts',(14.6041035608528,0.370322144162233,3.46452089026927));
#51044=CARTESIAN_POINT('Ctrl Pts',(14.6277176770027,0.580115251486915,3.70446207957941));
#51045=CARTESIAN_POINT('Ctrl Pts',(14.6513317931525,0.650879700384091,4.0152309888134));
#51046=CARTESIAN_POINT('Ctrl Pts',(14.6749459093024,0.565656298155129,4.32234968564526));
#51047=CARTESIAN_POINT('Ctrl Pts',(14.6985600254523,0.344869426209941,4.55221503612336));
#51048=CARTESIAN_POINT('Ctrl Pts',(14.7153162889182,0.129554394067723,4.62141618582314));
#51049=CARTESIAN_POINT('Ctrl Pts',(14.7242011803341,0.0132765736394338,
4.62504369367533));
#51050=CARTESIAN_POINT('Ctrl Pts',(14.7252146997001,1.17863019662174E-5,
4.62503218402409));
#51051=CARTESIAN_POINT('Ctrl Pts',(14.3247853002999,1.51969053300109E-5,
4.6249871875462));
#51052=CARTESIAN_POINT('Ctrl Pts',(14.3304905534298,-0.0746697890657793,
4.62491698721088));
#51053=CARTESIAN_POINT('Ctrl Pts',(14.3440671786096,-0.252453835406249,
4.59302599116618));
#51054=CARTESIAN_POINT('Ctrl Pts',(14.3655151758395,-0.490432948250941,
4.42819608115853));
#51055=CARTESIAN_POINT('Ctrl Pts',(14.3891292919893,-0.634910852255616,
4.14409916841427));
#51056=CARTESIAN_POINT('Ctrl Pts',(14.4127434081392,-0.627227950688033,
3.82546788683648));
#51057=CARTESIAN_POINT('Ctrl Pts',(14.4363575242891,-0.469225504392149,
3.54866444115539));
#51058=CARTESIAN_POINT('Ctrl Pts',(14.4599716404389,-0.198769899531221,
3.38002670405092));
#51059=CARTESIAN_POINT('Ctrl Pts',(14.4835857565888,0.11932229545683,3.35996988316441));
#51060=CARTESIAN_POINT('Ctrl Pts',(14.5071998727387,0.408818071695872,3.49330073524378));
#51061=CARTESIAN_POINT('Ctrl Pts',(14.5308139888885,0.600337751131954,3.74806559342675));
#51062=CARTESIAN_POINT('Ctrl Pts',(14.5544281050384,0.647982309355475,4.06320828594604));
#51063=CARTESIAN_POINT('Ctrl Pts',(14.5780422211883,0.540333396317157,4.36320267272319));
#51064=CARTESIAN_POINT('Ctrl Pts',(14.6014946196088,0.304813865567294,4.57469465218781));
#51065=CARTESIAN_POINT('Ctrl Pts',(14.6170756459793,0.100891269655612,4.62503197968527));
#51066=CARTESIAN_POINT('Ctrl Pts',(14.6247853002999,-2.16459804049194E-6,
4.62505212776347));
#51067=CARTESIAN_POINT('Origin',(11.8752146997001,0.,4.));
#51068=CARTESIAN_POINT('',(14.0247853002999,-6.3966029390794E-6,4.62495348172753));
#51069=CARTESIAN_POINT('',(14.1252146997001,-1.50974863142078E-5,4.62498583382255));
#51070=CARTESIAN_POINT('',(11.8752146997001,-1.68747709936658E-14,4.625));
#51071=CARTESIAN_POINT('Ctrl Pts',(14.1252146997001,-1.50974863141889E-5,
4.62498583382255));
#51072=CARTESIAN_POINT('Ctrl Pts',(14.1274168790852,-0.0288430498503269,
4.62501265364587));
#51073=CARTESIAN_POINT('Ctrl Pts',(14.1374904305203,-0.160695812902997,
4.61605202430223));
#51074=CARTESIAN_POINT('Ctrl Pts',(14.1554353540053,-0.385112282251534,
4.52494275637564));
#51075=CARTESIAN_POINT('Ctrl Pts',(14.1790494701552,-0.588131968915973,
4.27924389796604));
#51076=CARTESIAN_POINT('Ctrl Pts',(14.2026635863051,-0.65020173504413,3.96662229549764));
#51077=CARTESIAN_POINT('Ctrl Pts',(14.2262777024549,-0.556446129094758,
3.66199989226673));
#51078=CARTESIAN_POINT('Ctrl Pts',(14.2498918186048,-0.329334334698108,
3.43838156778717));
#51079=CARTESIAN_POINT('Ctrl Pts',(14.2735059347547,-0.0232952743833569,
3.34935901020328));
#51080=CARTESIAN_POINT('Ctrl Pts',(14.2971200509045,0.28832666060365,3.41626709515619));
#51081=CARTESIAN_POINT('Ctrl Pts',(14.3207341670544,0.530849104237583,3.62307083431711));
#51082=CARTESIAN_POINT('Ctrl Pts',(14.3443482832043,0.646149864620809,3.92020827196535));
#51083=CARTESIAN_POINT('Ctrl Pts',(14.3679623993541,0.606596311879891,4.2364683526943));
#51084=CARTESIAN_POINT('Ctrl Pts',(14.391576515504,0.42166773027486,4.49605714656388));
#51085=CARTESIAN_POINT('Ctrl Pts',(14.4106606156193,0.190545343529355,4.60977018898031));
#51086=CARTESIAN_POINT('Ctrl Pts',(14.4218733436847,0.0437536792250838,
4.62497100242767));
#51087=CARTESIAN_POINT('Ctrl Pts',(14.4252146997001,6.78316748347826E-6,
4.62495403506715));
#51088=CARTESIAN_POINT('Ctrl Pts',(14.0247853002999,-6.39660293913491E-6,
4.62495348172753));
#51089=CARTESIAN_POINT('Ctrl Pts',(14.0281627167804,-0.0442255271350925,
4.62496963662755));
#51090=CARTESIAN_POINT('Ctrl Pts',(14.0394115053108,-0.191490205391595,
4.6095527480466));
#51091=CARTESIAN_POINT('Ctrl Pts',(14.0585316658912,-0.422790583021024,
4.49510047824495));
#51092=CARTESIAN_POINT('Ctrl Pts',(14.0821457820411,-0.60713052675338,4.23509335195577));
#51093=CARTESIAN_POINT('Ctrl Pts',(14.1057598981909,-0.645967413308333,
3.91874446730605));
#51094=CARTESIAN_POINT('Ctrl Pts',(14.1293740143408,-0.529993712466286,
3.62186903671368));
#51095=CARTESIAN_POINT('Ctrl Pts',(14.1529881304907,-0.287003328966194,
3.41561532377041));
#51096=CARTESIAN_POINT('Ctrl Pts',(14.1766022466405,0.0247694002478971,
3.34941346658496));
#51097=CARTESIAN_POINT('Ctrl Pts',(14.2002163627904,0.330605970264406,3.43912920108534));
#51098=CARTESIAN_POINT('Ctrl Pts',(14.2238304789403,0.557210518047066,3.66326152695696));
#51099=CARTESIAN_POINT('Ctrl Pts',(14.2474445950901,0.650275686248857,3.96809557204375));
#51100=CARTESIAN_POINT('Ctrl Pts',(14.27105871124,0.587497759452106,4.28057573538778));
#51101=CARTESIAN_POINT('Ctrl Pts',(14.2946728273899,0.383921904832036,4.52581397056352));
#51102=CARTESIAN_POINT('Ctrl Pts',(14.3125816904098,0.159750963363977,4.61623247111552));
#51103=CARTESIAN_POINT('Ctrl Pts',(14.3226191813798,0.0283709170587055,
4.62501384057475));
#51104=CARTESIAN_POINT('Ctrl Pts',(14.3247853002999,1.51969053300109E-5,
4.6249871875462));
#51105=CARTESIAN_POINT('Origin',(11.8752146997001,0.,4.));
#51106=CARTESIAN_POINT('',(13.7247853002999,-1.20831421157597E-5,4.62503091248755));
#51107=CARTESIAN_POINT('',(13.8252146997001,1.68461488569462E-6,4.62505238998457));
#51108=CARTESIAN_POINT('',(11.8752146997001,-1.68747709936658E-14,4.625));
#51109=CARTESIAN_POINT('Ctrl Pts',(13.8252146997001,1.68461488569581E-6,
4.62505238998457));
#51110=CARTESIAN_POINT('Ctrl Pts',(13.8329604144858,-0.101363538932993,
4.62503644193381));
#51111=CARTESIAN_POINT('Ctrl Pts',(13.8485775013214,-0.305753798836605,
4.57432856173903));
#51112=CARTESIAN_POINT('Ctrl Pts',(13.8720659602069,-0.541154937947787,
4.36197748624323));
#51113=CARTESIAN_POINT('Ctrl Pts',(13.8956800763568,-0.648123865072376,
4.06173996222779));
#51114=CARTESIAN_POINT('Ctrl Pts',(13.9192941925067,-0.599765396122921,
3.74670602647169));
#51115=CARTESIAN_POINT('Ctrl Pts',(13.9429083086565,-0.407668974822819,
3.49237575473668));
#51116=CARTESIAN_POINT('Ctrl Pts',(13.9665224248064,-0.117871845784803,
3.35970116712309));
#51117=CARTESIAN_POINT('Ctrl Pts',(13.9901365409563,0.200174091641329,3.38047865214521));
#51118=CARTESIAN_POINT('Ctrl Pts',(14.0137506571061,0.470246914526057,3.54972874087838));
#51119=CARTESIAN_POINT('Ctrl Pts',(14.037364773256,0.627621790796785,3.82688947135059));
#51120=CARTESIAN_POINT('Ctrl Pts',(14.0609788894059,0.634582735815489,4.14553734509456));
#51121=CARTESIAN_POINT('Ctrl Pts',(14.0845930055557,0.489461510650943,4.42930618095194));
#51122=CARTESIAN_POINT('Ctrl Pts',(14.1060049423205,0.251510284961593,4.59332024860173));
#51123=CARTESIAN_POINT('Ctrl Pts',(14.1195455070353,0.074198300926532,4.62491679006221));
#51124=CARTESIAN_POINT('Ctrl Pts',(14.1252146997001,-1.50974863141889E-5,
4.62498583382255));
#51125=CARTESIAN_POINT('Ctrl Pts',(13.7247853002999,-1.20831421156938E-5,
4.62503091248755));
#51126=CARTESIAN_POINT('Ctrl Pts',(13.7258348801309,-0.013748904810447,
4.62504304225186));
#51127=CARTESIAN_POINT('Ctrl Pts',(13.734755832012,-0.130498998332177,4.62127102305724));
#51128=CARTESIAN_POINT('Ctrl Pts',(13.7515481559429,-0.346119716157775,
4.55143222859795));
#51129=CARTESIAN_POINT('Ctrl Pts',(13.7751622720928,-0.566385203513325,
4.32106722332061));
#51130=CARTESIAN_POINT('Ctrl Pts',(13.7987763882427,-0.650912534047929,
4.01375622291695));
#51131=CARTESIAN_POINT('Ctrl Pts',(13.8223905043925,-0.57944414457563,3.70314844792952));
#51132=CARTESIAN_POINT('Ctrl Pts',(13.8460046205424,-0.369107932149097,
3.46368321387984));
#51133=CARTESIAN_POINT('Ctrl Pts',(13.8696187366923,-0.0703124342978696,
3.35275003110641));
#51134=CARTESIAN_POINT('Ctrl Pts',(13.8932328528421,0.245333927901481,3.3969348091043));
#51135=CARTESIAN_POINT('Ctrl Pts',(13.916846968992,0.502184306426786,3.58564835824111));
#51136=CARTESIAN_POINT('Ctrl Pts',(13.9404610851419,0.638682720042094,3.87366416276737));
#51137=CARTESIAN_POINT('Ctrl Pts',(13.9640752012917,0.62211637371287,4.19195723015293));
#51138=CARTESIAN_POINT('Ctrl Pts',(13.9876893174416,0.456455507660852,4.46424641105313));
#51139=CARTESIAN_POINT('Ctrl Pts',(14.007926017111,0.220741531225703,4.60224444133776));
#51140=CARTESIAN_POINT('Ctrl Pts',(14.0202913447304,0.058831122868106,4.62493198618401));
#51141=CARTESIAN_POINT('Ctrl Pts',(14.0247853002999,-6.39660293913491E-6,
4.62495348172753));
#51142=CARTESIAN_POINT('Origin',(11.8752146997001,0.,4.));
#51143=CARTESIAN_POINT('',(13.4247853002999,1.36962628664028E-5,4.62502243215823));
#51144=CARTESIAN_POINT('',(13.5252146997001,1.40828270379035E-5,4.62497680637469));
#51145=CARTESIAN_POINT('',(11.8752146997001,-1.68747709936658E-14,4.625));
#51146=CARTESIAN_POINT('Ctrl Pts',(13.5252146997001,1.4082827037902E-5,
4.62497680637469));
#51147=CARTESIAN_POINT('Ctrl Pts',(13.5306325778363,-0.0709123884867814,
4.62491668074428));
#51148=CARTESIAN_POINT('Ctrl Pts',(13.5439218280225,-0.244933372371362,
4.59533688876844));
#51149=CARTESIAN_POINT('Ctrl Pts',(13.5650824502587,-0.482621788093898,
4.43698120905743));
#51150=CARTESIAN_POINT('Ctrl Pts',(13.5886965664085,-0.632205603168059,
4.15553919999523));
#51151=CARTESIAN_POINT('Ctrl Pts',(13.6123106825584,-0.630276944445953,
3.83682113889318));
#51152=CARTESIAN_POINT('Ctrl Pts',(13.6359247987083,-0.477298028416376,
3.55721002779864));
#51153=CARTESIAN_POINT('Ctrl Pts',(13.6595389148582,-0.209931317243796,
3.38371661595291));
#51154=CARTESIAN_POINT('Ctrl Pts',(13.683153031008,0.107746895509167,3.35791980725116));
#51155=CARTESIAN_POINT('Ctrl Pts',(13.7067671471579,0.399602814690774,3.48600198647908));
#51156=CARTESIAN_POINT('Ctrl Pts',(13.7303812633077,0.59569113756138,3.73726736776131));
#51157=CARTESIAN_POINT('Ctrl Pts',(13.7539953794576,0.649017932507905,4.05149845333026));
#51158=CARTESIAN_POINT('Ctrl Pts',(13.7776094956075,0.546803061895555,4.35338757606046));
#51159=CARTESIAN_POINT('Ctrl Pts',(13.8012236117573,0.313543031018869,4.57058490613733));
#51160=CARTESIAN_POINT('Ctrl Pts',(13.8170920131216,0.106300066848774,4.6246481407235));
#51161=CARTESIAN_POINT('Ctrl Pts',(13.8250890424358,0.00164611344283092,
4.62505264870678));
#51162=CARTESIAN_POINT('Ctrl Pts',(13.8252146997001,1.68461488569581E-6,
4.62505238998457));
#51163=CARTESIAN_POINT('Ctrl Pts',(13.4247853002999,1.36962628664097E-5,
4.62502243215823));
#51164=CARTESIAN_POINT('Ctrl Pts',(13.4313784155315,-0.086279884022628,
4.62493973056585));
#51165=CARTESIAN_POINT('Ctrl Pts',(13.445842902813,-0.275670893367246,4.58538934244717));
#51166=CARTESIAN_POINT('Ctrl Pts',(13.4681787621445,-0.513544980480383,
4.40018484937968));
#51167=CARTESIAN_POINT('Ctrl Pts',(13.4917928782944,-0.64195771209056,4.10847422061066));
#51168=CARTESIAN_POINT('Ctrl Pts',(13.5154069944443,-0.616520809113462,
3.79076698974655));
#51169=CARTESIAN_POINT('Ctrl Pts',(13.5390211105941,-0.443330402422436,
3.52320390633144));
#51170=CARTESIAN_POINT('Ctrl Pts',(13.562635226744,-0.163892778617988,3.36990832590288));
#51171=CARTESIAN_POINT('Ctrl Pts',(13.5862493428939,0.154822890495328,3.36761860145296));
#51172=CARTESIAN_POINT('Ctrl Pts',(13.6098634590437,0.43643417612693,3.51688348138565));
#51173=CARTESIAN_POINT('Ctrl Pts',(13.6334775751936,0.613450973283793,3.78193059814177));
#51174=CARTESIAN_POINT('Ctrl Pts',(13.6570916913435,0.643449974253473,4.09923956510808));
#51175=CARTESIAN_POINT('Ctrl Pts',(13.6807058074933,0.519241709620395,4.39276507945606));
#51176=CARTESIAN_POINT('Ctrl Pts',(13.7032703438121,0.281645253009076,4.58329909926801));
#51177=CARTESIAN_POINT('Ctrl Pts',(13.717963508081,0.0892710189108511,4.62495207452848));
#51178=CARTESIAN_POINT('Ctrl Pts',(13.7247853002999,-1.20831421156938E-5,
4.62503091248755));
#51179=CARTESIAN_POINT('Origin',(11.8752146997001,0.,4.));
#51180=CARTESIAN_POINT('',(13.1247853002999,3.84888821539087E-6,4.62495078081483));
#51181=CARTESIAN_POINT('',(13.2252146997001,-9.32440196476731E-6,4.62495874418382));
#51182=CARTESIAN_POINT('',(11.8752146997001,-1.68747709936658E-14,4.625));
#51183=CARTESIAN_POINT('Ctrl Pts',(13.2252146997001,-9.32440196474427E-6,
4.62495874418382));
#51184=CARTESIAN_POINT('Ctrl Pts',(13.2283047411869,-0.040464997295585,
4.62498052751194));
#51185=CARTESIAN_POINT('Ctrl Pts',(13.2392661547237,-0.18396024524725,4.61125364372682));
#51186=CARTESIAN_POINT('Ctrl Pts',(13.2580989403104,-0.413782468289504,
4.50265339583901));
#51187=CARTESIAN_POINT('Ctrl Pts',(13.2817130564603,-0.602786876612853,
4.24601696851145));
#51188=CARTESIAN_POINT('Ctrl Pts',(13.3053271726101,-0.647329213752593,
3.9304208620728));
#51189=CARTESIAN_POINT('Ctrl Pts',(13.32894128876,-0.536734598538914,3.6314998804023));
#51190=CARTESIAN_POINT('Ctrl Pts',(13.3525554049099,-0.297507800394296,
3.42089251764738));
#51191=CARTESIAN_POINT('Ctrl Pts',(13.3761695210598,0.0130188131672444,
3.34907229440132));
#51192=CARTESIAN_POINT('Ctrl Pts',(13.3997836372096,0.320425377524893,3.43325142712992));
#51193=CARTESIAN_POINT('Ctrl Pts',(13.4233977533595,0.551039769569266,3.65325580067535));
#51194=CARTESIAN_POINT('Ctrl Pts',(13.4470118695093,0.649593644862141,3.95635983539258));
#51195=CARTESIAN_POINT('Ctrl Pts',(13.4706259856592,0.592467881122722,4.26992253935193));
#51196=CARTESIAN_POINT('Ctrl Pts',(13.4942401018091,0.393353065302923,4.5187964277335));
#51197=CARTESIAN_POINT('Ctrl Pts',(13.5124363398227,0.1672808180195,4.61476328251587));
#51198=CARTESIAN_POINT('Ctrl Pts',(13.5227612057864,0.0321332374692893,
4.62500403435298));
#51199=CARTESIAN_POINT('Ctrl Pts',(13.5252146997001,1.4082827037902E-5,
4.62497680637469));
#51200=CARTESIAN_POINT('Ctrl Pts',(13.1247853002999,3.84888821536311E-6,
4.62495078081483));
#51201=CARTESIAN_POINT('Ctrl Pts',(13.1290505788821,-0.0558403875021823,
4.6249385719914));
#51202=CARTESIAN_POINT('Ctrl Pts',(13.1411872295142,-0.214751600407627,
4.60383286368317));
#51203=CARTESIAN_POINT('Ctrl Pts',(13.1611952521963,-0.449738236712957,
4.47075670902068));
#51204=CARTESIAN_POINT('Ctrl Pts',(13.1848093683461,-0.619294173608025,
4.2008758003961));
#51205=CARTESIAN_POINT('Ctrl Pts',(13.208423484496,-0.64043195068177,3.88285360784221));
#51206=CARTESIAN_POINT('Ctrl Pts',(13.2320376006459,-0.508085752511173,
3.59290636366459));
#51207=CARTESIAN_POINT('Ctrl Pts',(13.2556517167957,-0.253973266794505,
3.40052194335125));
#51208=CARTESIAN_POINT('Ctrl Pts',(13.2792658329456,0.0610056803032868,
3.3518066124833));
#51209=CARTESIAN_POINT('Ctrl Pts',(13.3028799490955,0.361364191435218,3.45843533922715));
#51210=CARTESIAN_POINT('Ctrl Pts',(13.3264940652453,0.575119258511334,3.69485380694));
#51211=CARTESIAN_POINT('Ctrl Pts',(13.3501081813952,0.65104299168552,4.00440268404554));
#51212=CARTESIAN_POINT('Ctrl Pts',(13.3737222975451,0.570939739771795,4.31289642727099));
#51213=CARTESIAN_POINT('Ctrl Pts',(13.3973364136949,0.354006804717113,4.54640236352309));
#51214=CARTESIAN_POINT('Ctrl Pts',(13.4143574146132,0.136489422610972,4.62032507485564));
#51215=CARTESIAN_POINT('Ctrl Pts',(13.4235070434815,0.0167440814458925,
4.62503846613771));
#51216=CARTESIAN_POINT('Ctrl Pts',(13.4247853002999,1.36962628664097E-5,
4.62502243215823));
#51217=CARTESIAN_POINT('Origin',(11.8752146997001,0.,4.));
#51218=CARTESIAN_POINT('',(12.8247853002999,-1.55438223423121E-5,4.62499607812274));
#51219=CARTESIAN_POINT('',(12.9252146997001,-9.4222586321007E-6,4.62504029123831));
#51220=CARTESIAN_POINT('',(11.8752146997001,-1.68747709936658E-14,4.625));
#51221=CARTESIAN_POINT('Ctrl Pts',(12.9252146997001,-9.42225863212465E-6,
4.62504029123832));
#51222=CARTESIAN_POINT('Ctrl Pts',(12.9259769045375,-0.00998466834883174,
4.6250476064301));
#51223=CARTESIAN_POINT('Ctrl Pts',(12.9346104814248,-0.122971475467856,
4.62239759066569));
#51224=CARTESIAN_POINT('Ctrl Pts',(12.9511154303622,-0.336107011072318,
4.55759164674784));
#51225=CARTESIAN_POINT('Ctrl Pts',(12.974729546512,-0.56049590900091,4.33124115596169));
#51226=CARTESIAN_POINT('Ctrl Pts',(12.9983436626619,-0.650558060547343,
4.02550641626558));
#51227=CARTESIAN_POINT('Ctrl Pts',(13.0219577788117,-0.584709444123524,
3.71365888635357));
#51228=CARTESIAN_POINT('Ctrl Pts',(13.0455718949616,-0.378731139057797,
3.47043499764384));
#51229=CARTESIAN_POINT('Ctrl Pts',(13.0691860111115,-0.0819872800401352,
3.35412504823007));
#51230=CARTESIAN_POINT('Ctrl Pts',(13.0928001272613,0.234405401379786,3.39260352716186));
#51231=CARTESIAN_POINT('Ctrl Pts',(13.1164142434112,0.494621196584012,3.57664879910166));
#51232=CARTESIAN_POINT('Ctrl Pts',(13.1400283595611,0.636297578801308,3.86215313342763));
#51233=CARTESIAN_POINT('Ctrl Pts',(13.1636424757109,0.625480816776257,4.18069342892634));
#51234=CARTESIAN_POINT('Ctrl Pts',(13.1872565918608,0.464763222827219,4.45592928631477));
#51235=CARTESIAN_POINT('Ctrl Pts',(13.2077806665239,0.228267895462889,4.60018049807294));
#51236=CARTESIAN_POINT('Ctrl Pts',(13.220433369137,0.0625891701764018,4.62492503806923));
#51237=CARTESIAN_POINT('Ctrl Pts',(13.2252146997001,-9.32440196474427E-6,
4.62495874418382));
#51238=CARTESIAN_POINT('Ctrl Pts',(12.8247853002999,-1.55438223423052E-5,
4.62499607812274));
#51239=CARTESIAN_POINT('Ctrl Pts',(12.8267227422326,-0.0253767156259869,
4.62502109614712));
#51240=CARTESIAN_POINT('Ctrl Pts',(12.8365315562153,-0.153759343851268,
4.61735081595804));
#51241=CARTESIAN_POINT('Ctrl Pts',(12.854211742248,-0.376327535803878,4.5312757721487));
#51242=CARTESIAN_POINT('Ctrl Pts',(12.8778258583979,-0.583405888470749,
4.28898776831928));
#51243=CARTESIAN_POINT('Ctrl Pts',(12.9014399745477,-0.650666957548692,
3.97744183415536));
#51244=CARTESIAN_POINT('Ctrl Pts',(12.9250540906976,-0.561991161265395,
3.67130212143154));
#51245=CARTESIAN_POINT('Ctrl Pts',(12.9486682068475,-0.338630270727757,
3.44393714350224));
#51246=CARTESIAN_POINT('Ctrl Pts',(12.9722823229973,-0.0341142786054444,
3.34983650006563));
#51247=CARTESIAN_POINT('Ctrl Pts',(12.9958964391472,0.278577437919422,3.41155206540036));
#51248=CARTESIAN_POINT('Ctrl Pts',(13.0195105552971,0.524506132150044,3.61429327464512));
#51249=CARTESIAN_POINT('Ctrl Pts',(13.0431246714469,0.644733280558021,3.90947178565704));
#51250=CARTESIAN_POINT('Ctrl Pts',(13.0667387875968,0.61044561006836,4.22634601343335));
#51251=CARTESIAN_POINT('Ctrl Pts',(13.0903529037467,0.429860399609997,4.4889748434194));
#51252=CARTESIAN_POINT('Ctrl Pts',(13.1097017413144,0.197481915229314,4.60814700801091));
#51253=CARTESIAN_POINT('Ctrl Pts',(13.1211792068321,0.0472175377905832,
4.6249611028038));
#51254=CARTESIAN_POINT('Ctrl Pts',(13.1247853002999,3.84888821536311E-6,
4.62495078081483));
#51255=CARTESIAN_POINT('Origin',(11.8752146997001,0.,4.));
#51256=CARTESIAN_POINT('',(12.5247853002999,3.80998376854277E-6,4.62503871776264));
#51257=CARTESIAN_POINT('',(12.6252146997001,1.49489494596481E-5,4.6250110476872));
#51258=CARTESIAN_POINT('',(11.8752146997001,-1.68747709936658E-14,4.625));
#51259=CARTESIAN_POINT('',(12.5,0.310062960217711,4.54266560670548));
#51260=CARTESIAN_POINT('Ctrl Pts',(12.5,0.310062960217722,4.54266560670548));
#51261=CARTESIAN_POINT('Ctrl Pts',(12.50787137205,0.220600394030941,4.59378185169648));
#51262=CARTESIAN_POINT('Ctrl Pts',(12.5161331388166,0.113220056708515,4.6237347594226));
#51263=CARTESIAN_POINT('Ctrl Pts',(12.5243949055832,0.00511234815255113,
4.6250406321328));
#51264=CARTESIAN_POINT('Ctrl Pts',(12.5247853002999,3.80998376856706E-6,
4.62503871776264));
#51265=CARTESIAN_POINT('',(12.5,0.310062960217774,3.45733439329455));
#51266=CARTESIAN_POINT('Origin',(12.5,0.,4.));
#51267=CARTESIAN_POINT('Ctrl Pts',(12.5,0.310093463203755,3.45730861053195));
#51268=CARTESIAN_POINT('Ctrl Pts',(12.5008157411716,0.319367492808711,3.46259780682489));
#51269=CARTESIAN_POINT('Ctrl Pts',(12.5095028543931,0.416666480413896,3.52147574364868));
#51270=CARTESIAN_POINT('Ctrl Pts',(12.5260613396645,0.569511032758309,3.68451895614546));
#51271=CARTESIAN_POINT('Ctrl Pts',(12.5496754558144,0.651018771792273,3.99264764559437));
#51272=CARTESIAN_POINT('Ctrl Pts',(12.5732895719643,0.576495013506714,4.3025367374363));
#51273=CARTESIAN_POINT('Ctrl Pts',(12.5969036881141,0.363815091701307,4.53992168461618));
#51274=CARTESIAN_POINT('Ctrl Pts',(12.6142120640261,0.144017971622128,4.61907377583531));
#51275=CARTESIAN_POINT('Ctrl Pts',(12.6236490678881,0.0205077016108913,
4.62503160004571));
#51276=CARTESIAN_POINT('Ctrl Pts',(12.6252146997001,1.49489494596471E-5,
4.6250110476872));
#51277=CARTESIAN_POINT('Origin',(11.8752146997001,0.,4.));
#51278=CARTESIAN_POINT('Ctrl Pts',(12.6252146997001,1.49489494596471E-5,
4.6250110476872));
#51279=CARTESIAN_POINT('Ctrl Pts',(12.631520439938,-0.0825216819810338,
4.62492827098767));
#51280=CARTESIAN_POINT('Ctrl Pts',(12.6456975522259,-0.268159494659544,
4.5879440580038));
#51281=CARTESIAN_POINT('Ctrl Pts',(12.6677460365637,-0.506235857616531,
4.40939182910775));
#51282=CARTESIAN_POINT('Ctrl Pts',(12.6913601527136,-0.639894509617229,
4.12004729681268));
#51283=CARTESIAN_POINT('Ctrl Pts',(12.7149742688635,-0.620198095551099,
3.8019325752266));
#51284=CARTESIAN_POINT('Ctrl Pts',(12.7385883850133,-0.451866840211785,
3.53128609963859));
#51285=CARTESIAN_POINT('Ctrl Pts',(12.7622025011632,-0.17524257447904,3.37297016902465));
#51286=CARTESIAN_POINT('Ctrl Pts',(12.7858166173131,0.143379805101228,3.36492630429559));
#51287=CARTESIAN_POINT('Ctrl Pts',(12.809430733463,0.42764021116234,3.50908227080648));
#51288=CARTESIAN_POINT('Ctrl Pts',(12.8330448496128,0.609413666055986,3.77089008898231));
#51289=CARTESIAN_POINT('Ctrl Pts',(12.8566589657627,0.645136892431096,4.08760569204938));
#51290=CARTESIAN_POINT('Ctrl Pts',(12.8802730819125,0.526248572038732,4.38332598125533));
#51291=CARTESIAN_POINT('Ctrl Pts',(12.903124993225,0.289149347937084,4.5805996458561));
#51292=CARTESIAN_POINT('Ctrl Pts',(12.9181055324875,0.0930307802739178,
4.62497206165088));
#51293=CARTESIAN_POINT('Ctrl Pts',(12.9252146997001,-9.42225863212465E-6,
4.62504029123832));
#51294=CARTESIAN_POINT('Ctrl Pts',(12.5247853002999,3.80998376856706E-6,
4.62503871776264));
#51295=CARTESIAN_POINT('Ctrl Pts',(12.5322662776332,-0.0978890574527522,
4.62500203345524));
#51296=CARTESIAN_POINT('Ctrl Pts',(12.5476186270164,-0.298862923743373,
4.57698368148067));
#51297=CARTESIAN_POINT('Ctrl Pts',(12.5708423484496,-0.535054221536356,
4.37092866956447));
#51298=CARTESIAN_POINT('Ctrl Pts',(12.5944564645995,-0.647009713430093,
4.07251155115386));
#51299=CARTESIAN_POINT('Ctrl Pts',(12.6180705807493,-0.603894380709874,
3.75671714932517));
#51300=CARTESIAN_POINT('Ctrl Pts',(12.6416846968992,-0.416056506175611,
3.49922677321964));
#51301=CARTESIAN_POINT('Ctrl Pts',(12.6652988130491,-0.128505496873939,
3.36175035317655));
#51302=CARTESIAN_POINT('Ctrl Pts',(12.6889129291989,0.189841674427298,3.37723482234205));
#51303=CARTESIAN_POINT('Ctrl Pts',(12.7125270453488,0.462692468193658,3.54196933898577));
#51304=CARTESIAN_POINT('Ctrl Pts',(12.7361411614987,0.624655556881011,3.81647407445394));
#51305=CARTESIAN_POINT('Ctrl Pts',(12.7597552776485,0.636915702199809,4.13496208375113));
#51306=CARTESIAN_POINT('Ctrl Pts',(12.7833693937984,0.496534514683115,4.42110548633398));
#51307=CARTESIAN_POINT('Ctrl Pts',(12.8050460680155,0.258436396781676,4.5911312751119));
#51308=CARTESIAN_POINT('Ctrl Pts',(12.8188513701827,0.0776597756952025,
4.62491945378327));
#51309=CARTESIAN_POINT('Ctrl Pts',(12.8247853002999,-1.55438223423052E-5,
4.62499607812274));
#51310=CARTESIAN_POINT('Ctrl Pts',(12.5,-0.186196943290592,3.58169363627332));
#51311=CARTESIAN_POINT('Ctrl Pts',(12.50787137205,-0.117235947257613,3.55099764935784));
#51312=CARTESIAN_POINT('Ctrl Pts',(12.5236141161499,0.0360970477778841,
3.52440632583991));
#51313=CARTESIAN_POINT('Ctrl Pts',(12.5472282322997,0.257537368848111,3.59853698535937));
#51314=CARTESIAN_POINT('Ctrl Pts',(12.5708423484496,0.417223782598737,3.76887858727216));
#51315=CARTESIAN_POINT('Ctrl Pts',(12.5944564645995,0.476936352215019,3.99461366516243));
#51316=CARTESIAN_POINT('Ctrl Pts',(12.6180705807493,0.422340246895018,4.22163841384584));
#51317=CARTESIAN_POINT('Ctrl Pts',(12.6416846968992,0.266530936180377,4.39554662614981));
#51318=CARTESIAN_POINT('Ctrl Pts',(12.6652988130491,0.0468439715927196,
4.47465904879863));
#51319=CARTESIAN_POINT('Ctrl Pts',(12.6889129291989,-0.184068700558194,
4.44001626345752));
#51320=CARTESIAN_POINT('Ctrl Pts',(12.7125270453488,-0.37086838928987,4.29992045400434));
#51321=CARTESIAN_POINT('Ctrl Pts',(12.7361411614987,-0.468786717745582,
4.08794664964497));
#51322=CARTESIAN_POINT('Ctrl Pts',(12.7597552776485,-0.454357124800734,
3.85489580461101));
#51323=CARTESIAN_POINT('Ctrl Pts',(12.7833693937984,-0.331037647139153,
3.65662019659523));
#51324=CARTESIAN_POINT('Ctrl Pts',(12.8069835099483,-0.128382710063344,
3.54063794582746));
#51325=CARTESIAN_POINT('Ctrl Pts',(12.8305976260981,0.10504004521716,3.53474501052695));
#51326=CARTESIAN_POINT('Ctrl Pts',(12.854211742248,0.31328921869753,3.64035367159283));
#51327=CARTESIAN_POINT('Ctrl Pts',(12.8778258583979,0.446456451752615,3.83215407918844));
#51328=CARTESIAN_POINT('Ctrl Pts',(12.9014399745477,0.47262728739502,4.06417992999538));
#51329=CARTESIAN_POINT('Ctrl Pts',(12.9250540906976,0.385529703875575,4.28082461386765));
#51330=CARTESIAN_POINT('Ctrl Pts',(12.9486682068475,0.206037242841946,4.43016772408018));
#51331=CARTESIAN_POINT('Ctrl Pts',(12.9722823229973,-0.0228334776507366,
4.47641814468844));
#51332=CARTESIAN_POINT('Ctrl Pts',(12.9958964391472,-0.24623199631158,4.40849164040747));
#51333=CARTESIAN_POINT('Ctrl Pts',(13.0195105552971,-0.410619302934066,
4.24266727085754));
#51334=CARTESIAN_POINT('Ctrl Pts',(13.0431246714469,-0.476598835156983,
4.01868600055616));
#51335=CARTESIAN_POINT('Ctrl Pts',(13.0667387875968,-0.428358138764893,
3.79022650014263));
#51336=CARTESIAN_POINT('Ctrl Pts',(13.0903529037467,-0.277458432473742,
3.61204067927388));
#51337=CARTESIAN_POINT('Ctrl Pts',(13.1139670198965,-0.060063881357403,
3.52683201033335));
#51338=CARTESIAN_POINT('Ctrl Pts',(13.1375811360464,0.171725397050831,3.55502134399878));
#51339=CARTESIAN_POINT('Ctrl Pts',(13.1611952521963,0.362359488617447,3.68985291022187));
#51340=CARTESIAN_POINT('Ctrl Pts',(13.1848093683461,0.466151606229838,3.89901338554908));
#51341=CARTESIAN_POINT('Ctrl Pts',(13.208423484496,0.458227246370285,4.13237600603144));
#51342=CARTESIAN_POINT('Ctrl Pts',(13.2320376006459,0.34048553704322,4.3340137951542));
#51343=CARTESIAN_POINT('Ctrl Pts',(13.2556517167957,0.141144098528766,4.45560285308526));
#51344=CARTESIAN_POINT('Ctrl Pts',(13.2792658329456,-0.0920235057499227,
4.46800351566886));
#51345=CARTESIAN_POINT('Ctrl Pts',(13.3028799490955,-0.30313703626889,4.36824387779166));
#51346=CARTESIAN_POINT('Ctrl Pts',(13.3264940652453,-0.441601665806575,
4.18023203113149));
#51347=CARTESIAN_POINT('Ctrl Pts',(13.3501081813952,-0.47423338199515,3.94902632355453));
#51348=CARTESIAN_POINT('Ctrl Pts',(13.3737222975451,-0.393211766889608,
3.73003681238273));
#51349=CARTESIAN_POINT('Ctrl Pts',(13.3973364136949,-0.217954214568861,
3.57574585842847));
#51350=CARTESIAN_POINT('Ctrl Pts',(13.4209505298448,0.00953758252632317,
3.52313036287841));
#51351=CARTESIAN_POINT('Ctrl Pts',(13.4445646459947,0.234743631574736,3.58479999551538));
#51352=CARTESIAN_POINT('Ctrl Pts',(13.4681787621445,0.403691735186444,3.74597519957476));
#51353=CARTESIAN_POINT('Ctrl Pts',(13.4917928782944,0.475892304226004,3.96802921540861));
#51354=CARTESIAN_POINT('Ctrl Pts',(13.5154069944443,0.434041969710506,4.19774525232923));
#51355=CARTESIAN_POINT('Ctrl Pts',(13.5390211105941,0.288170455640921,4.38007026295756));
#51356=CARTESIAN_POINT('Ctrl Pts',(13.562635226744,0.0732368858249759,4.47130878927046));
#51357=CARTESIAN_POINT('Ctrl Pts',(13.5862493428939,-0.159248413505658,
4.44959488329479));
#51358=CARTESIAN_POINT('Ctrl Pts',(13.6098634590437,-0.353568721957589,
4.32013243375547));
#51359=CARTESIAN_POINT('Ctrl Pts',(13.6334775751936,-0.46315382488092,4.1139480179165));
#51360=CARTESIAN_POINT('Ctrl Pts',(13.6570916913435,-0.461740889501104,
3.88045516635315));
#51361=CARTESIAN_POINT('Ctrl Pts',(13.6807058074933,-0.349668535617837,
3.67561206636528));
#51362=CARTESIAN_POINT('Ctrl Pts',(13.7043199236432,-0.153795683012805,
3.5485107928471));
#51363=CARTESIAN_POINT('Ctrl Pts',(13.7279340397931,0.0789353756500159,
3.5296120507922));
#51364=CARTESIAN_POINT('Ctrl Pts',(13.7515481559429,0.292749022042461,3.62344505529457));
#51365=CARTESIAN_POINT('Ctrl Pts',(13.7751622720928,0.436403327377467,3.80752207362193));
#51366=CARTESIAN_POINT('Ctrl Pts',(13.7987763882427,0.475470537355291,4.03772776690975));
#51367=CARTESIAN_POINT('Ctrl Pts',(13.8223905043925,0.400587923144683,4.25889173822189));
#51368=CARTESIAN_POINT('Ctrl Pts',(13.8460046205424,0.229701624524423,4.41801050223621));
#51369=CARTESIAN_POINT('Ctrl Pts',(13.8696187366923,0.00376573255618155,
4.47695013947711));
#51370=CARTESIAN_POINT('Ctrl Pts',(13.8932328528421,-0.223072643433687,
4.42158535558109));
#51371=CARTESIAN_POINT('Ctrl Pts',(13.916846968992,-0.396450107540549,4.26518470642179));
#51372=CARTESIAN_POINT('Ctrl Pts',(13.9404610851419,-0.474815543552022,
4.04523069632808));
#51373=CARTESIAN_POINT('Ctrl Pts',(13.9640752012917,-0.439388129199652,
3.81443683499316));
#51374=CARTESIAN_POINT('Ctrl Pts',(13.9876893174416,-0.298658290955197,
3.62811447792009));
#51375=CARTESIAN_POINT('Ctrl Pts',(14.0113034335915,-0.0863529142219465,
3.53091707503438));
#51376=CARTESIAN_POINT('Ctrl Pts',(14.0349175497413,0.146647539536438,3.54613866056158));
#51377=CARTESIAN_POINT('Ctrl Pts',(14.0585316658912,0.344502889581789,3.6701312755675));
#51378=CARTESIAN_POINT('Ctrl Pts',(14.0821457820411,0.459795723937725,3.87317922671144));
#51379=CARTESIAN_POINT('Ctrl Pts',(14.1057598981909,0.464895312258427,4.10662065901627));
#51380=CARTESIAN_POINT('Ctrl Pts',(14.1293740143408,0.358579502702881,4.31450970816539));
#51381=CARTESIAN_POINT('Ctrl Pts',(14.1529881304907,0.166327619131383,4.44702431634421));
#51382=CARTESIAN_POINT('Ctrl Pts',(14.1766022466405,-0.0657858362277661,
4.47240643522367));
#51383=CARTESIAN_POINT('Ctrl Pts',(14.2002163627904,-0.282133257977474,
4.38457306332079));
#51384=CARTESIAN_POINT('Ctrl Pts',(14.2238304789403,-0.430865480427841,
4.20457407964992));
#51385=CARTESIAN_POINT('Ctrl Pts',(14.2474445950901,-0.476337791093329,
3.97554749368157));
#51386=CARTESIAN_POINT('Ctrl Pts',(14.27105871124,-0.407652434174819,3.75238112107461));
#51387=CARTESIAN_POINT('Ctrl Pts',(14.2946728273899,-0.241270333599833,
3.58855833656088));
#51388=CARTESIAN_POINT('Ctrl Pts',(14.3182869435397,-0.0170661180132474,
3.52334041087493));
#51389=CARTESIAN_POINT('Ctrl Pts',(14.3419010596896,0.211228111558234,3.57235727391142));
#51390=CARTESIAN_POINT('Ctrl Pts',(14.3655151758395,0.388900053764453,3.72386169322071));
#51391=CARTESIAN_POINT('Ctrl Pts',(14.3891292919893,0.473369390821204,3.94154458004181));
#51392=CARTESIAN_POINT('Ctrl Pts',(14.4127434081392,0.444392458083208,4.17323671518384));
#51393=CARTESIAN_POINT('Ctrl Pts',(14.4363575242891,0.308913779199362,4.3634114655727));
#51394=CARTESIAN_POINT('Ctrl Pts',(14.4599716404389,0.0994017626770733,
4.46649212840691));
#51395=CARTESIAN_POINT('Ctrl Pts',(14.4835857565888,-0.133932578240045,
4.45777470525894));
#51396=CARTESIAN_POINT('Ctrl Pts',(14.5071998727387,-0.335169044432007,
4.33934838727104));
#51397=CARTESIAN_POINT('Ctrl Pts',(14.5308139888885,-0.456079915900645,
4.13959486595487));
#51398=CARTESIAN_POINT('Ctrl Pts',(14.5544281050384,-0.467688060597361,
3.90638646324521));
#51399=CARTESIAN_POINT('Ctrl Pts',(14.5780422211883,-0.367211505836647,
3.69561319629505));
#51400=CARTESIAN_POINT('Ctrl Pts',(14.6016563373381,-0.178730157419731,
3.55778834579073));
#51401=CARTESIAN_POINT('Ctrl Pts',(14.625270453488,0.0525851174261518,3.52594259660587));
#51402=CARTESIAN_POINT('Ctrl Pts',(14.6488845696379,0.271298002813252,3.60770800421126));
#51403=CARTESIAN_POINT('Ctrl Pts',(14.6724986857877,0.424992433239313,3.78348891949988));
#51404=CARTESIAN_POINT('Ctrl Pts',(14.6961128019376,0.476834468501385,4.01115822240469));
#51405=CARTESIAN_POINT('Ctrl Pts',(14.7197269180875,0.414399804028447,4.23615337970372));
#51406=CARTESIAN_POINT('Ctrl Pts',(14.7433410342373,0.252651341641402,4.40455273546398));
#51407=CARTESIAN_POINT('Ctrl Pts',(14.7669551503872,0.0303532266559796,
4.47599821226155));
#51408=CARTESIAN_POINT('Ctrl Pts',(14.7905692665371,-0.199219250862459,
4.43336740322118));
#51409=CARTESIAN_POINT('Ctrl Pts',(14.8141833826869,-0.381047447081096,
4.28687708064914));
#51410=CARTESIAN_POINT('Ctrl Pts',(14.8377974988368,-0.471554972144783,
4.07163466550741));
#51411=CARTESIAN_POINT('Ctrl Pts',(14.8614116149867,-0.449051060899263,
3.83922451083896));
#51412=CARTESIAN_POINT('Ctrl Pts',(14.8850257311365,-0.318928946727196,
3.64534530693059));
#51413=CARTESIAN_POINT('Ctrl Pts',(14.9086398472864,-0.112373269271187,
3.53646160000302));
#51414=CARTESIAN_POINT('Ctrl Pts',(14.9322539634362,0.121113399391719,3.5386680312482));
#51415=CARTESIAN_POINT('Ctrl Pts',(14.9558680795861,0.325574495333277,3.65143602219853));
#51416=CARTESIAN_POINT('Ctrl Pts',(14.979482195736,0.452009190454857,3.84773949289016));
#51417=CARTESIAN_POINT('Ctrl Pts',(15.0030963118858,0.470117180575255,4.08053390545391));
#51418=CARTESIAN_POINT('Ctrl Pts',(15.0267104280357,0.375557372208547,4.29402641177155));
#51419=CARTESIAN_POINT('Ctrl Pts',(15.0503245441856,0.190994688421392,4.43705643304037));
#51420=CARTESIAN_POINT('Ctrl Pts',(15.0739386603355,-0.0393454023191647,
4.47533644032795));
#51421=CARTESIAN_POINT('Ctrl Pts',(15.0975527764853,-0.260245916509526,
4.39971253597763));
#51422=CARTESIAN_POINT('Ctrl Pts',(15.1211668926352,-0.418792603204267,
4.22826540530875));
#51423=CARTESIAN_POINT('Ctrl Pts',(15.1369096367351,-0.457530945318996,
4.07754232577813));
#51424=CARTESIAN_POINT('Ctrl Pts',(15.1447810087851,-0.457870370902723,
4.00205890126089));
#51425=CARTESIAN_POINT('Ctrl Pts',(12.4850729970717,-0.208850989443975,
3.53079950502365));
#51426=CARTESIAN_POINT('Ctrl Pts',(12.4929443691216,-0.131499707516366,
3.49636882573344));
#51427=CARTESIAN_POINT('Ctrl Pts',(12.5086871132215,0.0404888716816997,
3.46654221242176));
#51428=CARTESIAN_POINT('Ctrl Pts',(12.5323012293714,0.288871199237585,3.54969213591223));
#51429=CARTESIAN_POINT('Ctrl Pts',(12.5559153455212,0.467986199318594,3.74075871022993));
#51430=CARTESIAN_POINT('Ctrl Pts',(12.5795294616711,0.534963825407437,3.99395832530641));
#51431=CARTESIAN_POINT('Ctrl Pts',(12.603143577821,0.473725169098917,4.24860452170932));
#51432=CARTESIAN_POINT('Ctrl Pts',(12.6267576939708,0.298958988020687,4.4436716456386));
#51433=CARTESIAN_POINT('Ctrl Pts',(12.6503718101207,0.0525433427838623,
4.53240944903922));
#51434=CARTESIAN_POINT('Ctrl Pts',(12.6739859262706,-0.206463809544117,
4.49355177571912));
#51435=CARTESIAN_POINT('Ctrl Pts',(12.6976000424205,-0.41599087873209,4.33641091237214));
#51436=CARTESIAN_POINT('Ctrl Pts',(12.7212141585703,-0.525822648369464,
4.09864686536754));
#51437=CARTESIAN_POINT('Ctrl Pts',(12.7448282747202,-0.509637448384189,
3.8372413948162));
#51438=CARTESIAN_POINT('Ctrl Pts',(12.76844239087,-0.37131404483003,3.61484216427635));
#51439=CARTESIAN_POINT('Ctrl Pts',(12.7920565070199,-0.144002664868576,
3.48474868689319));
#51440=CARTESIAN_POINT('Ctrl Pts',(12.8156706231698,0.117819965178516,3.47813877511649));
#51441=CARTESIAN_POINT('Ctrl Pts',(12.8392847393197,0.351406216185799,3.59659653799738));
#51442=CARTESIAN_POINT('Ctrl Pts',(12.8628988554695,0.500775523187073,3.81173274911973));
#51443=CARTESIAN_POINT('Ctrl Pts',(12.8865129716194,0.530130489073712,4.07198851734671));
#51444=CARTESIAN_POINT('Ctrl Pts',(12.9101270877692,0.432435993263294,4.31499173633021));
#51445=CARTESIAN_POINT('Ctrl Pts',(12.9337412039191,0.231105201134755,4.48250499290311));
#51446=CARTESIAN_POINT('Ctrl Pts',(12.957355320069,-0.0256115611541523,
4.53438256906268));
#51447=CARTESIAN_POINT('Ctrl Pts',(12.9809694362189,-0.276190334565159,
4.45819164252092));
#51448=CARTESIAN_POINT('Ctrl Pts',(13.0045835523687,-0.460578171623014,
4.27219189922559));
#51449=CARTESIAN_POINT('Ctrl Pts',(13.0281976685186,-0.534585243620437,
4.0209594724593));
#51450=CARTESIAN_POINT('Ctrl Pts',(13.0518117846684,-0.480475240551103,
3.76470396221295));
#51451=CARTESIAN_POINT('Ctrl Pts',(13.0754259008183,-0.311216001335094,
3.5648387853972));
#51452=CARTESIAN_POINT('Ctrl Pts',(13.0990400169682,-0.0673716809183137,
3.46926302296559));
#51453=CARTESIAN_POINT('Ctrl Pts',(13.122654133118,0.19261873182715,3.50088207171981));
#51454=CARTESIAN_POINT('Ctrl Pts',(13.1462682492679,0.406446724606302,3.65211820651514));
#51455=CARTESIAN_POINT('Ctrl Pts',(13.1698823654178,0.522866930420328,3.88672663484193));
#51456=CARTESIAN_POINT('Ctrl Pts',(13.1934964815676,0.513978436505609,4.14848181366307));
#51457=CARTESIAN_POINT('Ctrl Pts',(13.2171105977175,0.381911432304553,4.37465229220773));
#51458=CARTESIAN_POINT('Ctrl Pts',(13.2407247138674,0.158316694737061,4.51103474084347));
#51459=CARTESIAN_POINT('Ctrl Pts',(13.2643388300172,-0.103219740820234,
4.52494415635039));
#51460=CARTESIAN_POINT('Ctrl Pts',(13.2879529461671,-0.340018846942428,
4.41304705047411));
#51461=CARTESIAN_POINT('Ctrl Pts',(13.311567062317,-0.495330069408668,4.20216034359148));
#51462=CARTESIAN_POINT('Ctrl Pts',(13.3351811784669,-0.531931992580964,
3.94282450306062));
#51463=CARTESIAN_POINT('Ctrl Pts',(13.3587952946167,-0.44105271077271,3.69719116838925));
#51464=CARTESIAN_POINT('Ctrl Pts',(13.3824094107666,-0.244472076510672,
3.5241280781681));
#51465=CARTESIAN_POINT('Ctrl Pts',(13.4060235269164,0.0106979927399635,
3.46511100671938));
#51466=CARTESIAN_POINT('Ctrl Pts',(13.4296376430663,0.263304213558122,3.53428380605355));
#51467=CARTESIAN_POINT('Ctrl Pts',(13.4532517592162,0.452807746647384,3.71506873327496));
#51468=CARTESIAN_POINT('Ctrl Pts',(13.476865875366,0.533792751104717,3.96413942206993));
#51469=CARTESIAN_POINT('Ctrl Pts',(13.5004799915159,0.486850606847911,4.22180434800346));
#51470=CARTESIAN_POINT('Ctrl Pts',(13.5240941076658,0.323231325528255,4.42631231788287));
#51471=CARTESIAN_POINT('Ctrl Pts',(13.5477082238157,0.0821474069231642,
4.52865157307741));
#51472=CARTESIAN_POINT('Ctrl Pts',(13.5713223399655,-0.178623709606947,
4.50429579866153));
#51473=CARTESIAN_POINT('Ctrl Pts',(13.5949364561154,-0.396586410669692,
4.35908202552279));
#51474=CARTESIAN_POINT('Ctrl Pts',(13.6185505722652,-0.519504417643299,
4.12781174527607));
#51475=CARTESIAN_POINT('Ctrl Pts',(13.6421646884151,-0.517919574482721,
3.86591049053316));
#51476=CARTESIAN_POINT('Ctrl Pts',(13.665778804565,-0.392211699884016,3.6361447201764));
#51477=CARTESIAN_POINT('Ctrl Pts',(13.6893929207148,-0.172507561089802,
3.49357940054904));
#51478=CARTESIAN_POINT('Ctrl Pts',(13.7130070368647,0.0885392156030666,
3.47238130294519));
#51479=CARTESIAN_POINT('Ctrl Pts',(13.7366211530146,0.328366952925232,3.57763069902274));
#51480=CARTESIAN_POINT('Ctrl Pts',(13.7602352691644,0.489499264105438,3.78410383833506));
#51481=CARTESIAN_POINT('Ctrl Pts',(13.7838493853143,0.533319669072828,4.04231799571659));
#51482=CARTESIAN_POINT('Ctrl Pts',(13.8074635014642,0.449326302728307,4.29039035083475));
#51483=CARTESIAN_POINT('Ctrl Pts',(13.831077617614,0.257648760022572,4.46886863686992));
#51484=CARTESIAN_POINT('Ctrl Pts',(13.8546917337639,0.00422389839726028,
4.53497929012603));
#51485=CARTESIAN_POINT('Ctrl Pts',(13.8783058499138,-0.25021324988294,4.47287843233165));
#51486=CARTESIAN_POINT('Ctrl Pts',(13.9019199660636,-0.444685051009628,
4.29744896636227));
#51487=CARTESIAN_POINT('Ctrl Pts',(13.9255340822135,-0.532584984058807,
4.05073378496132));
#51488=CARTESIAN_POINT('Ctrl Pts',(13.9491481983634,-0.492847218174075,
3.79185989881933));
#51489=CARTESIAN_POINT('Ctrl Pts',(13.9727623145132,-0.334995185577738,
3.58286823685896));
#51490=CARTESIAN_POINT('Ctrl Pts',(13.9963764306631,-0.0968592247428986,
3.47384510573062));
#51491=CARTESIAN_POINT('Ctrl Pts',(14.019990546813,0.164489723571401,3.49091865775613));
#51492=CARTESIAN_POINT('Ctrl Pts',(14.0436046629628,0.386417564563212,3.62999709733779));
#51493=CARTESIAN_POINT('Ctrl Pts',(14.0672187791127,0.515737746224078,3.85774930825782));
#51494=CARTESIAN_POINT('Ctrl Pts',(14.0908328952626,0.521457786777448,4.11959288770904));
#51495=CARTESIAN_POINT('Ctrl Pts',(14.1144470114124,0.402206838685568,4.35277519909424));
#51496=CARTESIAN_POINT('Ctrl Pts',(14.1380611275623,0.186564221804844,4.50141247822903));
#51497=CARTESIAN_POINT('Ctrl Pts',(14.1616752437122,-0.0737898095680628,
4.52988276645436));
#51498=CARTESIAN_POINT('Ctrl Pts',(14.185289359862,-0.316459599402161,4.43136296100575));
#51499=CARTESIAN_POINT('Ctrl Pts',(14.2089034760119,-0.483287643257218,
4.22946401908862));
#51500=CARTESIAN_POINT('Ctrl Pts',(14.2325175921618,-0.53429243907693,3.97257242762026));
#51501=CARTESIAN_POINT('Ctrl Pts',(14.2561317083116,-0.457250332481466,
3.72225404480531));
#51502=CARTESIAN_POINT('Ctrl Pts',(14.2797458244615,-0.270625000632592,
3.53849941363631));
#51503=CARTESIAN_POINT('Ctrl Pts',(14.3033599406114,-0.0191425034699505,
3.46534661065105));
#51504=CARTESIAN_POINT('Ctrl Pts',(14.3269740567612,0.236927627906706,3.52032721432634));
#51505=CARTESIAN_POINT('Ctrl Pts',(14.3505881729111,0.436216403922163,3.69026474025285));
#51506=CARTESIAN_POINT('Ctrl Pts',(14.374202289061,0.530962882087739,3.93443247734966));
#51507=CARTESIAN_POINT('Ctrl Pts',(14.3978164052108,0.498460409348769,4.19431392768733));
#51508=CARTESIAN_POINT('Ctrl Pts',(14.4214305213607,0.346498429557861,4.40762669256976));
#51509=CARTESIAN_POINT('Ctrl Pts',(14.4450446375106,0.111495689030631,4.52324888295055));
#51510=CARTESIAN_POINT('Ctrl Pts',(14.4686587536604,-0.150227769531968,
4.51347083601981));
#51511=CARTESIAN_POINT('Ctrl Pts',(14.4922728698103,-0.375948097339969,
4.38063592879268));
#51512=CARTESIAN_POINT('Ctrl Pts',(14.5158869859602,-0.51156984651846,4.15657897149511));
#51513=CARTESIAN_POINT('Ctrl Pts',(14.53950110211,-0.52459032076832,3.89499677367918));
#51514=CARTESIAN_POINT('Ctrl Pts',(14.5631152182599,-0.411889072794842,
3.65857933001481));
#51515=CARTESIAN_POINT('Ctrl Pts',(14.5867293344098,-0.200475741228102,
3.50398572665543));
#51516=CARTESIAN_POINT('Ctrl Pts',(14.6103434505596,0.0589829973059192,
3.46826539682992));
#51517=CARTESIAN_POINT('Ctrl Pts',(14.6339575667095,0.304306049929579,3.5599789662306));
#51518=CARTESIAN_POINT('Ctrl Pts',(14.6575716828594,0.476700039321847,3.75714663952638));
#51519=CARTESIAN_POINT('Ctrl Pts',(14.6811857990092,0.53484954579562,4.0125158112076));
#51520=CARTESIAN_POINT('Ctrl Pts',(14.7047999151591,0.464818635404008,4.26488548168423));
#51521=CARTESIAN_POINT('Ctrl Pts',(14.728414031309,0.283390703164248,4.45377350235044));
#51522=CARTESIAN_POINT('Ctrl Pts',(14.7520281474588,0.0340462163765225,
4.5339115446661));
#51523=CARTESIAN_POINT('Ctrl Pts',(14.7756422636087,-0.223457683695575,
4.48609396779546));
#51524=CARTESIAN_POINT('Ctrl Pts',(14.7992563797586,-0.427408393186059,
4.32178058932398));
#51525=CARTESIAN_POINT('Ctrl Pts',(14.8228704959084,-0.528927708313459,
4.08035024907128));
#51526=CARTESIAN_POINT('Ctrl Pts',(14.8464846120583,-0.503685810960444,
3.81966341983811));
#51527=CARTESIAN_POINT('Ctrl Pts',(14.8700987282082,-0.357732113691821,
3.6021954912391));
#51528=CARTESIAN_POINT('Ctrl Pts',(14.893712844358,-0.126045401495737,3.48006421709321));
#51529=CARTESIAN_POINT('Ctrl Pts',(14.9173269605079,0.13584891809103,3.48253909847714));
#51530=CARTESIAN_POINT('Ctrl Pts',(14.9409410766578,0.365186207068703,3.60902724630258));
#51531=CARTESIAN_POINT('Ctrl Pts',(14.9645551928076,0.507003847624586,3.82921439524653));
#51532=CARTESIAN_POINT('Ctrl Pts',(14.9881693089575,0.52731498478211,4.0903322339271));
#51533=CARTESIAN_POINT('Ctrl Pts',(15.0117834251074,0.421250356706029,4.32979975898591));
#51534=CARTESIAN_POINT('Ctrl Pts',(15.0353975412572,0.214232462415332,4.49023183125449));
#51535=CARTESIAN_POINT('Ctrl Pts',(15.0590116574071,-0.0441324441701724,
4.53316925684615));
#51536=CARTESIAN_POINT('Ctrl Pts',(15.082625773557,-0.291909288096862,4.4483444097243));
#51537=CARTESIAN_POINT('Ctrl Pts',(15.1062398897068,-0.469745893811612,
4.25603780014884));
#51538=CARTESIAN_POINT('Ctrl Pts',(15.1219826338067,-0.513197418509596,
4.08697667736293));
#51539=CARTESIAN_POINT('Ctrl Pts',(15.1298540058567,-0.513578141027115,
4.0023094018511));
#51540=CARTESIAN_POINT('Ctrl Pts',(12.4701459941433,-0.231505035597357,
3.47990537377399));
#51541=CARTESIAN_POINT('Ctrl Pts',(12.4780173661933,-0.145763467775118,
3.44174000210903));
#51542=CARTESIAN_POINT('Ctrl Pts',(12.4937601102932,0.0448806955855158,
3.40867809900361));
#51543=CARTESIAN_POINT('Ctrl Pts',(12.517374226443,0.320205029627059,3.5008472864651));
#51544=CARTESIAN_POINT('Ctrl Pts',(12.5409883425929,0.518748616038451,3.71263883318769));
#51545=CARTESIAN_POINT('Ctrl Pts',(12.5646024587428,0.592991298599855,3.99330298545039));
#51546=CARTESIAN_POINT('Ctrl Pts',(12.5882165748926,0.525110091302815,4.27557062957281));
#51547=CARTESIAN_POINT('Ctrl Pts',(12.6118306910425,0.331387039860997,4.49179666512739));
#51548=CARTESIAN_POINT('Ctrl Pts',(12.6354448071924,0.0582427139750047,
4.5901598492798));
#51549=CARTESIAN_POINT('Ctrl Pts',(12.6590589233422,-0.22885891853004,4.54708728798072));
#51550=CARTESIAN_POINT('Ctrl Pts',(12.6826730394921,-0.461113368174311,
4.37290137073994));
#51551=CARTESIAN_POINT('Ctrl Pts',(12.706287155642,-0.582858578993347,4.10934708109011));
#51552=CARTESIAN_POINT('Ctrl Pts',(12.7299012717918,-0.564917771967644,
3.8195869850214));
#51553=CARTESIAN_POINT('Ctrl Pts',(12.7535153879417,-0.411590442520908,
3.57306413195747));
#51554=CARTESIAN_POINT('Ctrl Pts',(12.7771295040916,-0.159622619673808,
3.42885942795892));
#51555=CARTESIAN_POINT('Ctrl Pts',(12.8007436202414,0.130599885139872,3.42153253970604));
#51556=CARTESIAN_POINT('Ctrl Pts',(12.8243577363913,0.38952321367407,3.55283940440193));
#51557=CARTESIAN_POINT('Ctrl Pts',(12.8479718525412,0.555094594621529,3.79131141905102));
#51558=CARTESIAN_POINT('Ctrl Pts',(12.871585968691,0.587633690752404,4.07979710469805));
#51559=CARTESIAN_POINT('Ctrl Pts',(12.8952000848409,0.479342282651013,4.34915885879276));
#51560=CARTESIAN_POINT('Ctrl Pts',(12.9188142009908,0.256173159427565,4.53484226172604));
#51561=CARTESIAN_POINT('Ctrl Pts',(12.9424283171406,-0.0283896446575681,
4.59234699343691));
#51562=CARTESIAN_POINT('Ctrl Pts',(12.9660424332905,-0.306148672818738,
4.50789164463438));
#51563=CARTESIAN_POINT('Ctrl Pts',(12.9896565494404,-0.510537040311962,
4.30171652759364));
#51564=CARTESIAN_POINT('Ctrl Pts',(13.0132706655902,-0.59257165208389,4.02323294436244));
#51565=CARTESIAN_POINT('Ctrl Pts',(13.0368847817401,-0.532592342337314,
3.73918142428326));
#51566=CARTESIAN_POINT('Ctrl Pts',(13.06049889789,-0.344973570196446,3.51763689152052));
#51567=CARTESIAN_POINT('Ctrl Pts',(13.0841130140398,-0.0746794804792245,
3.41169403559782));
#51568=CARTESIAN_POINT('Ctrl Pts',(13.1077271301897,0.213512066603468,3.44674279944083));
#51569=CARTESIAN_POINT('Ctrl Pts',(13.1313412463396,0.450533960595157,3.6143835028084));
#51570=CARTESIAN_POINT('Ctrl Pts',(13.1549553624894,0.579582254610818,3.87443988413478));
#51571=CARTESIAN_POINT('Ctrl Pts',(13.1785694786393,0.569729626640933,4.1645876212947));
#51572=CARTESIAN_POINT('Ctrl Pts',(13.2021835947892,0.423337327565886,4.41529078926125));
#51573=CARTESIAN_POINT('Ctrl Pts',(13.225797710939,0.175489290945357,4.56646662860168));
#51574=CARTESIAN_POINT('Ctrl Pts',(13.2494118270889,-0.114415975890545,
4.58188479703192));
#51575=CARTESIAN_POINT('Ctrl Pts',(13.2730259432388,-0.376900657615966,
4.45785022315656));
#51576=CARTESIAN_POINT('Ctrl Pts',(13.2966400593886,-0.54905847301076,4.22408865605146));
#51577=CARTESIAN_POINT('Ctrl Pts',(13.3202541755385,-0.589630603166779,
3.93662268256671));
#51578=CARTESIAN_POINT('Ctrl Pts',(13.3438682916884,-0.488893654655812,
3.66434552439578));
#51579=CARTESIAN_POINT('Ctrl Pts',(13.3674824078382,-0.270989938452484,
3.47251029790774));
#51580=CARTESIAN_POINT('Ctrl Pts',(13.3910965239881,0.0118584029536041,
3.40709165056035));
#51581=CARTESIAN_POINT('Ctrl Pts',(13.414710640138,0.291864795541507,3.48376761659174));
#51582=CARTESIAN_POINT('Ctrl Pts',(13.4383247562878,0.501923758108325,3.68416226697515));
#51583=CARTESIAN_POINT('Ctrl Pts',(13.4619388724377,0.591693197983429,3.96024962873126));
#51584=CARTESIAN_POINT('Ctrl Pts',(13.4855529885876,0.539659243985316,4.2458634436777));
#51585=CARTESIAN_POINT('Ctrl Pts',(13.5091671047374,0.358292195415589,4.47255437280819));
#51586=CARTESIAN_POINT('Ctrl Pts',(13.5327812208873,0.0910579280213527,
4.58599435688436));
#51587=CARTESIAN_POINT('Ctrl Pts',(13.5563953370372,-0.197999005708236,
4.55899671402827));
#51588=CARTESIAN_POINT('Ctrl Pts',(13.580009453187,-0.439604099381795,4.39803161729011));
#51589=CARTESIAN_POINT('Ctrl Pts',(13.6036235693369,-0.575855010405679,
4.14167547263565));
#51590=CARTESIAN_POINT('Ctrl Pts',(13.6272376854868,-0.574098259464336,
3.85136581471317));
#51591=CARTESIAN_POINT('Ctrl Pts',(13.6508518016366,-0.434754864150196,
3.59667737398752));
#51592=CARTESIAN_POINT('Ctrl Pts',(13.6744659177865,-0.191219439166798,
3.43864800825098));
#51593=CARTESIAN_POINT('Ctrl Pts',(13.6980800339364,0.0981430555561168,
3.41515055509818));
#51594=CARTESIAN_POINT('Ctrl Pts',(13.7216941500862,0.363984883808003,3.53181634275091));
#51595=CARTESIAN_POINT('Ctrl Pts',(13.7453082662361,0.54259520083341,3.76068560304818));
#51596=CARTESIAN_POINT('Ctrl Pts',(13.768922382386,0.591168800790367,4.04690822452342));
#51597=CARTESIAN_POINT('Ctrl Pts',(13.7925364985358,0.498064682311931,4.32188896344761));
#51598=CARTESIAN_POINT('Ctrl Pts',(13.8161506146857,0.28559589552072,4.51972677150362));
#51599=CARTESIAN_POINT('Ctrl Pts',(13.8397647308356,0.00468206423833927,
4.59300844077494));
#51600=CARTESIAN_POINT('Ctrl Pts',(13.8633788469854,-0.277353856332193,
4.52417150908221));
#51601=CARTESIAN_POINT('Ctrl Pts',(13.8869929631353,-0.492919994478707,
4.32971322630275));
#51602=CARTESIAN_POINT('Ctrl Pts',(13.9106070792852,-0.590354424565592,
4.05623687359455));
#51603=CARTESIAN_POINT('Ctrl Pts',(13.934221195435,-0.546306307148498,3.76928296264551));
#51604=CARTESIAN_POINT('Ctrl Pts',(13.9578353115849,-0.371332080200278,
3.53762199579782));
#51605=CARTESIAN_POINT('Ctrl Pts',(13.9814494277348,-0.107365535263851,
3.41677313642685));
#51606=CARTESIAN_POINT('Ctrl Pts',(14.0050635438846,0.182331907606365,3.43569865495067));
#51607=CARTESIAN_POINT('Ctrl Pts',(14.0286776600345,0.428332239544634,3.58986291910809));
#51608=CARTESIAN_POINT('Ctrl Pts',(14.0522917761844,0.571679768510432,3.8423193898042));
#51609=CARTESIAN_POINT('Ctrl Pts',(14.0759058923342,0.578020261296468,4.1325651164018));
#51610=CARTESIAN_POINT('Ctrl Pts',(14.0995200084841,0.445834174668256,4.39104069002309));
#51611=CARTESIAN_POINT('Ctrl Pts',(14.123134124634,0.206800824478305,4.55580064011384));
#51612=CARTESIAN_POINT('Ctrl Pts',(14.1467482407838,-0.0817937829083601,
4.58735909768505));
#51613=CARTESIAN_POINT('Ctrl Pts',(14.1703623569337,-0.350785940826847,
4.4781528586907));
#51614=CARTESIAN_POINT('Ctrl Pts',(14.1939764730836,-0.535709806086595,
4.25435395852733));
#51615=CARTESIAN_POINT('Ctrl Pts',(14.2175905892334,-0.59224708706053,3.96959736155895));
#51616=CARTESIAN_POINT('Ctrl Pts',(14.2412047053833,-0.506848230788112,
3.69212696853602));
#51617=CARTESIAN_POINT('Ctrl Pts',(14.2648188215332,-0.29997966766535,3.48844049071174));
#51618=CARTESIAN_POINT('Ctrl Pts',(14.288432937683,-0.0212188889266537,
3.40735281042717));
#51619=CARTESIAN_POINT('Ctrl Pts',(14.3120470538329,0.262627144255178,3.46829715474127));
#51620=CARTESIAN_POINT('Ctrl Pts',(14.3356611699828,0.483532754079872,3.65666778728498));
#51621=CARTESIAN_POINT('Ctrl Pts',(14.3592752861326,0.588556373354274,3.9273203746575));
#51622=CARTESIAN_POINT('Ctrl Pts',(14.3828894022825,0.55252836061433,4.21539114019081));
#51623=CARTESIAN_POINT('Ctrl Pts',(14.4065035184324,0.384083079916361,4.45184191956682));
#51624=CARTESIAN_POINT('Ctrl Pts',(14.4301176345822,0.123589615384189,4.58000563749418));
#51625=CARTESIAN_POINT('Ctrl Pts',(14.4537317507321,-0.166522960823891,
4.56916696678068));
#51626=CARTESIAN_POINT('Ctrl Pts',(14.477345866882,-0.416727150247931,4.42192347031433));
#51627=CARTESIAN_POINT('Ctrl Pts',(14.5009599830318,-0.567059777136274,
4.17356307703535));
#51628=CARTESIAN_POINT('Ctrl Pts',(14.5245740991817,-0.58149258093928,3.88360708411314));
#51629=CARTESIAN_POINT('Ctrl Pts',(14.5481882153316,-0.456566639753037,
3.62154546373458));
#51630=CARTESIAN_POINT('Ctrl Pts',(14.5718023314814,-0.222221325036472,
3.45018310752014));
#51631=CARTESIAN_POINT('Ctrl Pts',(14.5954164476313,0.0653808771856868,
3.41058819705396));
#51632=CARTESIAN_POINT('Ctrl Pts',(14.6190305637812,0.337314097045906,3.51224992824993));
#51633=CARTESIAN_POINT('Ctrl Pts',(14.642644679931,0.528407645404381,3.73080435955289));
#51634=CARTESIAN_POINT('Ctrl Pts',(14.6662587960809,0.592864623089856,4.0138734000105));
#51635=CARTESIAN_POINT('Ctrl Pts',(14.6898729122308,0.515237466779568,4.29361758366474));
#51636=CARTESIAN_POINT('Ctrl Pts',(14.7134870283806,0.314130064687094,4.5029942692369));
#51637=CARTESIAN_POINT('Ctrl Pts',(14.7371011445305,0.0377392060970651,
4.59182487707066));
#51638=CARTESIAN_POINT('Ctrl Pts',(14.7607152606804,-0.24769611652869,4.53882053236973));
#51639=CARTESIAN_POINT('Ctrl Pts',(14.7843293768302,-0.47376933929102,4.35668409799883));
#51640=CARTESIAN_POINT('Ctrl Pts',(14.8079434929801,-0.586300444482135,
4.08906583263515));
#51641=CARTESIAN_POINT('Ctrl Pts',(14.83155760913,-0.558320561021625,3.80010232883727));
#51642=CARTESIAN_POINT('Ctrl Pts',(14.8551717252798,-0.396535280656446,
3.55904567554761));
#51643=CARTESIAN_POINT('Ctrl Pts',(14.8787858414297,-0.139717533720287,
3.42366683418339));
#51644=CARTESIAN_POINT('Ctrl Pts',(14.9023999575795,0.150584436790342,3.42641016570609));
#51645=CARTESIAN_POINT('Ctrl Pts',(14.9260140737294,0.404797918804129,3.56661847040663));
#51646=CARTESIAN_POINT('Ctrl Pts',(14.9496281898793,0.561998504794314,3.8106892976029));
#51647=CARTESIAN_POINT('Ctrl Pts',(14.9732423060292,0.584512788988964,4.10013056240029));
#51648=CARTESIAN_POINT('Ctrl Pts',(14.996856422179,0.466943341203511,4.36557310620026));
#51649=CARTESIAN_POINT('Ctrl Pts',(15.0204705383289,0.237470236409271,4.54340722946861));
#51650=CARTESIAN_POINT('Ctrl Pts',(15.0440846544788,-0.0489194860211801,
4.59100207336435));
#51651=CARTESIAN_POINT('Ctrl Pts',(15.0676987706286,-0.323572659684198,
4.49697628347096));
#51652=CARTESIAN_POINT('Ctrl Pts',(15.0913128867785,-0.520699184418956,
4.28381019498893));
#51653=CARTESIAN_POINT('Ctrl Pts',(15.1070556308784,-0.568863891700195,
4.09641102894772));
#51654=CARTESIAN_POINT('Ctrl Pts',(15.1149270029284,-0.569285911151507,
4.00255990244131));
#51655=CARTESIAN_POINT('Ctrl Pts',(12.455218991215,-0.25415908175074,3.42901124252432));
#51656=CARTESIAN_POINT('Ctrl Pts',(12.4630903632649,-0.16002722803387,3.38711117848463));
#51657=CARTESIAN_POINT('Ctrl Pts',(12.4788331073648,0.0492725194893315,
3.35081398558546));
#51658=CARTESIAN_POINT('Ctrl Pts',(12.5024472235147,0.351538860016532,3.45200243701797));
#51659=CARTESIAN_POINT('Ctrl Pts',(12.5260613396645,0.569511032758309,3.68451895614546));
#51660=CARTESIAN_POINT('Ctrl Pts',(12.5496754558144,0.651018771792273,3.99264764559437));
#51661=CARTESIAN_POINT('Ctrl Pts',(12.5732895719643,0.576495013506714,4.3025367374363));
#51662=CARTESIAN_POINT('Ctrl Pts',(12.5969036881141,0.363815091701307,4.53992168461618));
#51663=CARTESIAN_POINT('Ctrl Pts',(12.620517804264,0.0639420851661475,4.64791024952038));
#51664=CARTESIAN_POINT('Ctrl Pts',(12.6441319204139,-0.251254027515963,
4.60062280024232));
#51665=CARTESIAN_POINT('Ctrl Pts',(12.6677460365637,-0.506235857616531,
4.40939182910775));
#51666=CARTESIAN_POINT('Ctrl Pts',(12.6913601527136,-0.639894509617229,
4.12004729681268));
#51667=CARTESIAN_POINT('Ctrl Pts',(12.7149742688635,-0.620198095551099,
3.8019325752266));
#51668=CARTESIAN_POINT('Ctrl Pts',(12.7385883850133,-0.451866840211785,
3.53128609963859));
#51669=CARTESIAN_POINT('Ctrl Pts',(12.7622025011632,-0.17524257447904,3.37297016902465));
#51670=CARTESIAN_POINT('Ctrl Pts',(12.7858166173131,0.143379805101228,3.36492630429559));
#51671=CARTESIAN_POINT('Ctrl Pts',(12.809430733463,0.42764021116234,3.50908227080648));
#51672=CARTESIAN_POINT('Ctrl Pts',(12.8330448496128,0.609413666055986,3.77089008898231));
#51673=CARTESIAN_POINT('Ctrl Pts',(12.8566589657627,0.645136892431096,4.08760569204938));
#51674=CARTESIAN_POINT('Ctrl Pts',(12.8802730819125,0.526248572038732,4.38332598125533));
#51675=CARTESIAN_POINT('Ctrl Pts',(12.9038871980624,0.281241117720374,4.58717953054897));
#51676=CARTESIAN_POINT('Ctrl Pts',(12.9275013142123,-0.0311677281609838,
4.65031141781114));
#51677=CARTESIAN_POINT('Ctrl Pts',(12.9511154303622,-0.336107011072318,
4.55759164674784));
#51678=CARTESIAN_POINT('Ctrl Pts',(12.974729546512,-0.56049590900091,4.33124115596169));
#51679=CARTESIAN_POINT('Ctrl Pts',(12.9983436626619,-0.650558060547343,
4.02550641626558));
#51680=CARTESIAN_POINT('Ctrl Pts',(13.0219577788117,-0.584709444123524,
3.71365888635357));
#51681=CARTESIAN_POINT('Ctrl Pts',(13.0455718949616,-0.378731139057797,
3.47043499764384));
#51682=CARTESIAN_POINT('Ctrl Pts',(13.0691860111115,-0.0819872800401352,
3.35412504823007));
#51683=CARTESIAN_POINT('Ctrl Pts',(13.0928001272613,0.234405401379786,3.39260352716186));
#51684=CARTESIAN_POINT('Ctrl Pts',(13.1164142434112,0.494621196584012,3.57664879910166));
#51685=CARTESIAN_POINT('Ctrl Pts',(13.1400283595611,0.636297578801308,3.86215313342763));
#51686=CARTESIAN_POINT('Ctrl Pts',(13.1636424757109,0.625480816776257,4.18069342892634));
#51687=CARTESIAN_POINT('Ctrl Pts',(13.1872565918608,0.464763222827219,4.45592928631477));
#51688=CARTESIAN_POINT('Ctrl Pts',(13.2108707080107,0.192661887153653,4.62189851635989));
#51689=CARTESIAN_POINT('Ctrl Pts',(13.2344848241605,-0.125612210960856,
4.63882543771344));
#51690=CARTESIAN_POINT('Ctrl Pts',(13.2580989403104,-0.413782468289504,
4.50265339583901));
#51691=CARTESIAN_POINT('Ctrl Pts',(13.2817130564603,-0.602786876612853,
4.24601696851145));
#51692=CARTESIAN_POINT('Ctrl Pts',(13.3053271726101,-0.647329213752593,
3.9304208620728));
#51693=CARTESIAN_POINT('Ctrl Pts',(13.32894128876,-0.536734598538914,3.6314998804023));
#51694=CARTESIAN_POINT('Ctrl Pts',(13.3525554049099,-0.297507800394296,
3.42089251764738));
#51695=CARTESIAN_POINT('Ctrl Pts',(13.3761695210598,0.0130188131672444,
3.34907229440132));
#51696=CARTESIAN_POINT('Ctrl Pts',(13.3997836372096,0.320425377524893,3.43325142712992));
#51697=CARTESIAN_POINT('Ctrl Pts',(13.4233977533595,0.551039769569266,3.65325580067535));
#51698=CARTESIAN_POINT('Ctrl Pts',(13.4470118695093,0.649593644862141,3.95635983539258));
#51699=CARTESIAN_POINT('Ctrl Pts',(13.4706259856592,0.592467881122722,4.26992253935193));
#51700=CARTESIAN_POINT('Ctrl Pts',(13.4942401018091,0.393353065302923,4.5187964277335));
#51701=CARTESIAN_POINT('Ctrl Pts',(13.5178542179589,0.0999684491195412,
4.64333714069132));
#51702=CARTESIAN_POINT('Ctrl Pts',(13.5414683341088,-0.217374301809525,
4.61369762939502));
#51703=CARTESIAN_POINT('Ctrl Pts',(13.5650824502587,-0.482621788093898,
4.43698120905743));
#51704=CARTESIAN_POINT('Ctrl Pts',(13.5886965664085,-0.632205603168059,
4.15553919999523));
#51705=CARTESIAN_POINT('Ctrl Pts',(13.6123106825584,-0.630276944445953,
3.83682113889318));
#51706=CARTESIAN_POINT('Ctrl Pts',(13.6359247987083,-0.477298028416376,
3.55721002779864));
#51707=CARTESIAN_POINT('Ctrl Pts',(13.6595389148582,-0.209931317243796,
3.38371661595291));
#51708=CARTESIAN_POINT('Ctrl Pts',(13.683153031008,0.107746895509167,3.35791980725116));
#51709=CARTESIAN_POINT('Ctrl Pts',(13.7067671471579,0.399602814690774,3.48600198647908));
#51710=CARTESIAN_POINT('Ctrl Pts',(13.7303812633077,0.59569113756138,3.73726736776131));
#51711=CARTESIAN_POINT('Ctrl Pts',(13.7539953794576,0.649017932507905,4.05149845333026));
#51712=CARTESIAN_POINT('Ctrl Pts',(13.7776094956075,0.546803061895555,4.35338757606046));
#51713=CARTESIAN_POINT('Ctrl Pts',(13.8012236117573,0.313543031018869,4.57058490613733));
#51714=CARTESIAN_POINT('Ctrl Pts',(13.8248377279072,0.00514023007941788,
4.65103759142385));
#51715=CARTESIAN_POINT('Ctrl Pts',(13.8484518440571,-0.304494462781446,
4.57546458583277));
#51716=CARTESIAN_POINT('Ctrl Pts',(13.8720659602069,-0.541154937947787,
4.36197748624323));
#51717=CARTESIAN_POINT('Ctrl Pts',(13.8956800763568,-0.648123865072376,
4.06173996222779));
#51718=CARTESIAN_POINT('Ctrl Pts',(13.9192941925067,-0.599765396122921,
3.74670602647169));
#51719=CARTESIAN_POINT('Ctrl Pts',(13.9429083086565,-0.407668974822819,
3.49237575473668));
#51720=CARTESIAN_POINT('Ctrl Pts',(13.9665224248064,-0.117871845784803,
3.35970116712309));
#51721=CARTESIAN_POINT('Ctrl Pts',(13.9901365409563,0.200174091641329,3.38047865214521));
#51722=CARTESIAN_POINT('Ctrl Pts',(14.0137506571061,0.470246914526057,3.54972874087838));
#51723=CARTESIAN_POINT('Ctrl Pts',(14.037364773256,0.627621790796785,3.82688947135059));
#51724=CARTESIAN_POINT('Ctrl Pts',(14.0609788894059,0.634582735815489,4.14553734509456));
#51725=CARTESIAN_POINT('Ctrl Pts',(14.0845930055557,0.489461510650943,4.42930618095194));
#51726=CARTESIAN_POINT('Ctrl Pts',(14.1082071217056,0.227037427151766,4.61018880199865));
#51727=CARTESIAN_POINT('Ctrl Pts',(14.1318212378555,-0.0897977562486571,
4.64483542891575));
#51728=CARTESIAN_POINT('Ctrl Pts',(14.1554353540053,-0.385112282251534,
4.52494275637564));
#51729=CARTESIAN_POINT('Ctrl Pts',(14.1790494701552,-0.588131968915973,
4.27924389796604));
#51730=CARTESIAN_POINT('Ctrl Pts',(14.2026635863051,-0.65020173504413,3.96662229549764));
#51731=CARTESIAN_POINT('Ctrl Pts',(14.2262777024549,-0.556446129094758,
3.66199989226673));
#51732=CARTESIAN_POINT('Ctrl Pts',(14.2498918186048,-0.329334334698108,
3.43838156778717));
#51733=CARTESIAN_POINT('Ctrl Pts',(14.2735059347547,-0.0232952743833569,
3.34935901020328));
#51734=CARTESIAN_POINT('Ctrl Pts',(14.2971200509045,0.28832666060365,3.41626709515619));
#51735=CARTESIAN_POINT('Ctrl Pts',(14.3207341670544,0.530849104237583,3.62307083431711));
#51736=CARTESIAN_POINT('Ctrl Pts',(14.3443482832043,0.646149864620809,3.92020827196535));
#51737=CARTESIAN_POINT('Ctrl Pts',(14.3679623993541,0.606596311879891,4.2364683526943));
#51738=CARTESIAN_POINT('Ctrl Pts',(14.391576515504,0.42166773027486,4.49605714656388));
#51739=CARTESIAN_POINT('Ctrl Pts',(14.4151906316539,0.135683541737747,4.63676239203782));
#51740=CARTESIAN_POINT('Ctrl Pts',(14.4388047478037,-0.182818152115814,
4.62486309754155));
#51741=CARTESIAN_POINT('Ctrl Pts',(14.4624188639536,-0.457506203155893,
4.46321101183598));
#51742=CARTESIAN_POINT('Ctrl Pts',(14.4860329801035,-0.622549707754089,
4.19054718257559));
#51743=CARTESIAN_POINT('Ctrl Pts',(14.5096470962533,-0.63839484111024,3.87221739454711));
#51744=CARTESIAN_POINT('Ctrl Pts',(14.5332612124032,-0.501244206711231,
3.58451159745434));
#51745=CARTESIAN_POINT('Ctrl Pts',(14.5568753285531,-0.243966908844842,
3.39638048838484));
#51746=CARTESIAN_POINT('Ctrl Pts',(14.5804894447029,0.0717787570654544,
3.35291099727801));
#51747=CARTESIAN_POINT('Ctrl Pts',(14.6041035608528,0.370322144162233,3.46452089026927));
#51748=CARTESIAN_POINT('Ctrl Pts',(14.6277176770027,0.580115251486915,3.70446207957941));
#51749=CARTESIAN_POINT('Ctrl Pts',(14.6513317931525,0.650879700384091,4.0152309888134));
#51750=CARTESIAN_POINT('Ctrl Pts',(14.6749459093024,0.565656298155129,4.32234968564526));
#51751=CARTESIAN_POINT('Ctrl Pts',(14.6985600254523,0.344869426209941,4.55221503612336));
#51752=CARTESIAN_POINT('Ctrl Pts',(14.7221741416021,0.041432195817608,4.64973820947522));
#51753=CARTESIAN_POINT('Ctrl Pts',(14.745788257752,-0.271934549361806,4.59154709694401));
#51754=CARTESIAN_POINT('Ctrl Pts',(14.7694023739019,-0.520130285395982,
4.39158760667368));
#51755=CARTESIAN_POINT('Ctrl Pts',(14.7930164900517,-0.64367318065081,4.09778141619902));
#51756=CARTESIAN_POINT('Ctrl Pts',(14.8166306062016,-0.612955311082805,
3.78054123783642));
#51757=CARTESIAN_POINT('Ctrl Pts',(14.8402447223515,-0.435338447621071,
3.51589585985611));
#51758=CARTESIAN_POINT('Ctrl Pts',(14.8638588385013,-0.153389665944836,
3.36726945127358));
#51759=CARTESIAN_POINT('Ctrl Pts',(14.8874729546512,0.165319955489652,3.37028123293502));
#51760=CARTESIAN_POINT('Ctrl Pts',(14.9110870708011,0.444409630539555,3.52420969451069));
#51761=CARTESIAN_POINT('Ctrl Pts',(14.9347011869509,0.616993161964042,3.79216419995926));
#51762=CARTESIAN_POINT('Ctrl Pts',(14.9583153031008,0.641710593195818,4.10992889087348));
#51763=CARTESIAN_POINT('Ctrl Pts',(14.9819294192507,0.512636325700993,4.40134645341462));
#51764=CARTESIAN_POINT('Ctrl Pts',(15.0055435354005,0.260708010403211,4.59658262768273));
#51765=CARTESIAN_POINT('Ctrl Pts',(15.0291576515504,-0.0537065278721878,
4.64883488988255));
#51766=CARTESIAN_POINT('Ctrl Pts',(15.0527717677003,-0.355236031271534,
4.54560815721762));
#51767=CARTESIAN_POINT('Ctrl Pts',(15.0763858838501,-0.571652475026301,
4.31158258982903));
#51768=CARTESIAN_POINT('Ctrl Pts',(15.09212862795,-0.624530364890795,4.10584538053252));
#51769=CARTESIAN_POINT('Ctrl Pts',(15.1,-0.624993681275899,4.00281040303152));
#51770=CARTESIAN_POINT('Ctrl Pts',(15.1,-0.624993681275899,4.00281040303152));
#51771=CARTESIAN_POINT('Ctrl Pts',(15.1,-0.617358358083874,4.02914127082806));
#51772=CARTESIAN_POINT('Ctrl Pts',(15.1,-0.607931963506944,4.05484759228836));
#51773=CARTESIAN_POINT('Ctrl Pts',(15.1,-0.596773861259576,4.07974656001827));
#51774=CARTESIAN_POINT('Ctrl Pts',(15.1,-0.585871522029423,4.10407480030985));
#51775=CARTESIAN_POINT('Ctrl Pts',(15.1,-0.573314772633929,4.12763281365198));
#51776=CARTESIAN_POINT('Ctrl Pts',(15.1,-0.559143639302279,4.1502040881484));
#51777=CARTESIAN_POINT('Ctrl Pts',(15.1,-0.549626121151564,4.16536325076984));
#51778=CARTESIAN_POINT('Ctrl Pts',(15.1,-0.539380106047495,4.18007635520315));
#51779=CARTESIAN_POINT('Ctrl Pts',(15.1,-0.528417753985571,4.19426420824267));
#51780=CARTESIAN_POINT('Ctrl Pts',(15.1,-0.523814643226911,4.2002217124899));
#51781=CARTESIAN_POINT('Ctrl Pts',(15.1,-0.519084627089791,4.20608691507751));
#51782=CARTESIAN_POINT('Ctrl Pts',(15.1,-0.514239086396905,4.21184190560023));
#51783=CARTESIAN_POINT('Ctrl Pts',(15.1,-0.50085552272952,4.2277374035328));
#51784=CARTESIAN_POINT('Ctrl Pts',(15.1,-0.486572803760524,4.24281789068328));
#51785=CARTESIAN_POINT('Ctrl Pts',(15.1,-0.4714177983537,4.25697008589974));
#51786=CARTESIAN_POINT('Ctrl Pts',(15.1,-0.457151696655403,4.27029219637033));
#51787=CARTESIAN_POINT('Ctrl Pts',(15.1,-0.442112042545397,4.28279146400573));
#51788=CARTESIAN_POINT('Ctrl Pts',(15.1,-0.426369607892924,4.29437520287289));
#51789=CARTESIAN_POINT('Ctrl Pts',(15.1,-0.419074661497203,4.29974303548351));
#51790=CARTESIAN_POINT('Ctrl Pts',(15.1,-0.411628924918527,4.30491398987477));
#51791=CARTESIAN_POINT('Ctrl Pts',(15.1,-0.404040271526401,4.30987739070861));
#51792=CARTESIAN_POINT('Ctrl Pts',(15.1,-0.398073367501634,4.31378007737535));
#51793=CARTESIAN_POINT('Ctrl Pts',(15.1,-0.392026704362881,4.31754881952869));
#51794=CARTESIAN_POINT('Ctrl Pts',(15.1,-0.385904261325812,4.32117966642505));
#51795=CARTESIAN_POINT('Ctrl Pts',(15.1,-0.366868686798561,4.33246850264191));
#51796=CARTESIAN_POINT('Ctrl Pts',(15.1,-0.347097727375919,4.34242824684389));
#51797=CARTESIAN_POINT('Ctrl Pts',(15.1,-0.326713262272485,4.3509180109496));
#51798=CARTESIAN_POINT('Ctrl Pts',(15.1,-0.308010762698638,4.35870726657947));
#51799=CARTESIAN_POINT('Ctrl Pts',(15.1,-0.288791261952878,4.36525839133365));
#51800=CARTESIAN_POINT('Ctrl Pts',(15.1,-0.269173508333929,4.37043259773196));
#51801=CARTESIAN_POINT('Ctrl Pts',(12.5,-0.186196943290592,3.58169363627332));
#51802=CARTESIAN_POINT('Ctrl Pts',(12.5,-0.170588484282379,3.56594316788148));
#51803=CARTESIAN_POINT('Ctrl Pts',(12.5,-0.153797667832464,3.55144458439849));
#51804=CARTESIAN_POINT('Ctrl Pts',(12.5,-0.136060690067392,3.53823162417247));
#51805=CARTESIAN_POINT('Ctrl Pts',(12.5,-0.117990710310259,3.5247705978929));
#51806=CARTESIAN_POINT('Ctrl Pts',(12.5,-0.0989385549429972,3.51264262455394));
#51807=CARTESIAN_POINT('Ctrl Pts',(12.5,-0.0790990435859813,3.5018744512649));
#51808=CARTESIAN_POINT('Ctrl Pts',(12.5,-0.0668145727052721,3.49520688224936));
#51809=CARTESIAN_POINT('Ctrl Pts',(12.5,-0.054227138249592,3.4890605701039));
#51810=CARTESIAN_POINT('Ctrl Pts',(12.5,-0.0413735013057162,3.4834433907237));
#51811=CARTESIAN_POINT('Ctrl Pts',(12.5,-0.0353493612034326,3.48081077586818));
#51812=CARTESIAN_POINT('Ctrl Pts',(12.5,-0.0292710672153644,3.47829647656688));
#51813=CARTESIAN_POINT('Ctrl Pts',(12.5,-0.0231507758853709,3.47590397706369));
#51814=CARTESIAN_POINT('Ctrl Pts',(12.5,-0.00211397253512804,3.467680423829));
#51815=CARTESIAN_POINT('Ctrl Pts',(12.5,0.0194422610390746,3.46088402724794));
#51816=CARTESIAN_POINT('Ctrl Pts',(12.5,0.0413436963816045,3.45552737346533));
#51817=CARTESIAN_POINT('Ctrl Pts',(12.5,0.0650920698750741,3.44971899548849));
#51818=CARTESIAN_POINT('Ctrl Pts',(12.5,0.089246474293393,3.44560199012534));
#51819=CARTESIAN_POINT('Ctrl Pts',(12.5,0.113633446029948,3.44311473184586));
#51820=CARTESIAN_POINT('Ctrl Pts',(12.5,0.123118497624279,3.44214733936417));
#51821=CARTESIAN_POINT('Ctrl Pts',(12.5,0.132642564327611,3.44142688205345));
#51822=CARTESIAN_POINT('Ctrl Pts',(12.5,0.142169452875131,3.44095138714122));
#51823=CARTESIAN_POINT('Ctrl Pts',(12.5,0.170359862108328,3.43954438042575));
#51824=CARTESIAN_POINT('Ctrl Pts',(12.5,0.19861482332424,3.44027367679077));
#51825=CARTESIAN_POINT('Ctrl Pts',(12.5,0.226679319731597,3.44302987267532));
#51826=CARTESIAN_POINT('Ctrl Pts',(12.5,0.254743816138955,3.44578606855986));
#51827=CARTESIAN_POINT('Ctrl Pts',(12.5,0.282619254593541,3.45056842907764));
#51828=CARTESIAN_POINT('Ctrl Pts',(12.5,0.310093463203745,3.45730861053194));
#51829=CARTESIAN_POINT('Ctrl Pts',(15.0699957084852,-1.05870731373636E-5,
4.45788944868556));
#51830=CARTESIAN_POINT('Ctrl Pts',(15.0634386537186,0.0628625045491076,
4.45782850550181));
#51831=CARTESIAN_POINT('Ctrl Pts',(15.0568815989521,0.125761012144406,4.44477074790967));
#51832=CARTESIAN_POINT('Ctrl Pts',(15.0503245441856,0.183365120595825,4.41959809737683));
#51833=CARTESIAN_POINT('Ctrl Pts',(15.0424531721356,0.252515583017112,4.38937975928409));
#51834=CARTESIAN_POINT('Ctrl Pts',(15.0345818000857,0.314036477612831,4.34170308552782));
#51835=CARTESIAN_POINT('Ctrl Pts',(15.0267104280357,0.360556892971808,4.28228266426341));
#51836=CARTESIAN_POINT('Ctrl Pts',(15.0188390559858,0.407077308330786,4.222862242999));
#51837=CARTESIAN_POINT('Ctrl Pts',(15.0109676839358,0.438597244453022,4.15169807422645));
#51838=CARTESIAN_POINT('Ctrl Pts',(15.0030963118859,0.45133921416074,4.07731692107955));
#51839=CARTESIAN_POINT('Ctrl Pts',(14.9952249398359,0.464081183868457,4.00293576793266));
#51840=CARTESIAN_POINT('Ctrl Pts',(14.9873535677859,0.458045187161657,3.92533763041141));
#51841=CARTESIAN_POINT('Ctrl Pts',(14.979482195736,0.433954739621328,3.85382131653551));
#51842=CARTESIAN_POINT('Ctrl Pts',(14.971610823686,0.409864292080999,3.78230500265962));
#51843=CARTESIAN_POINT('Ctrl Pts',(14.9637394516361,0.367719393707138,3.71687051242907));
#51844=CARTESIAN_POINT('Ctrl Pts',(14.9558680795861,0.312570095196614,3.66535860215541));
#51845=CARTESIAN_POINT('Ctrl Pts',(14.9479967075362,0.257420796686091,3.61384669188175));
#51846=CARTESIAN_POINT('Ctrl Pts',(14.9401253354862,0.189267098038905,3.57625736156498));
#51847=CARTESIAN_POINT('Ctrl Pts',(14.9322539634362,0.116275803938161,3.55709495786573));
#51848=CARTESIAN_POINT('Ctrl Pts',(14.9243825913863,0.0432845098374172,
3.53793255416647));
#51849=CARTESIAN_POINT('Ctrl Pts',(14.9165112193363,-0.0345443797168851,
3.53719707708475));
#51850=CARTESIAN_POINT('Ctrl Pts',(14.9086398472864,-0.107884770736704,
3.55497662303181));
#51851=CARTESIAN_POINT('Ctrl Pts',(14.9007684752364,-0.181225161756525,
3.57275616897888));
#51852=CARTESIAN_POINT('Ctrl Pts',(14.8928971031865,-0.250077054241862,
3.60905073795473));
#51853=CARTESIAN_POINT('Ctrl Pts',(14.8850257311365,-0.306190019513209,
3.65951122309406));
#51854=CARTESIAN_POINT('Ctrl Pts',(14.8771543590866,-0.362302984784554,
3.70997170823338));
#51855=CARTESIAN_POINT('Ctrl Pts',(14.8692829870366,-0.405677022841909,
3.77459810953617));
#51856=CARTESIAN_POINT('Ctrl Pts',(14.8614116149867,-0.431114693744839,
3.84564633596564));
#51857=CARTESIAN_POINT('Ctrl Pts',(14.8535402429367,-0.45655236464777,3.91669456239511));
#51858=CARTESIAN_POINT('Ctrl Pts',(14.8456688708867,-0.464053668396277,
3.99416461395126));
#51859=CARTESIAN_POINT('Ctrl Pts',(14.8377974988368,-0.452719732759917,
4.06877337558629));
#51860=CARTESIAN_POINT('Ctrl Pts',(14.8299261267868,-0.441385797123556,
4.14338213722132));
#51861=CARTESIAN_POINT('Ctrl Pts',(14.8220547547369,-0.411216622102327,
4.21512960893523));
#51862=CARTESIAN_POINT('Ctrl Pts',(14.8141833826869,-0.365827335221939,
4.27541839855419));
#51863=CARTESIAN_POINT('Ctrl Pts',(14.806312010637,-0.32043804834155,4.33570718817315));
#51864=CARTESIAN_POINT('Ctrl Pts',(14.798440638587,-0.259828649602004,4.38453729569717));
#51865=CARTESIAN_POINT('Ctrl Pts',(14.7905692665371,-0.191261870645823,
4.41605748429924));
#51866=CARTESIAN_POINT('Ctrl Pts',(14.7837114138531,-0.131523763221734,
4.44351912740692));
#51867=CARTESIAN_POINT('Ctrl Pts',(14.7768535611691,-0.065745536276614,
4.45784152413683));
#51868=CARTESIAN_POINT('Ctrl Pts',(14.7699957084852,8.6346448269735E-6,
4.45789857801605));
#51869=CARTESIAN_POINT('Ctrl Pts',(12.5,0.310062960217722,4.54266560670548));
#51870=CARTESIAN_POINT('Ctrl Pts',(12.50787137205,0.220600394030941,4.59378185169648));
#51871=CARTESIAN_POINT('Ctrl Pts',(12.5236141161499,0.0159878432799406,
4.65085692712531));
#51872=CARTESIAN_POINT('Ctrl Pts',(12.5472282322997,-0.294892507759568,
4.580447501361));
#51873=CARTESIAN_POINT('Ctrl Pts',(12.5708423484496,-0.535054221536356,
4.37092866956447));
#51874=CARTESIAN_POINT('Ctrl Pts',(12.5944564645995,-0.647009713430093,
4.07251155115386));
#51875=CARTESIAN_POINT('Ctrl Pts',(12.6180705807493,-0.603894380709874,
3.75671714932517));
#51876=CARTESIAN_POINT('Ctrl Pts',(12.6416846968992,-0.416056506175611,
3.49922677321964));
#51877=CARTESIAN_POINT('Ctrl Pts',(12.6652988130491,-0.128505496873939,
3.36175035317655));
#51878=CARTESIAN_POINT('Ctrl Pts',(12.6889129291989,0.189841674427298,3.37723482234205));
#51879=CARTESIAN_POINT('Ctrl Pts',(12.7125270453488,0.462692468193658,3.54196933898577));
#51880=CARTESIAN_POINT('Ctrl Pts',(12.7361411614987,0.624655556881011,3.81647407445394));
#51881=CARTESIAN_POINT('Ctrl Pts',(12.7597552776485,0.636915702199809,4.13496208375113));
#51882=CARTESIAN_POINT('Ctrl Pts',(12.7833693937984,0.496534514683115,4.42110548633398));
#51883=CARTESIAN_POINT('Ctrl Pts',(12.8069835099483,0.237155397994168,4.60632802944461));
#51884=CARTESIAN_POINT('Ctrl Pts',(12.8305976260981,-0.0790596718614395,
4.64623983861064));
#51885=CARTESIAN_POINT('Ctrl Pts',(12.854211742248,-0.376327535803878,4.5312757721487));
#51886=CARTESIAN_POINT('Ctrl Pts',(12.8778258583979,-0.583405888470749,
4.28898776831928));
#51887=CARTESIAN_POINT('Ctrl Pts',(12.9014399745477,-0.650666957548692,
3.97744183415536));
#51888=CARTESIAN_POINT('Ctrl Pts',(12.9250540906976,-0.561991161265395,
3.67130212143154));
#51889=CARTESIAN_POINT('Ctrl Pts',(12.9486682068475,-0.338630270727757,
3.44393714350224));
#51890=CARTESIAN_POINT('Ctrl Pts',(12.9722823229973,-0.0341142786054444,
3.34983650006563));
#51891=CARTESIAN_POINT('Ctrl Pts',(12.9958964391472,0.278577437919422,3.41155206540036));
#51892=CARTESIAN_POINT('Ctrl Pts',(13.0195105552971,0.524506132150044,3.61429327464512));
#51893=CARTESIAN_POINT('Ctrl Pts',(13.0431246714469,0.644733280558021,3.90947178565704));
#51894=CARTESIAN_POINT('Ctrl Pts',(13.0667387875968,0.61044561006836,4.22634601343335));
#51895=CARTESIAN_POINT('Ctrl Pts',(13.0903529037467,0.429860399609997,4.4889748434194));
#51896=CARTESIAN_POINT('Ctrl Pts',(13.1139670198965,0.146256151980267,4.63441744826062));
#51897=CARTESIAN_POINT('Ctrl Pts',(13.1375811360464,-0.172399400609521,
4.62781749523177));
#51898=CARTESIAN_POINT('Ctrl Pts',(13.1611952521963,-0.449738236712957,
4.47075670902068));
#51899=CARTESIAN_POINT('Ctrl Pts',(13.1848093683461,-0.619294173608025,
4.2008758003961));
#51900=CARTESIAN_POINT('Ctrl Pts',(13.208423484496,-0.64043195068177,3.88285360784221));
#51901=CARTESIAN_POINT('Ctrl Pts',(13.2320376006459,-0.508085752511173,
3.59290636366459));
#51902=CARTESIAN_POINT('Ctrl Pts',(13.2556517167957,-0.253973266794505,
3.40052194335125));
#51903=CARTESIAN_POINT('Ctrl Pts',(13.2792658329456,0.0610056803032868,
3.3518066124833));
#51904=CARTESIAN_POINT('Ctrl Pts',(13.3028799490955,0.361364191435218,3.45843533922715));
#51905=CARTESIAN_POINT('Ctrl Pts',(13.3264940652453,0.575119258511334,3.69485380694));
#51906=CARTESIAN_POINT('Ctrl Pts',(13.3501081813952,0.65104299168552,4.00440268404554));
#51907=CARTESIAN_POINT('Ctrl Pts',(13.3737222975451,0.570939739771795,4.31289642727099));
#51908=CARTESIAN_POINT('Ctrl Pts',(13.3973364136949,0.354006804717113,4.54640236352309));
#51909=CARTESIAN_POINT('Ctrl Pts',(13.4209505298448,0.0522336745508671,
4.6489591696652));
#51910=CARTESIAN_POINT('Ctrl Pts',(13.4445646459947,-0.26205761933777,4.59598839317277));
#51911=CARTESIAN_POINT('Ctrl Pts',(13.4681787621445,-0.513544980480383,
4.40018484937968));
#51912=CARTESIAN_POINT('Ctrl Pts',(13.4917928782944,-0.64195771209056,4.10847422061066));
#51913=CARTESIAN_POINT('Ctrl Pts',(13.5154069944443,-0.616520809113462,
3.79076698974655));
#51914=CARTESIAN_POINT('Ctrl Pts',(13.5390211105941,-0.443330402422436,
3.52320390633144));
#51915=CARTESIAN_POINT('Ctrl Pts',(13.562635226744,-0.163892778617988,3.36990832590288));
#51916=CARTESIAN_POINT('Ctrl Pts',(13.5862493428939,0.154822890495328,3.36761860145296));
#51917=CARTESIAN_POINT('Ctrl Pts',(13.6098634590437,0.43643417612693,3.51688348138565));
#51918=CARTESIAN_POINT('Ctrl Pts',(13.6334775751936,0.613450973283793,3.78193059814177));
#51919=CARTESIAN_POINT('Ctrl Pts',(13.6570916913435,0.643449974253473,4.09923956510808));
#51920=CARTESIAN_POINT('Ctrl Pts',(13.6807058074933,0.519241709620395,4.39276507945606));
#51921=CARTESIAN_POINT('Ctrl Pts',(13.7043199236432,0.270593554659618,4.59216170834183));
#51922=CARTESIAN_POINT('Ctrl Pts',(13.7279340397931,-0.0429042293685969,
4.64964266158552));
#51923=CARTESIAN_POINT('Ctrl Pts',(13.7515481559429,-0.346119716157775,
4.55143222859795));
#51924=CARTESIAN_POINT('Ctrl Pts',(13.7751622720928,-0.566385203513325,
4.32106722332061));
#51925=CARTESIAN_POINT('Ctrl Pts',(13.7987763882427,-0.650912534047929,
4.01375622291695));
#51926=CARTESIAN_POINT('Ctrl Pts',(13.8223905043925,-0.57944414457563,3.70314844792952));
#51927=CARTESIAN_POINT('Ctrl Pts',(13.8460046205424,-0.369107932149097,
3.46368321387984));
#51928=CARTESIAN_POINT('Ctrl Pts',(13.8696187366923,-0.0703124342978696,
3.35275003110641));
#51929=CARTESIAN_POINT('Ctrl Pts',(13.8932328528421,0.245333927901481,3.3969348091043));
#51930=CARTESIAN_POINT('Ctrl Pts',(13.916846968992,0.502184306426786,3.58564835824111));
#51931=CARTESIAN_POINT('Ctrl Pts',(13.9404610851419,0.638682720042094,3.87366416276737));
#51932=CARTESIAN_POINT('Ctrl Pts',(13.9640752012917,0.62211637371287,4.19195723015293));
#51933=CARTESIAN_POINT('Ctrl Pts',(13.9876893174416,0.456455507660852,4.46424641105313));
#51934=CARTESIAN_POINT('Ctrl Pts',(14.0113034335915,0.181401901656729,4.62527570776815));
#51935=CARTESIAN_POINT('Ctrl Pts',(14.0349175497413,-0.137125932879425,
4.63645332836083));
#51936=CARTESIAN_POINT('Ctrl Pts',(14.0585316658912,-0.422790583021024,
4.49510047824495));
#51937=CARTESIAN_POINT('Ctrl Pts',(14.0821457820411,-0.60713052675338,4.23509335195577));
#51938=CARTESIAN_POINT('Ctrl Pts',(14.1057598981909,-0.645967413308333,
3.91874446730605));
#51939=CARTESIAN_POINT('Ctrl Pts',(14.1293740143408,-0.529993712466286,
3.62186903671368));
#51940=CARTESIAN_POINT('Ctrl Pts',(14.1529881304907,-0.287003328966194,
3.41561532377041));
#51941=CARTESIAN_POINT('Ctrl Pts',(14.1766022466405,0.0247694002478971,
3.34941346658496));
#51942=CARTESIAN_POINT('Ctrl Pts',(14.2002163627904,0.330605970264406,3.43912920108534));
#51943=CARTESIAN_POINT('Ctrl Pts',(14.2238304789403,0.557210518047066,3.66326152695696));
#51944=CARTESIAN_POINT('Ctrl Pts',(14.2474445950901,0.650275686248857,3.96809557204375));
#51945=CARTESIAN_POINT('Ctrl Pts',(14.27105871124,0.587497759452106,4.28057573538778));
#51946=CARTESIAN_POINT('Ctrl Pts',(14.2946728273899,0.383921904832036,4.52581397056352));
#51947=CARTESIAN_POINT('Ctrl Pts',(14.3182869435397,0.088336493108731,4.64503722732482));
#51948=CARTESIAN_POINT('Ctrl Pts',(14.3419010596896,-0.22841937412829,4.6096728222354));
#51949=CARTESIAN_POINT('Ctrl Pts',(14.3655151758395,-0.490432948250941,
4.42819608115853));
#51950=CARTESIAN_POINT('Ctrl Pts',(14.3891292919893,-0.634910852255616,
4.14409916841427));
#51951=CARTESIAN_POINT('Ctrl Pts',(14.4127434081392,-0.627227950688033,
3.82546788683648));
#51952=CARTESIAN_POINT('Ctrl Pts',(14.4363575242891,-0.469225504392149,
3.54866444115539));
#51953=CARTESIAN_POINT('Ctrl Pts',(14.4599716404389,-0.198769899531221,
3.38002670405092));
#51954=CARTESIAN_POINT('Ctrl Pts',(14.4835857565888,0.11932229545683,3.35996988316441));
#51955=CARTESIAN_POINT('Ctrl Pts',(14.5071998727387,0.408818071695872,3.49330073524378));
#51956=CARTESIAN_POINT('Ctrl Pts',(14.5308139888885,0.600337751131954,3.74806559342675));
#51957=CARTESIAN_POINT('Ctrl Pts',(14.5544281050384,0.647982309355475,4.06320828594604));
#51958=CARTESIAN_POINT('Ctrl Pts',(14.5780422211883,0.540333396317157,4.36320267272319));
#51959=CARTESIAN_POINT('Ctrl Pts',(14.6016563373381,0.303189823409542,4.57615301060753));
#51960=CARTESIAN_POINT('Ctrl Pts',(14.625270453488,-0.00661530128860875,
4.65102426869959));
#51961=CARTESIAN_POINT('Ctrl Pts',(14.6488845696379,-0.314835022974042,
4.56987302880665));
#51962=CARTESIAN_POINT('Ctrl Pts',(14.6724986857877,-0.547602339746838,
4.35214775046202));
#51963=CARTESIAN_POINT('Ctrl Pts',(14.6961128019376,-0.649132943719538,
4.05002781234082));
#51964=CARTESIAN_POINT('Ctrl Pts',(14.7197269180875,-0.595094318970103,
3.73591836064326));
#51965=CARTESIAN_POINT('Ctrl Pts',(14.7433410342373,-0.398437197867616,
3.48509791236843));
#51966=CARTESIAN_POINT('Ctrl Pts',(14.7669551503872,-0.1062918289807,3.35767733339665));
#51967=CARTESIAN_POINT('Ctrl Pts',(14.7905692665371,0.211327117384507,3.38419385377023));
#51968=CARTESIAN_POINT('Ctrl Pts',(14.8141833826869,0.478300047385911,3.5582926020622));
#51969=CARTESIAN_POINT('Ctrl Pts',(14.8377974988368,0.630645044771057,3.83824960712979));
#51970=CARTESIAN_POINT('Ctrl Pts',(14.8614116149867,0.631851559871185,4.15697121131127));
#51971=CARTESIAN_POINT('Ctrl Pts',(14.8850257311365,0.481630465478622,4.4380735902585));
#51972=CARTESIAN_POINT('Ctrl Pts',(14.9086398472864,0.215983244330552,4.61418854455152));
#51973=CARTESIAN_POINT('Ctrl Pts',(14.9322539634363,-0.101425794369151,
4.64310902247508));
#51974=CARTESIAN_POINT('Ctrl Pts',(14.9558680795861,-0.394527586443172,
4.517903766532));
#51975=CARTESIAN_POINT('Ctrl Pts',(14.979482195736,-0.593077772790822,4.26857965265179));
#51976=CARTESIAN_POINT('Ctrl Pts',(15.0030963118859,-0.649493436571599,
3.95488773069898));
#51977=CARTESIAN_POINT('Ctrl Pts',(15.0267104280357,-0.550252000240565,
3.65200904506483));
#51978=CARTESIAN_POINT('Ctrl Pts',(15.0503245441856,-0.319142060764588,
3.43252503194012));
#51979=CARTESIAN_POINT('Ctrl Pts',(15.0739386603355,-0.0115409051696555,
3.34904846156061));
#51980=CARTESIAN_POINT('Ctrl Pts',(15.0975527764853,0.298810377697559,3.42155963907315));
#51981=CARTESIAN_POINT('Ctrl Pts',(15.1211668926352,0.537575400322941,3.63273573589665));
#51982=CARTESIAN_POINT('Ctrl Pts',(15.1369096367351,0.610790903144771,3.83214323401692));
#51983=CARTESIAN_POINT('Ctrl Pts',(15.1447810087851,0.621570310124627,3.93461384266089));
#51984=CARTESIAN_POINT('Ctrl Pts',(12.4850729970716,0.282426015030316,4.49429601229446));
#51985=CARTESIAN_POINT('Ctrl Pts',(12.4929443691216,0.200937545576316,4.54085609598193));
#51986=CARTESIAN_POINT('Ctrl Pts',(12.5086871132215,0.0145627935155885,
4.59284387968754));
#51987=CARTESIAN_POINT('Ctrl Pts',(12.5323012293714,-0.268607755567932,
4.52871028073968));
#51988=CARTESIAN_POINT('Ctrl Pts',(12.5559153455213,-0.487363055256749,
4.3378665608173));
#51989=CARTESIAN_POINT('Ctrl Pts',(12.5795294616711,-0.589339580973024,
4.06604835489435));
#51990=CARTESIAN_POINT('Ctrl Pts',(12.603143577821,-0.550067261575934,3.77840176074865));
#51991=CARTESIAN_POINT('Ctrl Pts',(12.6267576939709,-0.378972002925158,
3.54386236016666));
#51992=CARTESIAN_POINT('Ctrl Pts',(12.6503718101207,-0.117051373585908,
3.41863967169675));
#51993=CARTESIAN_POINT('Ctrl Pts',(12.6739859262706,0.172920453180012,3.43274395851062));
#51994=CARTESIAN_POINT('Ctrl Pts',(12.6976000424204,0.42145114619533,3.58279513857084));
#51995=CARTESIAN_POINT('Ctrl Pts',(12.7212141585703,0.568977924911017,3.83283235195095));
#51996=CARTESIAN_POINT('Ctrl Pts',(12.7448282747202,0.580145282610399,4.12293246335278));
#51997=CARTESIAN_POINT('Ctrl Pts',(12.76844239087,0.45227673827436,4.38357095065208));
#51998=CARTESIAN_POINT('Ctrl Pts',(12.7920565070199,0.216016946852954,4.55228399108678));
#51999=CARTESIAN_POINT('Ctrl Pts',(12.8156706231698,-0.0720128197761896,
4.58863832766248));
#52000=CARTESIAN_POINT('Ctrl Pts',(12.8392847393196,-0.34278420811256,4.48392139165784));
#52001=CARTESIAN_POINT('Ctrl Pts',(12.8628988554695,-0.531404976945056,
4.26322932523642));
#52002=CARTESIAN_POINT('Ctrl Pts',(12.8865129716194,-0.592670842732518,
3.97945251867098));
#52003=CARTESIAN_POINT('Ctrl Pts',(12.9101270877692,-0.51189901575794,3.70060005900794));
#52004=CARTESIAN_POINT('Ctrl Pts',(12.9337412039191,-0.308447025930223,
3.49350087944474));
#52005=CARTESIAN_POINT('Ctrl Pts',(12.957355320069,-0.0310735592390789,
3.40778774002645));
#52006=CARTESIAN_POINT('Ctrl Pts',(12.9809694362188,0.253746902286204,3.46400239130434));
#52007=CARTESIAN_POINT('Ctrl Pts',(13.0045835523687,0.477755152237737,3.64867260076509));
#52008=CARTESIAN_POINT('Ctrl Pts',(13.0281976685186,0.587266054150949,3.91754086716214));
#52009=CARTESIAN_POINT('Ctrl Pts',(13.0518117846685,0.556034558024266,4.20617103876933));
#52010=CARTESIAN_POINT('Ctrl Pts',(13.0754259008183,0.391545509324759,4.44539088570928));
#52011=CARTESIAN_POINT('Ctrl Pts',(13.0990400169682,0.133219853633759,4.57786970637232));
#52012=CARTESIAN_POINT('Ctrl Pts',(13.122654133118,-0.157032867368526,4.57185802915678));
#52013=CARTESIAN_POINT('Ctrl Pts',(13.1462682492679,-0.409651568547275,
4.42879659435664));
#52014=CARTESIAN_POINT('Ctrl Pts',(13.1698823654178,-0.564094419600429,
4.1829710707208));
#52015=CARTESIAN_POINT('Ctrl Pts',(13.1934964815676,-0.583348116144335,
3.89329525626321));
#52016=CARTESIAN_POINT('Ctrl Pts',(13.2171105977175,-0.462798375770677,
3.62919197644995));
#52017=CARTESIAN_POINT('Ctrl Pts',(13.2407247138674,-0.231335782947555,
3.45395542080054));
#52018=CARTESIAN_POINT('Ctrl Pts',(13.2643388300172,0.055568040665587,3.40958224975729));
#52019=CARTESIAN_POINT('Ctrl Pts',(13.2879529461671,0.329154596505292,3.50670680265737));
#52020=CARTESIAN_POINT('Ctrl Pts',(13.311567062317,0.523856961936024,3.72205250428141));
#52021=CARTESIAN_POINT('Ctrl Pts',(13.3351811784668,0.593013359693284,4.00401025814095));
#52022=CARTESIAN_POINT('Ctrl Pts',(13.3587952946167,0.520049977633468,4.28500692572024));
#52023=CARTESIAN_POINT('Ctrl Pts',(13.3824094107666,0.322452998189994,4.49769969952106));
#52024=CARTESIAN_POINT('Ctrl Pts',(13.4060235269164,0.0475779130258999,
4.59111527567571));
#52025=CARTESIAN_POINT('Ctrl Pts',(13.4296376430663,-0.238699550200797,
4.5428659610613));
#52026=CARTESIAN_POINT('Ctrl Pts',(13.4532517592162,-0.467771004553565,
4.36451503980497));
#52027=CARTESIAN_POINT('Ctrl Pts',(13.476865875366,-0.584737881352888,4.09880555174689));
#52028=CARTESIAN_POINT('Ctrl Pts',(13.5004799915159,-0.561568254327815,
3.80941662539381));
#52029=CARTESIAN_POINT('Ctrl Pts',(13.5240941076658,-0.403814885886516,
3.56570233148043));
#52030=CARTESIAN_POINT('Ctrl Pts',(13.5477082238157,-0.149284468950505,
3.42607049712074));
#52031=CARTESIAN_POINT('Ctrl Pts',(13.5713223399655,0.141023010189178,3.42398486344345));
#52032=CARTESIAN_POINT('Ctrl Pts',(13.5949364561154,0.39753334322815,3.55994526707815));
#52033=CARTESIAN_POINT('Ctrl Pts',(13.6185505722652,0.55877204319843,3.8013678508274));
#52034=CARTESIAN_POINT('Ctrl Pts',(13.6421646884151,0.586097133215014,4.09039401187145));
#52035=CARTESIAN_POINT('Ctrl Pts',(13.665778804565,0.47295996523623,4.35775661870721));
#52036=CARTESIAN_POINT('Ctrl Pts',(13.6893929207148,0.24647464915429,4.53938036140496));
#52037=CARTESIAN_POINT('Ctrl Pts',(13.7130070368647,-0.0390800323908759,
4.59173784568287));
#52038=CARTESIAN_POINT('Ctrl Pts',(13.7366211530146,-0.315268912124245,
4.50228123595558));
#52039=CARTESIAN_POINT('Ctrl Pts',(13.7602352691644,-0.515901402373503,
4.29244943148197));
#52040=CARTESIAN_POINT('Ctrl Pts',(13.7838493853143,-0.59289453017979,4.01253008491428));
#52041=CARTESIAN_POINT('Ctrl Pts',(13.8074635014642,-0.527796356489121,
3.72960781627073));
#52042=CARTESIAN_POINT('Ctrl Pts',(13.831077617614,-0.336208111796874,3.51148691674935));
#52043=CARTESIAN_POINT('Ctrl Pts',(13.8546917337639,-0.0640452526541193,
3.4104415783338));
#52044=CARTESIAN_POINT('Ctrl Pts',(13.8783058499138,0.223466497127862,3.45068801978614));
#52045=CARTESIAN_POINT('Ctrl Pts',(13.9019199660636,0.457422945247278,3.62258090124322));
#52046=CARTESIAN_POINT('Ctrl Pts',(13.9255340822135,0.581754800262342,3.88492489705937));
#52047=CARTESIAN_POINT('Ctrl Pts',(13.9491481983634,0.566665067602596,4.17484744237197));
#52048=CARTESIAN_POINT('Ctrl Pts',(13.9727623145132,0.415770106744681,4.42286658094793));
#52049=CARTESIAN_POINT('Ctrl Pts',(13.9963764306631,0.165232945489059,4.56954279968241));
#52050=CARTESIAN_POINT('Ctrl Pts',(14.019990546813,-0.124903441395439,4.57972412169294));
#52051=CARTESIAN_POINT('Ctrl Pts',(14.0436046629628,-0.385105849054417,
4.45097052228405));
#52052=CARTESIAN_POINT('Ctrl Pts',(14.0672187791127,-0.553014959135429,
4.21413869785145));
#52053=CARTESIAN_POINT('Ctrl Pts',(14.0908328952626,-0.58839018453545,3.92598704378684));
#52054=CARTESIAN_POINT('Ctrl Pts',(14.1144470114124,-0.482753606228458,
3.65557310990793));
#52055=CARTESIAN_POINT('Ctrl Pts',(14.1380611275623,-0.261421765577673,
3.46770347791168));
#52056=CARTESIAN_POINT('Ctrl Pts',(14.1616752437122,0.0225616210391343,
3.40740241293002));
#52057=CARTESIAN_POINT('Ctrl Pts',(14.185289359862,0.301137958114838,3.48912148496193));
#52058=CARTESIAN_POINT('Ctrl Pts',(14.2089034760119,0.507544487205137,3.69327614952086));
#52059=CARTESIAN_POINT('Ctrl Pts',(14.2325175921618,0.592314446747875,3.97093932005559));
#52060=CARTESIAN_POINT('Ctrl Pts',(14.2561317083116,0.535132125826274,4.25556708484021));
#52061=CARTESIAN_POINT('Ctrl Pts',(14.2797458244615,0.349701665714674,4.47894641865396));
#52062=CARTESIAN_POINT('Ctrl Pts',(14.3033599406114,0.0804627670229728,
4.58754290912926));
#52063=CARTESIAN_POINT('Ctrl Pts',(14.3269740567612,-0.208059593914322,
4.55533065134682));
#52064=CARTESIAN_POINT('Ctrl Pts',(14.3505881729111,-0.44671902479684,4.39002953712461));
#52065=CARTESIAN_POINT('Ctrl Pts',(14.374202289061,-0.578319131624566,4.13125512920294));
#52066=CARTESIAN_POINT('Ctrl Pts',(14.3978164052108,-0.571321032683373,
3.84102451585645));
#52067=CARTESIAN_POINT('Ctrl Pts',(14.4214305213607,-0.427401871100662,
3.58889348396707));
#52068=CARTESIAN_POINT('Ctrl Pts',(14.4450446375106,-0.181052875819672,
3.43528699049651));
#52069=CARTESIAN_POINT('Ctrl Pts',(14.4686587536604,0.108686701521778,3.41701790091169));
#52070=CARTESIAN_POINT('Ctrl Pts',(14.4922728698103,0.372378754238714,3.53846452970905));
#52071=CARTESIAN_POINT('Ctrl Pts',(14.5158869859602,0.546827646247725,3.77052134686598));
#52072=CARTESIAN_POINT('Ctrl Pts',(14.53950110211,0.59022548618159,4.05757432072539));
#52073=CARTESIAN_POINT('Ctrl Pts',(14.5631152182599,0.492171679592087,4.3308292078278));
#52074=CARTESIAN_POINT('Ctrl Pts',(14.5867293344098,0.276165503816305,4.52479857226205));
#52075=CARTESIAN_POINT('Ctrl Pts',(14.6103434505596,-0.00602565743375084,
4.59299630554951));
#52076=CARTESIAN_POINT('Ctrl Pts',(14.6339575667095,-0.286772727926288,
4.51907834617235));
#52077=CARTESIAN_POINT('Ctrl Pts',(14.6575716828594,-0.49879271786407,4.32075964763751));
#52078=CARTESIAN_POINT('Ctrl Pts',(14.6811857990092,-0.591273560669336,
4.04556866666751));
#52079=CARTESIAN_POINT('Ctrl Pts',(14.7047999151591,-0.542051578672567,
3.75945683743125));
#52080=CARTESIAN_POINT('Ctrl Pts',(14.728414031309,-0.362923162297683,3.53099285177933));
#52081=CARTESIAN_POINT('Ctrl Pts',(14.7520281474588,-0.0968176839575538,
3.41492969374656));
#52082=CARTESIAN_POINT('Ctrl Pts',(14.7756422636087,0.192490826988301,3.43908270827084));
#52083=CARTESIAN_POINT('Ctrl Pts',(14.7992563797586,0.435667569828913,3.59766345479839));
#52084=CARTESIAN_POINT('Ctrl Pts',(14.8228704959084,0.574433549780463,3.85266695881428));
#52085=CARTESIAN_POINT('Ctrl Pts',(14.8464846120583,0.575532524168,4.14297984400973));
#52086=CARTESIAN_POINT('Ctrl Pts',(14.8700987282082,0.438701136655627,4.39902663091346));
#52087=CARTESIAN_POINT('Ctrl Pts',(14.893712844358,0.196731937819222,4.55944387228049));
#52088=CARTESIAN_POINT('Ctrl Pts',(14.9173269605079,-0.0923853752310475,
4.58578657160514));
#52089=CARTESIAN_POINT('Ctrl Pts',(14.9409410766578,-0.359362027571537,
4.47174127747511));
#52090=CARTESIAN_POINT('Ctrl Pts',(14.9645551928076,-0.540214773976066,
4.24464025294543));
#52091=CARTESIAN_POINT('Ctrl Pts',(14.9881693089575,-0.59160192159185,3.95890873763601));
#52092=CARTESIAN_POINT('Ctrl Pts',(15.0117834251074,-0.501206205285789,
3.68302663884805));
#52093=CARTESIAN_POINT('Ctrl Pts',(15.0353975412572,-0.290695865081771,
3.48310596742652));
#52094=CARTESIAN_POINT('Ctrl Pts',(15.0590116574071,-0.0105122258222001,
3.40706994202017));
#52095=CARTESIAN_POINT('Ctrl Pts',(15.082625773557,0.272176412698783,3.47311795657709));
#52096=CARTESIAN_POINT('Ctrl Pts',(15.1062398897068,0.489659512974156,3.66547122397039));
#52097=CARTESIAN_POINT('Ctrl Pts',(15.1219826338067,0.5563490739778,3.84710486709154));
#52098=CARTESIAN_POINT('Ctrl Pts',(15.1298540058567,0.566167676482186,3.94044192881839));
#52099=CARTESIAN_POINT('Ctrl Pts',(12.4701459941433,0.254789069842909,4.44592641788345));
#52100=CARTESIAN_POINT('Ctrl Pts',(12.4780173661933,0.181274697121691,4.48793034026739));
#52101=CARTESIAN_POINT('Ctrl Pts',(12.4937601102932,0.0131377437512366,
4.53483083224977));
#52102=CARTESIAN_POINT('Ctrl Pts',(12.517374226443,-0.242323003376296,4.47697306011837));
#52103=CARTESIAN_POINT('Ctrl Pts',(12.5409883425929,-0.439671888977142,
4.30480445207012));
#52104=CARTESIAN_POINT('Ctrl Pts',(12.5646024587428,-0.531669448515955,
4.05958515863483));
#52105=CARTESIAN_POINT('Ctrl Pts',(12.5882165748926,-0.496240142441994,
3.80008637217214));
#52106=CARTESIAN_POINT('Ctrl Pts',(12.6118306910425,-0.341887499674706,
3.58849794711368));
#52107=CARTESIAN_POINT('Ctrl Pts',(12.6354448071924,-0.105597250297878,
3.47552899021694));
#52108=CARTESIAN_POINT('Ctrl Pts',(12.6590589233422,0.155999231932725,3.4882530946792));
#52109=CARTESIAN_POINT('Ctrl Pts',(12.6826730394921,0.380209824197002,3.62362093815591));
#52110=CARTESIAN_POINT('Ctrl Pts',(12.706287155642,0.513300292941022,3.84919062944795));
#52111=CARTESIAN_POINT('Ctrl Pts',(12.7299012717918,0.52337486302099,4.11090284295443));
#52112=CARTESIAN_POINT('Ctrl Pts',(12.7535153879417,0.408018961865605,4.34603641497018));
#52113=CARTESIAN_POINT('Ctrl Pts',(12.7771295040916,0.194878495711741,4.49823995272895));
#52114=CARTESIAN_POINT('Ctrl Pts',(12.8007436202414,-0.0649659676909401,
4.53103681671432));
#52115=CARTESIAN_POINT('Ctrl Pts',(12.8243577363913,-0.30924088042124,4.43656701116699));
#52116=CARTESIAN_POINT('Ctrl Pts',(12.8479718525412,-0.479404065419363,
4.23747088215356));
#52117=CARTESIAN_POINT('Ctrl Pts',(12.871585968691,-0.534674727916345,3.9814632031866));
#52118=CARTESIAN_POINT('Ctrl Pts',(12.8952000848409,-0.461806870250484,
3.72989799658434));
#52119=CARTESIAN_POINT('Ctrl Pts',(12.9188142009908,-0.278263781132688,
3.54306461538724));
#52120=CARTESIAN_POINT('Ctrl Pts',(12.9424283171406,-0.0280328398727138,
3.46573897998727));
#52121=CARTESIAN_POINT('Ctrl Pts',(12.9660424332905,0.228916366652986,3.51645271720832));
#52122=CARTESIAN_POINT('Ctrl Pts',(12.9896565494404,0.431004172325429,3.68305192688505));
#52123=CARTESIAN_POINT('Ctrl Pts',(13.0132706655902,0.529798827743877,3.92560994866724));
#52124=CARTESIAN_POINT('Ctrl Pts',(13.0368847817401,0.501623505980173,4.1859960641053));
#52125=CARTESIAN_POINT('Ctrl Pts',(13.06049889789,0.353230619039521,4.40180692799916));
#52126=CARTESIAN_POINT('Ctrl Pts',(13.0841130140398,0.120183555287252,4.52132196448402));
#52127=CARTESIAN_POINT('Ctrl Pts',(13.1077271301897,-0.14166633412753,4.51589856308179));
#52128=CARTESIAN_POINT('Ctrl Pts',(13.1313412463396,-0.369564900381594,
4.38683647969259));
#52129=CARTESIAN_POINT('Ctrl Pts',(13.1549553624894,-0.508894665592834,
4.16506634104549));
#52130=CARTESIAN_POINT('Ctrl Pts',(13.1785694786393,-0.5262642816069,3.9037369046842));
#52131=CARTESIAN_POINT('Ctrl Pts',(13.2021835947892,-0.417510999030181,
3.66547758923531));
#52132=CARTESIAN_POINT('Ctrl Pts',(13.225797710939,-0.208698299100604,3.50738889824983));
#52133=CARTESIAN_POINT('Ctrl Pts',(13.2494118270889,0.0501304010278875,
3.46735788703128));
#52134=CARTESIAN_POINT('Ctrl Pts',(13.2730259432388,0.296945001575366,3.55497826608759));
#52135=CARTESIAN_POINT('Ctrl Pts',(13.2966400593886,0.472594665360713,3.74925120162283));
#52136=CARTESIAN_POINT('Ctrl Pts',(13.3202541755385,0.534983727701048,4.00361783223636));
#52137=CARTESIAN_POINT('Ctrl Pts',(13.3438682916884,0.469160215495142,4.25711742416948));
#52138=CARTESIAN_POINT('Ctrl Pts',(13.3674824078382,0.290899191662876,4.44899703551904));
#52139=CARTESIAN_POINT('Ctrl Pts',(13.3910965239881,0.0429221515009326,
4.53327138168622));
#52140=CARTESIAN_POINT('Ctrl Pts',(13.414710640138,-0.215341481063824,4.48974352894983));
#52141=CARTESIAN_POINT('Ctrl Pts',(13.4383247562878,-0.421997028626747,
4.32884523023027));
#52142=CARTESIAN_POINT('Ctrl Pts',(13.4619388724377,-0.527518050615216,
4.08913688288313));
#52143=CARTESIAN_POINT('Ctrl Pts',(13.4855529885876,-0.506615699542168,
3.82806626104107));
#52144=CARTESIAN_POINT('Ctrl Pts',(13.5091671047374,-0.364299369350597,
3.60820075662942));
#52145=CARTESIAN_POINT('Ctrl Pts',(13.5327812208873,-0.134676159283021,
3.48223266833859));
#52146=CARTESIAN_POINT('Ctrl Pts',(13.5563953370372,0.127223129883027,3.48035112543394));
#52147=CARTESIAN_POINT('Ctrl Pts',(13.580009453187,0.35863251032937,3.60300705277064));
#52148=CARTESIAN_POINT('Ctrl Pts',(13.6036235693369,0.504093113113068,3.82080510351303));
#52149=CARTESIAN_POINT('Ctrl Pts',(13.6272376854868,0.528744292176554,4.08154845863482));
#52150=CARTESIAN_POINT('Ctrl Pts',(13.6508518016366,0.426678220852065,4.32274815795836));
#52151=CARTESIAN_POINT('Ctrl Pts',(13.6744659177865,0.222355743648963,4.48659901446809));
#52152=CARTESIAN_POINT('Ctrl Pts',(13.6980800339364,-0.0352558354131549,
4.53383302978021));
#52153=CARTESIAN_POINT('Ctrl Pts',(13.7216941500862,-0.284418108090716,
4.45313024331322));
#52154=CARTESIAN_POINT('Ctrl Pts',(13.7453082662361,-0.465417601233682,
4.26383163964332));
#52155=CARTESIAN_POINT('Ctrl Pts',(13.768922382386,-0.534876526311652,4.01130394691162));
#52156=CARTESIAN_POINT('Ctrl Pts',(13.7925364985358,-0.476148568402614,
3.75606718461195));
#52157=CARTESIAN_POINT('Ctrl Pts',(13.8161506146857,-0.303308291444651,
3.55929061961886));
#52158=CARTESIAN_POINT('Ctrl Pts',(13.8397647308356,-0.0577780710103693,
3.46813312556118));
#52159=CARTESIAN_POINT('Ctrl Pts',(13.8633788469854,0.201599066354243,3.50444123046797));
#52160=CARTESIAN_POINT('Ctrl Pts',(13.8869929631353,0.412661584067771,3.65951344424533));
#52161=CARTESIAN_POINT('Ctrl Pts',(13.9106070792852,0.52482688048259,3.89618563135138));
#52162=CARTESIAN_POINT('Ctrl Pts',(13.934221195435,0.511213761492322,4.157737654591));
#52163=CARTESIAN_POINT('Ctrl Pts',(13.9578353115849,0.375084705828511,4.38148675084272));
#52164=CARTESIAN_POINT('Ctrl Pts',(13.9814494277348,0.149063989321389,4.51380989159668));
#52165=CARTESIAN_POINT('Ctrl Pts',(14.0050635438846,-0.112680949911453,
4.52299491502504));
#52166=CARTESIAN_POINT('Ctrl Pts',(14.0286776600345,-0.347421115087809,
4.40684056632315));
#52167=CARTESIAN_POINT('Ctrl Pts',(14.0522917761844,-0.498899391517477,
4.19318404374712));
#52168=CARTESIAN_POINT('Ctrl Pts',(14.0759058923342,-0.530812955762567,
3.93322962026762));
#52169=CARTESIAN_POINT('Ctrl Pts',(14.0995200084841,-0.435513499990629,
3.68927718310219));
#52170=CARTESIAN_POINT('Ctrl Pts',(14.123134124634,-0.235840202189154,3.51979163205294));
#52171=CARTESIAN_POINT('Ctrl Pts',(14.1467482407838,0.020353841830372,3.46539135927508));
#52172=CARTESIAN_POINT('Ctrl Pts',(14.1703623569337,0.271669945965271,3.53911376883853));
#52173=CARTESIAN_POINT('Ctrl Pts',(14.1939764730836,0.457878456363209,3.72329077208477));
#52174=CARTESIAN_POINT('Ctrl Pts',(14.2175905892334,0.534353207246894,3.97378306806742));
#52175=CARTESIAN_POINT('Ctrl Pts',(14.2412047053833,0.482766492200443,4.23055843429265));
#52176=CARTESIAN_POINT('Ctrl Pts',(14.2648188215332,0.315481426597312,4.4320788667444));
#52177=CARTESIAN_POINT('Ctrl Pts',(14.288432937683,0.0725890409372144,4.53004859093371));
#52178=CARTESIAN_POINT('Ctrl Pts',(14.3120470538329,-0.187699813700353,
4.50098848045824));
#52179=CARTESIAN_POINT('Ctrl Pts',(14.3356611699828,-0.40300510134274,4.35186299309067));
#52180=CARTESIAN_POINT('Ctrl Pts',(14.3592752861326,-0.521727410993515,
4.11841108999162));
#52181=CARTESIAN_POINT('Ctrl Pts',(14.3828894022825,-0.515414114678713,
3.85658114487643));
#52182=CARTESIAN_POINT('Ctrl Pts',(14.4065035184324,-0.385578237809175,
3.62912252677875));
#52183=CARTESIAN_POINT('Ctrl Pts',(14.4301176345822,-0.163335852108122,
3.49054727694211));
#52184=CARTESIAN_POINT('Ctrl Pts',(14.4537317507321,0.0980511075867261,
3.47406591865897));
#52185=CARTESIAN_POINT('Ctrl Pts',(14.477345866882,0.335939436781555,3.58362832417432));
#52186=CARTESIAN_POINT('Ctrl Pts',(14.5009599830318,0.493317541363497,3.79297710030521));
#52187=CARTESIAN_POINT('Ctrl Pts',(14.5245740991817,0.532468663007706,4.05194035550473));
#52188=CARTESIAN_POINT('Ctrl Pts',(14.5481882153316,0.444009962867018,4.2984557429324));
#52189=CARTESIAN_POINT('Ctrl Pts',(14.5718023314814,0.249141184223067,4.47344413391656));
#52190=CARTESIAN_POINT('Ctrl Pts',(14.5954164476313,-0.00543601357889273,
4.53496834239941));
#52191=CARTESIAN_POINT('Ctrl Pts',(14.6190305637812,-0.258710432878536,
4.46828366353805));
#52192=CARTESIAN_POINT('Ctrl Pts',(14.642644679931,-0.449983095981302,4.28937154481299));
#52193=CARTESIAN_POINT('Ctrl Pts',(14.6662587960809,-0.533414177619135,
4.0411095209942));
#52194=CARTESIAN_POINT('Ctrl Pts',(14.6898729122308,-0.489008838375032,
3.78299531421925));
#52195=CARTESIAN_POINT('Ctrl Pts',(14.7134870283806,-0.327409126727749,
3.57688779119022));
#52196=CARTESIAN_POINT('Ctrl Pts',(14.7371011445305,-0.0873435389344073,
3.47218205409647));
#52197=CARTESIAN_POINT('Ctrl Pts',(14.7607152606804,0.173654536592096,3.49397156277145));
#52198=CARTESIAN_POINT('Ctrl Pts',(14.7843293768302,0.393035092271916,3.63703430753458));
#52199=CARTESIAN_POINT('Ctrl Pts',(14.8079434929801,0.518222054789869,3.86708431049878));
#52200=CARTESIAN_POINT('Ctrl Pts',(14.8315576091299,0.519213488464815,4.12898847670818));
#52201=CARTESIAN_POINT('Ctrl Pts',(14.8551717252798,0.395771807832633,4.35997967156842));
#52202=CARTESIAN_POINT('Ctrl Pts',(14.8787858414297,0.177480631307892,4.50469920000947));
#52203=CARTESIAN_POINT('Ctrl Pts',(14.9023999575796,-0.0833449560929437,
4.52846412073519));
#52204=CARTESIAN_POINT('Ctrl Pts',(14.9260140737294,-0.324196468699902,
4.42557878841823));
#52205=CARTESIAN_POINT('Ctrl Pts',(14.9496281898793,-0.487351775161311,
4.22070085323907));
#52206=CARTESIAN_POINT('Ctrl Pts',(14.9732423060292,-0.533710406612102,
3.96292974457304));
#52207=CARTESIAN_POINT('Ctrl Pts',(14.996856422179,-0.452160410331013,3.71404423263127));
#52208=CARTESIAN_POINT('Ctrl Pts',(15.0204705383289,-0.262249669398955,
3.53368690291293));
#52209=CARTESIAN_POINT('Ctrl Pts',(15.0440846544788,-0.0094835464747447,
3.46509142247974));
#52210=CARTESIAN_POINT('Ctrl Pts',(15.0676987706286,0.245542447700007,3.52467627408104));
#52211=CARTESIAN_POINT('Ctrl Pts',(15.0913128867785,0.441743625625371,3.69820671204414));
#52212=CARTESIAN_POINT('Ctrl Pts',(15.1070556308784,0.501907244810829,3.86206650016617));
#52213=CARTESIAN_POINT('Ctrl Pts',(15.1149270029284,0.510765042839744,3.94627001497588));
#52214=CARTESIAN_POINT('Ctrl Pts',(12.4552189912149,0.227152124655503,4.39755682347243));
#52215=CARTESIAN_POINT('Ctrl Pts',(12.4630903632649,0.161611848667067,4.43500458455284));
#52216=CARTESIAN_POINT('Ctrl Pts',(12.4788331073648,0.0117126939868845,
4.476817784812));
#52217=CARTESIAN_POINT('Ctrl Pts',(12.5024472235147,-0.216038251184659,
4.42523583949706));
#52218=CARTESIAN_POINT('Ctrl Pts',(12.5260613396645,-0.391980722697534,
4.27174234332294));
#52219=CARTESIAN_POINT('Ctrl Pts',(12.5496754558144,-0.473999316058885,
4.05312196237532));
#52220=CARTESIAN_POINT('Ctrl Pts',(12.5732895719643,-0.442413023308054,
3.82177098359562));
#52221=CARTESIAN_POINT('Ctrl Pts',(12.5969036881141,-0.304802996424253,
3.6331335340607));
#52222=CARTESIAN_POINT('Ctrl Pts',(12.620517804264,-0.0941431270098475,
3.53241830873714));
#52223=CARTESIAN_POINT('Ctrl Pts',(12.6441319204139,0.139078010685439,3.54376223084778));
#52224=CARTESIAN_POINT('Ctrl Pts',(12.6677460365637,0.338968502198674,3.66444673774097));
#52225=CARTESIAN_POINT('Ctrl Pts',(12.6913601527136,0.457622660971028,3.86554890694496));
#52226=CARTESIAN_POINT('Ctrl Pts',(12.7149742688635,0.46660444343158,4.09887322255608));
#52227=CARTESIAN_POINT('Ctrl Pts',(12.7385883850133,0.36376118545685,4.30850187928827));
#52228=CARTESIAN_POINT('Ctrl Pts',(12.7622025011632,0.173740044570527,4.44419591437112));
#52229=CARTESIAN_POINT('Ctrl Pts',(12.7858166173131,-0.0579191156056905,
4.47343530576616));
#52230=CARTESIAN_POINT('Ctrl Pts',(12.809430733463,-0.275697552729921,4.38921263067613));
#52231=CARTESIAN_POINT('Ctrl Pts',(12.8330448496128,-0.42740315389367,4.2117124390707));
#52232=CARTESIAN_POINT('Ctrl Pts',(12.8566589657627,-0.476678613100171,
3.98347388770222));
#52233=CARTESIAN_POINT('Ctrl Pts',(12.8802730819125,-0.411714724743029,
3.75919593416074));
#52234=CARTESIAN_POINT('Ctrl Pts',(12.9038871980624,-0.248080536335154,
3.59262835132974));
#52235=CARTESIAN_POINT('Ctrl Pts',(12.9275013142123,-0.0249921205063485,
3.52369021994808));
#52236=CARTESIAN_POINT('Ctrl Pts',(12.9511154303621,0.204085831019768,3.5689030431123));
#52237=CARTESIAN_POINT('Ctrl Pts',(12.974729546512,0.384253192413122,3.71743125300502));
#52238=CARTESIAN_POINT('Ctrl Pts',(12.9983436626619,0.472331601336806,3.93367903017235));
#52239=CARTESIAN_POINT('Ctrl Pts',(13.0219577788117,0.44721245393608,4.16582108944128));
#52240=CARTESIAN_POINT('Ctrl Pts',(13.0455718949616,0.314915728754283,4.35822297028905));
#52241=CARTESIAN_POINT('Ctrl Pts',(13.0691860111115,0.107147256940744,4.46477422259573));
#52242=CARTESIAN_POINT('Ctrl Pts',(13.0928001272613,-0.126299800886535,
4.4599390970068));
#52243=CARTESIAN_POINT('Ctrl Pts',(13.1164142434112,-0.329478232215912,
4.34487636502855));
#52244=CARTESIAN_POINT('Ctrl Pts',(13.1400283595611,-0.453694911585238,
4.14716161137019));
#52245=CARTESIAN_POINT('Ctrl Pts',(13.1636424757109,-0.469180447069464,
3.9141785531052));
#52246=CARTESIAN_POINT('Ctrl Pts',(13.1872565918608,-0.372223622289685,
3.70176320202068));
#52247=CARTESIAN_POINT('Ctrl Pts',(13.2108707080107,-0.186060815253654,
3.56082237569912));
#52248=CARTESIAN_POINT('Ctrl Pts',(13.2344848241605,0.0446927613901878,
3.52513352430527));
#52249=CARTESIAN_POINT('Ctrl Pts',(13.2580989403104,0.26473540664544,3.60324972951781));
#52250=CARTESIAN_POINT('Ctrl Pts',(13.2817130564603,0.421332368785403,3.77644989896424));
#52251=CARTESIAN_POINT('Ctrl Pts',(13.3053271726101,0.476954095708811,4.00322540633176));
#52252=CARTESIAN_POINT('Ctrl Pts',(13.32894128876,0.418270453356816,4.22922792261873));
#52253=CARTESIAN_POINT('Ctrl Pts',(13.3525554049099,0.259345385135757,4.40029437151701));
#52254=CARTESIAN_POINT('Ctrl Pts',(13.3761695210597,0.0382663899759653,
4.47542748769673));
#52255=CARTESIAN_POINT('Ctrl Pts',(13.3997836372096,-0.19198341192685,4.43662109683837));
#52256=CARTESIAN_POINT('Ctrl Pts',(13.4233977533595,-0.376223052699929,
4.29317542065556));
#52257=CARTESIAN_POINT('Ctrl Pts',(13.4470118695093,-0.470298219877544,
4.07946821401937));
#52258=CARTESIAN_POINT('Ctrl Pts',(13.4706259856592,-0.451663144756522,
3.84671589668833));
#52259=CARTESIAN_POINT('Ctrl Pts',(13.4942401018091,-0.324783852814677,
3.65069918177841));
#52260=CARTESIAN_POINT('Ctrl Pts',(13.5178542179589,-0.120067849615538,
3.53839483955645));
#52261=CARTESIAN_POINT('Ctrl Pts',(13.5414683341088,0.113423249576877,3.53671738742444));
#52262=CARTESIAN_POINT('Ctrl Pts',(13.5650824502587,0.319731677430589,3.64606883846313));
#52263=CARTESIAN_POINT('Ctrl Pts',(13.5886965664085,0.449414183027706,3.84024235619866));
#52264=CARTESIAN_POINT('Ctrl Pts',(13.6123106825584,0.471391451138094,4.07270290539818));
#52265=CARTESIAN_POINT('Ctrl Pts',(13.6359247987083,0.380396476467901,4.28773969720951));
#52266=CARTESIAN_POINT('Ctrl Pts',(13.6595389148581,0.198236838143636,4.43381766753122));
#52267=CARTESIAN_POINT('Ctrl Pts',(13.683153031008,-0.0314316384354341,
4.47592821387755));
#52268=CARTESIAN_POINT('Ctrl Pts',(13.7067671471579,-0.253567304057185,
4.40397925067086));
#52269=CARTESIAN_POINT('Ctrl Pts',(13.7303812633077,-0.414933800093862,
4.23521384780468));
#52270=CARTESIAN_POINT('Ctrl Pts',(13.7539953794576,-0.476858522443512,
4.01007780890896));
#52271=CARTESIAN_POINT('Ctrl Pts',(13.7776094956075,-0.424500780316106,
3.78252655295316));
#52272=CARTESIAN_POINT('Ctrl Pts',(13.8012236117573,-0.270408471092428,
3.60709432248837));
#52273=CARTESIAN_POINT('Ctrl Pts',(13.8248377279072,-0.0515108893666192,
3.52582467278856));
#52274=CARTESIAN_POINT('Ctrl Pts',(13.8484518440571,0.179731635580624,3.55819444114981));
#52275=CARTESIAN_POINT('Ctrl Pts',(13.8720659602069,0.367900222888263,3.69644598724744));
#52276=CARTESIAN_POINT('Ctrl Pts',(13.8956800763568,0.467898960702838,3.90744636564338));
#52277=CARTESIAN_POINT('Ctrl Pts',(13.9192941925067,0.455762455382048,4.14062786681004));
#52278=CARTESIAN_POINT('Ctrl Pts',(13.9429083086565,0.33439930491234,4.34010692073752));
#52279=CARTESIAN_POINT('Ctrl Pts',(13.9665224248064,0.132895033153719,4.45807698351094));
#52280=CARTESIAN_POINT('Ctrl Pts',(13.9901365409563,-0.100458458427467,
4.46626570835715));
#52281=CARTESIAN_POINT('Ctrl Pts',(14.0137506571061,-0.309736381121202,
4.36271061036225));
#52282=CARTESIAN_POINT('Ctrl Pts',(14.037364773256,-0.444783823899526,4.1722293896428));
#52283=CARTESIAN_POINT('Ctrl Pts',(14.0609788894059,-0.473235726989685,
3.94047219674841));
#52284=CARTESIAN_POINT('Ctrl Pts',(14.0845930055557,-0.388273393752801,
3.72298125629644));
#52285=CARTESIAN_POINT('Ctrl Pts',(14.1082071217056,-0.210258638800633,
3.5718797861942));
#52286=CARTESIAN_POINT('Ctrl Pts',(14.1318212378555,0.0181460626216094,
3.52338030562014));
#52287=CARTESIAN_POINT('Ctrl Pts',(14.1554353540053,0.242201933815703,3.58910605271512));
#52288=CARTESIAN_POINT('Ctrl Pts',(14.1790494701552,0.40821242552128,3.75330539464867));
#52289=CARTESIAN_POINT('Ctrl Pts',(14.2026635863051,0.476391967745912,3.97662681607925));
#52290=CARTESIAN_POINT('Ctrl Pts',(14.2262777024549,0.430400858574612,4.20554978374509));
#52291=CARTESIAN_POINT('Ctrl Pts',(14.2498918186048,0.28126118747995,4.38521131483484));
#52292=CARTESIAN_POINT('Ctrl Pts',(14.2735059347547,0.0647153148514563,
4.47255427273816));
#52293=CARTESIAN_POINT('Ctrl Pts',(14.2971200509045,-0.167340033486385,
4.44664630956965));
#52294=CARTESIAN_POINT('Ctrl Pts',(14.3207341670544,-0.359291177888639,
4.31369644905674));
#52295=CARTESIAN_POINT('Ctrl Pts',(14.3443482832043,-0.465135690362464,
4.10556705078029));
#52296=CARTESIAN_POINT('Ctrl Pts',(14.3679623993541,-0.459507196674052,
3.87213777389641));
#52297=CARTESIAN_POINT('Ctrl Pts',(14.391576515504,-0.343754604517688,3.66935156959044));
#52298=CARTESIAN_POINT('Ctrl Pts',(14.4151906316539,-0.145618828396573,
3.5458075633877));
#52299=CARTESIAN_POINT('Ctrl Pts',(14.4388047478037,0.0874155136516737,
3.53111393640625));
#52300=CARTESIAN_POINT('Ctrl Pts',(14.4624188639536,0.299500119324396,3.6287921186396));
#52301=CARTESIAN_POINT('Ctrl Pts',(14.4860329801035,0.439807436479269,3.81543285374444));
#52302=CARTESIAN_POINT('Ctrl Pts',(14.5096470962533,0.474711839833821,4.04630639028407));
#52303=CARTESIAN_POINT('Ctrl Pts',(14.5332612124032,0.395848246141948,4.26608227803701));
#52304=CARTESIAN_POINT('Ctrl Pts',(14.5568753285531,0.22211686462983,4.42208969557108));
#52305=CARTESIAN_POINT('Ctrl Pts',(14.5804894447029,-0.00484636972403486,
4.47694037924932));
#52306=CARTESIAN_POINT('Ctrl Pts',(14.6041035608528,-0.230648137830783,
4.41748898090375));
#52307=CARTESIAN_POINT('Ctrl Pts',(14.6277176770027,-0.401173474098533,
4.25798344198848));
#52308=CARTESIAN_POINT('Ctrl Pts',(14.6513317931525,-0.475554794568933,
4.03665037532088));
#52309=CARTESIAN_POINT('Ctrl Pts',(14.6749459093024,-0.435966098077497,
3.80653379100725));
#52310=CARTESIAN_POINT('Ctrl Pts',(14.6985600254523,-0.291895091157815,
3.62278273060111));
#52311=CARTESIAN_POINT('Ctrl Pts',(14.7221741416021,-0.077869393911261,
3.52943441444639));
#52312=CARTESIAN_POINT('Ctrl Pts',(14.745788257752,0.15481824619589,3.54886041727207));
#52313=CARTESIAN_POINT('Ctrl Pts',(14.7694023739019,0.350402614714918,3.67640516027076));
#52314=CARTESIAN_POINT('Ctrl Pts',(14.7930164900517,0.462010559799276,3.88150166218328));
#52315=CARTESIAN_POINT('Ctrl Pts',(14.8166306062016,0.46289445276163,4.11499710940664));
#52316=CARTESIAN_POINT('Ctrl Pts',(14.8402447223515,0.352842479009638,4.32093271222338));
#52317=CARTESIAN_POINT('Ctrl Pts',(14.8638588385013,0.158229324796562,4.44995452773844));
#52318=CARTESIAN_POINT('Ctrl Pts',(14.8874729546512,-0.07430453695484,4.47114166986524));
#52319=CARTESIAN_POINT('Ctrl Pts',(14.9110870708011,-0.289030909828268,
4.37941629936134));
#52320=CARTESIAN_POINT('Ctrl Pts',(14.9347011869509,-0.434488776346555,
4.1967614535327));
#52321=CARTESIAN_POINT('Ctrl Pts',(14.9583153031008,-0.475818891632353,
3.96695075151007));
#52322=CARTESIAN_POINT('Ctrl Pts',(14.9819294192507,-0.403114615376237,
3.74506182641449));
#52323=CARTESIAN_POINT('Ctrl Pts',(15.0055435354005,-0.233803473716137,
3.58426783839933));
#52324=CARTESIAN_POINT('Ctrl Pts',(15.0291576515504,-0.00845486712728951,
3.5231129029393));
#52325=CARTESIAN_POINT('Ctrl Pts',(15.0527717677003,0.218908482701231,3.57623459158499));
#52326=CARTESIAN_POINT('Ctrl Pts',(15.0763858838501,0.393827738276586,3.73094220011788));
#52327=CARTESIAN_POINT('Ctrl Pts',(15.09212862795,0.447465415643859,3.87702813324079));
#52328=CARTESIAN_POINT('Ctrl Pts',(15.1,0.455362409197302,3.95209810113337));
#52329=CARTESIAN_POINT('',(15.1,0.455362409197302,3.95209810113338));
#52330=CARTESIAN_POINT('Ctrl Pts',(15.1,0.455362409197302,3.95209810113337));
#52331=CARTESIAN_POINT('Ctrl Pts',(15.1,0.461198486074795,3.93070554260298));
#52332=CARTESIAN_POINT('Ctrl Pts',(15.1,0.46535922191849,3.9089149747703));
#52333=CARTESIAN_POINT('Ctrl Pts',(15.1,0.467933495509747,3.88694781877637));
#52334=CARTESIAN_POINT('Ctrl Pts',(15.1,0.470556099470815,3.86456824322593));
#52335=CARTESIAN_POINT('Ctrl Pts',(15.1,0.471533159003394,3.84200460508655));
#52336=CARTESIAN_POINT('Ctrl Pts',(15.1,0.470938919222204,3.8194389967166));
#52337=CARTESIAN_POINT('Ctrl Pts',(15.1,0.470570970565677,3.80546654730098));
#52338=CARTESIAN_POINT('Ctrl Pts',(15.1,0.469600118414825,3.7914923521806));
#52339=CARTESIAN_POINT('Ctrl Pts',(15.1,0.468037922355437,3.77755218535593));
#52340=CARTESIAN_POINT('Ctrl Pts',(15.1,0.467305764617198,3.77101881782393));
#52341=CARTESIAN_POINT('Ctrl Pts',(15.1,0.466444065557791,3.76449770946228));
#52342=CARTESIAN_POINT('Ctrl Pts',(15.1,0.465455885979624,3.7580011302485));
#52343=CARTESIAN_POINT('Ctrl Pts',(15.1,0.462059294618766,3.73567095330476));
#52344=CARTESIAN_POINT('Ctrl Pts',(15.1,0.45716703427379,3.71360451488159));
#52345=CARTESIAN_POINT('Ctrl Pts',(15.1,0.450855318277529,3.69195899424001));
#52346=CARTESIAN_POINT('Ctrl Pts',(15.1,0.444011336009419,3.66848810937402));
#52347=CARTESIAN_POINT('Ctrl Pts',(15.1,0.435499564516811,3.64551127788848));
#52348=CARTESIAN_POINT('Ctrl Pts',(15.1,0.425460105602329,3.62314791088594));
#52349=CARTESIAN_POINT('Ctrl Pts',(15.1,0.421555366121865,3.61444992000866));
#52350=CARTESIAN_POINT('Ctrl Pts',(15.1,0.417417266816347,3.60584160863805));
#52351=CARTESIAN_POINT('Ctrl Pts',(15.1,0.413065612826793,3.5973533346642));
#52352=CARTESIAN_POINT('Ctrl Pts',(15.1,0.400188909388694,3.57223622128044));
#52353=CARTESIAN_POINT('Ctrl Pts',(15.1,0.385429835973237,3.54813135585314));
#52354=CARTESIAN_POINT('Ctrl Pts',(15.1,0.369010648251791,3.52520488756047));
#52355=CARTESIAN_POINT('Ctrl Pts',(15.1,0.352591460530346,3.50227841926781));
#52356=CARTESIAN_POINT('Ctrl Pts',(15.1,0.334512091502091,3.48052876229398));
#52357=CARTESIAN_POINT('Ctrl Pts',(15.1,0.31493781544227,3.46010549098216));
#52358=CARTESIAN_POINT('Ctrl Pts',(14.8800042915148,-1.01702808208336E-5,
4.45785711824254));
#52359=CARTESIAN_POINT('Ctrl Pts',(14.8824938458936,-0.0238866377941533,
4.45787702641871));
#52360=CARTESIAN_POINT('Ctrl Pts',(14.8849834002724,-0.0477600743578134,
4.45604121816599));
#52361=CARTESIAN_POINT('Ctrl Pts',(14.8874729546512,-0.0713366221418418,
4.45232291776013));
#52362=CARTESIAN_POINT('Ctrl Pts',(14.8953443267012,-0.145879994579315,
4.44056654636394));
#52363=CARTESIAN_POINT('Ctrl Pts',(14.9032156987511,-0.217455452203791,
4.40999142286264));
#52364=CARTESIAN_POINT('Ctrl Pts',(14.9110870708011,-0.277486158769077,
4.36426138680722));
#52365=CARTESIAN_POINT('Ctrl Pts',(14.918958442851,-0.337516865334364,4.31853135075179));
#52366=CARTESIAN_POINT('Ctrl Pts',(14.926829814901,-0.38600282084046,4.25764640214225));
#52367=CARTESIAN_POINT('Ctrl Pts',(14.9347011869509,-0.417134151141141,
4.18890214416703));
#52368=CARTESIAN_POINT('Ctrl Pts',(14.9425725590009,-0.448265481441821,
4.12015788619182));
#52369=CARTESIAN_POINT('Ctrl Pts',(14.9504439310508,-0.462042186537087,
4.04355431885095));
#52370=CARTESIAN_POINT('Ctrl Pts',(14.9583153031008,-0.456813159708701,
3.96827104766458));
#52371=CARTESIAN_POINT('Ctrl Pts',(14.9661866751508,-0.451584132880315,
3.89298777647821));
#52372=CARTESIAN_POINT('Ctrl Pts',(14.9740580472007,-0.427349374128277,
3.81902480144635));
#52373=CARTESIAN_POINT('Ctrl Pts',(14.9819294192507,-0.387013471142241,
3.7552443159279));
#52374=CARTESIAN_POINT('Ctrl Pts',(14.9898007913006,-0.346677568156205,
3.69146383040944));
#52375=CARTESIAN_POINT('Ctrl Pts',(14.9976721633506,-0.290240520936171,
3.63786583440439));
#52376=CARTESIAN_POINT('Ctrl Pts',(15.0055435354005,-0.224463896228013,
3.60087434715852));
#52377=CARTESIAN_POINT('Ctrl Pts',(15.0134149074505,-0.158687271519854,
3.56388285991266));
#52378=CARTESIAN_POINT('Ctrl Pts',(15.0212862795004,-0.0835710693235713,
3.54349788142598));
#52379=CARTESIAN_POINT('Ctrl Pts',(15.0291576515504,-0.00811907658734153,
3.54215900695692));
#52380=CARTESIAN_POINT('Ctrl Pts',(15.0370290236004,0.067332916148885,3.54082013248786));
#52381=CARTESIAN_POINT('Ctrl Pts',(15.0449003956503,0.143120699425059,3.55852736203643));
#52382=CARTESIAN_POINT('Ctrl Pts',(15.0527717677003,0.210167800325704,3.59316557823286));
#52383=CARTESIAN_POINT('Ctrl Pts',(15.0606431397502,0.27721490122635,3.62780379442929));
#52384=CARTESIAN_POINT('Ctrl Pts',(15.0685145118002,0.335521319751467,3.67937299727358));
#52385=CARTESIAN_POINT('Ctrl Pts',(15.0763858838501,0.378083948355844,3.74167908197646));
#52386=CARTESIAN_POINT('Ctrl Pts',(15.0842572559001,0.420646576960222,3.80398516667934));
#52387=CARTESIAN_POINT('Ctrl Pts',(15.09212862795,0.447465415643859,3.87702813324079));
#52388=CARTESIAN_POINT('Ctrl Pts',(15.1,0.455362409197302,3.95209810113337));
#52389=CARTESIAN_POINT('Ctrl Pts',(12.5,0.310062960217722,4.54266560670548));
#52390=CARTESIAN_POINT('Ctrl Pts',(12.5,0.283442099593322,4.54921865641189));
#52391=CARTESIAN_POINT('Ctrl Pts',(12.5,0.256466577744696,4.55390832200786));
#52392=CARTESIAN_POINT('Ctrl Pts',(12.5,0.229324391633413,4.55669460918752));
#52393=CARTESIAN_POINT('Ctrl Pts',(12.5,0.202804350211112,4.55941702996513));
#52394=CARTESIAN_POINT('Ctrl Pts',(12.5,0.176124140498118,4.56032157710196));
#52395=CARTESIAN_POINT('Ctrl Pts',(12.5,0.149491279718871,4.55933465732487));
#52396=CARTESIAN_POINT('Ctrl Pts',(12.5,0.131604301980395,4.55867182909064));
#52397=CARTESIAN_POINT('Ctrl Pts',(12.5,0.113739373486447,4.5571550748263));
#52398=CARTESIAN_POINT('Ctrl Pts',(12.5,0.0959711573489174,4.5547553284502));
#52399=CARTESIAN_POINT('Ctrl Pts',(12.5,0.0885102514788159,4.55374767063663));
#52400=CARTESIAN_POINT('Ctrl Pts',(12.5,0.0810658284660142,4.55258395860043));
#52401=CARTESIAN_POINT('Ctrl Pts',(12.5,0.0736590895785168,4.55126509319275));
#52402=CARTESIAN_POINT('Ctrl Pts',(12.5,0.0532014046082737,4.54762233847462));
#52403=CARTESIAN_POINT('Ctrl Pts',(12.5,0.0329999615976937,4.54279338637244));
#52404=CARTESIAN_POINT('Ctrl Pts',(12.5,0.0131662989716721,4.53674486487483));
#52405=CARTESIAN_POINT('Ctrl Pts',(12.5,-0.00550403753485725,4.53105111411095));
#52406=CARTESIAN_POINT('Ctrl Pts',(12.5,-0.0238485481480196,4.52427602479051));
#52407=CARTESIAN_POINT('Ctrl Pts',(12.5,-0.0417515783368052,4.51643454453567));
#52408=CARTESIAN_POINT('Ctrl Pts',(12.5,-0.0500477299146631,4.51280085190917));
#52409=CARTESIAN_POINT('Ctrl Pts',(12.5,-0.058248775177811,4.50893813195896));
#52410=CARTESIAN_POINT('Ctrl Pts',(12.5,-0.0663415323109863,4.50484786558969));
#52411=CARTESIAN_POINT('Ctrl Pts',(12.5,-0.0727048112135971,4.50163171746301));
#52412=CARTESIAN_POINT('Ctrl Pts',(12.5,-0.0789919703630761,4.49827952355299));
#52413=CARTESIAN_POINT('Ctrl Pts',(12.5,-0.085197598682301,4.4947927546146));
#52414=CARTESIAN_POINT('Ctrl Pts',(12.5,-0.104491803581693,4.48395188067351));
#52415=CARTESIAN_POINT('Ctrl Pts',(12.5,-0.123002674071495,4.47180959856144));
#52416=CARTESIAN_POINT('Ctrl Pts',(12.5,-0.140547257611399,4.45840101528927));
#52417=CARTESIAN_POINT('Ctrl Pts',(12.5,-0.156644205929787,4.44609879839914));
#52418=CARTESIAN_POINT('Ctrl Pts',(12.5,-0.17192740174072,4.43272977950413));
#52419=CARTESIAN_POINT('Ctrl Pts',(12.5,-0.186217277007305,4.41832740439832));
#52420=CARTESIAN_POINT('Origin',(15.1,0.,4.));
#52421=CARTESIAN_POINT('',(15.1,-1.16619037896906,2.5));
#52422=CARTESIAN_POINT('',(15.1,1.16619037896906,2.5));
#52423=CARTESIAN_POINT('',(15.1,1.25,2.5));
#52424=CARTESIAN_POINT('Origin',(15.1,0.,4.));
#52425=CARTESIAN_POINT('Origin',(15.1,0.,4.));
#52426=CARTESIAN_POINT('',(15.1,2.75545529808154E-17,5.725));
#52427=CARTESIAN_POINT('Origin',(15.1,0.,5.5));
#52428=CARTESIAN_POINT('',(15.1,1.5,4.225));
#52429=CARTESIAN_POINT('Origin',(15.1,1.5,4.));
#52430=CARTESIAN_POINT('',(15.1,-1.5,4.225));
#52431=CARTESIAN_POINT('Origin',(15.1,-1.5,4.));
#52432=CARTESIAN_POINT('Origin',(14.4,-1.5,4.));
#52433=CARTESIAN_POINT('',(14.5,-1.5,4.225));
#52434=CARTESIAN_POINT('Origin',(14.5,-1.5,4.));
#52435=CARTESIAN_POINT('',(14.4,-1.5,4.225));
#52436=CARTESIAN_POINT('Origin',(14.4,1.5,4.));
#52437=CARTESIAN_POINT('',(14.5,1.5,4.225));
#52438=CARTESIAN_POINT('Origin',(14.5,1.5,4.));
#52439=CARTESIAN_POINT('',(14.4,1.5,4.225));
#52440=CARTESIAN_POINT('Origin',(14.4,0.,5.5));
#52441=CARTESIAN_POINT('',(14.5,-2.75545529808154E-17,5.725));
#52442=CARTESIAN_POINT('Origin',(14.5,0.,5.5));
#52443=CARTESIAN_POINT('',(14.4,-2.75545529808154E-17,5.725));
#52444=CARTESIAN_POINT('Origin',(14.4,2.5,2.5));
#52445=CARTESIAN_POINT('',(14.5,1.16619037896906,2.5));
#52446=CARTESIAN_POINT('',(14.5,-1.16619037896906,2.5));
#52447=CARTESIAN_POINT('',(14.5,1.25,2.5));
#52448=CARTESIAN_POINT('',(14.5,1.16619037896906,2.5));
#52449=CARTESIAN_POINT('',(14.5,-1.16619037896906,2.5));
#52450=CARTESIAN_POINT('Origin',(14.5,0.,4.));
#52451=CARTESIAN_POINT('Origin',(14.5,0.,4.));
#52452=CARTESIAN_POINT('',(14.5,-1.34711147906209E-16,5.1));
#52453=CARTESIAN_POINT('Origin',(14.5,0.,4.));
#52454=CARTESIAN_POINT('Origin',(14.5,0.,4.));
#52455=CARTESIAN_POINT('Origin',(12.5,0.,4.));
#52456=CARTESIAN_POINT('Origin',(12.5,0.,4.));
#52457=CARTESIAN_POINT('',(12.5,-1.34711147906209E-16,5.1));
#52458=CARTESIAN_POINT('',(12.5,-1.34711147906209E-16,5.1));
#52459=CARTESIAN_POINT('Origin',(12.5,0.,4.));
#52460=CARTESIAN_POINT('Origin',(12.5,0.,4.));
#52461=CARTESIAN_POINT('',(0.,0.,0.));
#52462=CARTESIAN_POINT('Origin',(0.3,0.4,0.));
#52463=CARTESIAN_POINT('',(-0.3,0.4,-3.67394039744206E-17));
#52464=CARTESIAN_POINT('Origin',(0.,0.4,0.));
#52465=CARTESIAN_POINT('Origin',(0.,0.375,0.));
#52466=CARTESIAN_POINT('',(-0.35,0.35,-4.28626379701573E-17));
#52467=CARTESIAN_POINT('Origin',(0.,0.35,0.));
#52468=CARTESIAN_POINT('',(-0.325,0.375,-3.9801020972289E-17));
#52469=CARTESIAN_POINT('Origin',(0.,0.19,0.));
#52470=CARTESIAN_POINT('',(-0.35,0.03,-4.28626379701574E-17));
#52471=CARTESIAN_POINT('Origin',(0.,0.03,0.));
#52472=CARTESIAN_POINT('',(-0.35,0.19,-4.28626379701574E-17));
#52473=CARTESIAN_POINT('Origin',(0.,0.0149999999999999,0.));
#52474=CARTESIAN_POINT('',(-0.32,-3.29597460435593E-17,-3.91886975727153E-17));
#52475=CARTESIAN_POINT('Origin',(0.,0.,0.));
#52476=CARTESIAN_POINT('',(-0.335,0.0149999999999999,-4.10256677714363E-17));
#52477=CARTESIAN_POINT('Origin',(0.22,0.,0.));
#52478=CARTESIAN_POINT('',(-0.22,-6.93889390390723E-18,-2.69422295812418E-17));
#52479=CARTESIAN_POINT('Origin',(0.,0.,0.));
#52480=CARTESIAN_POINT('Origin',(0.,-0.02,0.));
#52481=CARTESIAN_POINT('',(-0.1954,-0.0492,2.39295984553393E-17));
#52482=CARTESIAN_POINT('Origin',(0.,-0.0492,0.));
#52483=CARTESIAN_POINT('',(-0.21,-0.02,-2.57175827820944E-17));
#52484=CARTESIAN_POINT('Origin',(0.,-0.8,0.));
#52485=CARTESIAN_POINT('',(-0.1954,-1.5646,2.39295984553393E-17));
#52486=CARTESIAN_POINT('Origin',(0.,-1.5646,0.));
#52487=CARTESIAN_POINT('',(-0.1954,-0.8,-2.39295984553393E-17));
#52488=CARTESIAN_POINT('Origin',(0.,-1.58,0.));
#52489=CARTESIAN_POINT('',(-0.16,-1.6,-1.95943487863577E-17));
#52490=CARTESIAN_POINT('Origin',(0.,-1.6,0.));
#52491=CARTESIAN_POINT('',(-0.18,-1.58,-2.20436423846524E-17));
#52492=CARTESIAN_POINT('Origin',(0.,-1.6,0.));
#52493=CARTESIAN_POINT('Origin',(0.0866025403784439,-0.4,-0.15));
#52494=CARTESIAN_POINT('',(0.173205080756888,-0.4,0.));
#52495=CARTESIAN_POINT('',(0.0866025403784439,-0.4,-0.15));
#52496=CARTESIAN_POINT('',(0.173205080756888,-0.4,0.));
#52497=CARTESIAN_POINT('',(0.0866025403784439,-0.64,-0.15));
#52498=CARTESIAN_POINT('',(0.0866025403784439,-0.4,-0.15));
#52499=CARTESIAN_POINT('',(0.173205080756888,-0.64,0.));
#52500=CARTESIAN_POINT('',(0.173205080756888,-0.64,0.));
#52501=CARTESIAN_POINT('',(0.173205080756888,-0.4,0.));
#52502=CARTESIAN_POINT('Origin',(-0.0866025403784438,-0.4,-0.15));
#52503=CARTESIAN_POINT('',(-0.0866025403784438,-0.4,-0.15));
#52504=CARTESIAN_POINT('',(0.0866025403784439,-0.4,-0.15));
#52505=CARTESIAN_POINT('',(-0.0866025403784438,-0.64,-0.15));
#52506=CARTESIAN_POINT('',(-0.0866025403784438,-0.4,-0.15));
#52507=CARTESIAN_POINT('',(0.0866025403784439,-0.64,-0.15));
#52508=CARTESIAN_POINT('Origin',(-0.173205080756888,-0.4,-2.77555756156289E-17));
#52509=CARTESIAN_POINT('',(-0.173205080756888,-0.4,-2.12115047744981E-17));
#52510=CARTESIAN_POINT('',(-0.0866025403784438,-0.4,-0.15));
#52511=CARTESIAN_POINT('',(-0.173205080756888,-0.64,-2.77555756156289E-17));
#52512=CARTESIAN_POINT('',(-0.173205080756888,-0.4,-2.12115047744981E-17));
#52513=CARTESIAN_POINT('',(-0.0866025403784438,-0.64,-0.15));
#52514=CARTESIAN_POINT('Origin',(-0.0866025403784439,-0.4,0.15));
#52515=CARTESIAN_POINT('',(-0.0866025403784439,-0.4,0.15));
#52516=CARTESIAN_POINT('',(-0.173205080756888,-0.4,-2.12115047744981E-17));
#52517=CARTESIAN_POINT('',(-0.0866025403784439,-0.64,0.15));
#52518=CARTESIAN_POINT('',(-0.0866025403784439,-0.4,0.15));
#52519=CARTESIAN_POINT('',(-0.173205080756888,-0.64,-2.12115047744981E-17));
#52520=CARTESIAN_POINT('Origin',(0.0866025403784439,-0.4,0.15));
#52521=CARTESIAN_POINT('',(0.0866025403784439,-0.4,0.15));
#52522=CARTESIAN_POINT('',(-0.0866025403784439,-0.4,0.15));
#52523=CARTESIAN_POINT('',(0.0866025403784439,-0.64,0.15));
#52524=CARTESIAN_POINT('',(0.0866025403784439,-0.4,0.15));
#52525=CARTESIAN_POINT('',(-0.0866025403784439,-0.64,0.15));
#52526=CARTESIAN_POINT('Origin',(0.173205080756888,-0.4,0.));
#52527=CARTESIAN_POINT('',(0.0866025403784439,-0.4,0.15));
#52528=CARTESIAN_POINT('',(0.0866025403784439,-0.64,0.15));
#52529=CARTESIAN_POINT('Origin',(0.,-0.4,-2.77555756156289E-17));
#52530=CARTESIAN_POINT('Origin',(0.,-0.64,-2.77555756156289E-17));
#52531=CARTESIAN_POINT('',(0.,0.,0.));
#52532=CARTESIAN_POINT('Origin',(0.375,0.5,0.));
#52533=CARTESIAN_POINT('',(-0.375,0.5,-4.59242549680257E-17));
#52534=CARTESIAN_POINT('Origin',(0.,0.5,0.));
#52535=CARTESIAN_POINT('Origin',(0.,0.475,0.));
#52536=CARTESIAN_POINT('',(-0.425,0.45,-5.20474889637625E-17));
#52537=CARTESIAN_POINT('Origin',(0.,0.45,0.));
#52538=CARTESIAN_POINT('',(-0.4,0.475,-4.89858719658941E-17));
#52539=CARTESIAN_POINT('Origin',(0.,0.24,0.));
#52540=CARTESIAN_POINT('',(-0.425,0.0299999999999998,-5.20474889637625E-17));
#52541=CARTESIAN_POINT('Origin',(0.,0.0299999999999998,0.));
#52542=CARTESIAN_POINT('',(-0.425,0.24,-5.20474889637625E-17));
#52543=CARTESIAN_POINT('Origin',(0.,0.0150000000000001,0.));
#52544=CARTESIAN_POINT('',(-0.395,4.85722573273506E-17,-4.83735485663204E-17));
#52545=CARTESIAN_POINT('Origin',(0.,0.,0.));
#52546=CARTESIAN_POINT('',(-0.41,0.0150000000000001,-5.02105187650415E-17));
#52547=CARTESIAN_POINT('Origin',(0.27,0.,0.));
#52548=CARTESIAN_POINT('',(-0.27,0.,-3.30654635769785E-17));
#52549=CARTESIAN_POINT('Origin',(0.,0.,0.));
#52550=CARTESIAN_POINT('Origin',(0.,-0.02,0.));
#52551=CARTESIAN_POINT('',(-0.24505,-0.0498999999999999,3.00099698131059E-17));
#52552=CARTESIAN_POINT('Origin',(0.,-0.0498999999999999,0.));
#52553=CARTESIAN_POINT('',(-0.26,-0.02,-3.18408167778312E-17));
#52554=CARTESIAN_POINT('Origin',(0.,-0.995,0.));
#52555=CARTESIAN_POINT('',(-0.24505,-1.95495,3.00099698131059E-17));
#52556=CARTESIAN_POINT('Origin',(0.,-1.95495,0.));
#52557=CARTESIAN_POINT('',(-0.24505,-0.995,-3.00099698131059E-17));
#52558=CARTESIAN_POINT('Origin',(0.,-1.975,0.));
#52559=CARTESIAN_POINT('',(-0.2,-2.,-2.44929359829471E-17));
#52560=CARTESIAN_POINT('Origin',(0.,-2.,0.));
#52561=CARTESIAN_POINT('',(-0.225,-1.975,-2.75545529808154E-17));
#52562=CARTESIAN_POINT('Origin',(0.,-2.,0.));
#52563=CARTESIAN_POINT('Origin',(0.115470053837925,-0.5,-0.2));
#52564=CARTESIAN_POINT('',(0.23094010767585,-0.5,0.));
#52565=CARTESIAN_POINT('',(0.115470053837925,-0.5,-0.2));
#52566=CARTESIAN_POINT('',(0.23094010767585,-0.5,0.));
#52567=CARTESIAN_POINT('',(0.115470053837925,-0.8,-0.2));
#52568=CARTESIAN_POINT('',(0.115470053837925,-0.5,-0.2));
#52569=CARTESIAN_POINT('',(0.23094010767585,-0.8,0.));
#52570=CARTESIAN_POINT('',(0.23094010767585,-0.8,0.));
#52571=CARTESIAN_POINT('',(0.23094010767585,-0.5,0.));
#52572=CARTESIAN_POINT('Origin',(-0.115470053837925,-0.5,-0.2));
#52573=CARTESIAN_POINT('',(-0.115470053837925,-0.5,-0.2));
#52574=CARTESIAN_POINT('',(0.115470053837925,-0.5,-0.2));
#52575=CARTESIAN_POINT('',(-0.115470053837925,-0.8,-0.2));
#52576=CARTESIAN_POINT('',(-0.115470053837925,-0.5,-0.2));
#52577=CARTESIAN_POINT('',(0.115470053837925,-0.8,-0.2));
#52578=CARTESIAN_POINT('Origin',(-0.23094010767585,-0.5,-2.77555756156289E-17));
#52579=CARTESIAN_POINT('',(-0.23094010767585,-0.5,-2.82820063659975E-17));
#52580=CARTESIAN_POINT('',(-0.115470053837925,-0.5,-0.2));
#52581=CARTESIAN_POINT('',(-0.23094010767585,-0.8,-2.77555756156289E-17));
#52582=CARTESIAN_POINT('',(-0.23094010767585,-0.5,-2.82820063659975E-17));
#52583=CARTESIAN_POINT('',(-0.115470053837925,-0.8,-0.2));
#52584=CARTESIAN_POINT('Origin',(-0.115470053837925,-0.5,0.2));
#52585=CARTESIAN_POINT('',(-0.115470053837925,-0.5,0.2));
#52586=CARTESIAN_POINT('',(-0.23094010767585,-0.5,-2.82820063659975E-17));
#52587=CARTESIAN_POINT('',(-0.115470053837925,-0.8,0.2));
#52588=CARTESIAN_POINT('',(-0.115470053837925,-0.5,0.2));
#52589=CARTESIAN_POINT('',(-0.23094010767585,-0.8,-2.82820063659975E-17));
#52590=CARTESIAN_POINT('Origin',(0.115470053837925,-0.5,0.2));
#52591=CARTESIAN_POINT('',(0.115470053837925,-0.5,0.2));
#52592=CARTESIAN_POINT('',(-0.115470053837925,-0.5,0.2));
#52593=CARTESIAN_POINT('',(0.115470053837925,-0.8,0.2));
#52594=CARTESIAN_POINT('',(0.115470053837925,-0.5,0.2));
#52595=CARTESIAN_POINT('',(-0.115470053837925,-0.8,0.2));
#52596=CARTESIAN_POINT('Origin',(0.23094010767585,-0.5,0.));
#52597=CARTESIAN_POINT('',(0.115470053837925,-0.5,0.2));
#52598=CARTESIAN_POINT('',(0.115470053837925,-0.8,0.2));
#52599=CARTESIAN_POINT('Origin',(0.,-0.5,0.));
#52600=CARTESIAN_POINT('Origin',(0.,-0.8,0.));
#52601=CARTESIAN_POINT('',(0.,0.,0.));
#52602=CARTESIAN_POINT('',(0.,0.,0.));
#52603=CARTESIAN_POINT('',(0.,0.,0.));
#52604=CARTESIAN_POINT('',(13.5,-6.,2.8));
#52605=CARTESIAN_POINT('',(12.,-7.9,7.2));
#52606=CARTESIAN_POINT('',(12.,-7.9,7.3));
#52607=CARTESIAN_POINT('',(12.,-4.1,7.2));
#52608=CARTESIAN_POINT('',(12.,-4.1,7.3));
#52609=CARTESIAN_POINT('',(15.,-7.9,7.2));
#52610=CARTESIAN_POINT('',(15.,-7.9,7.3));
#52611=CARTESIAN_POINT('',(15.,-4.1,7.2));
#52612=CARTESIAN_POINT('',(15.,-4.1,7.3));
#52613=CARTESIAN_POINT('',(0.,0.,0.));
#52614=CARTESIAN_POINT('',(15.1,-1.5,4.));
#52615=CARTESIAN_POINT('',(15.1,1.5,4.));
#52616=CARTESIAN_POINT('',(15.1,0.,5.5));
#52617=CARTESIAN_POINT('',(12.5,-1.5,7.2));
#52618=CARTESIAN_POINT('',(12.5,1.5,7.2));
#52619=CARTESIAN_POINT('',(14.,-1.5,7.2));
#52620=CARTESIAN_POINT('',(14.,1.5,7.2));
#52621=CARTESIAN_POINT('',(0.,0.,0.));
#52622=CARTESIAN_POINT('',(0.,0.,0.));
#52623=CARTESIAN_POINT('Origin',(4.,0.,4.));
#52624=CARTESIAN_POINT('',(4.12884541125756,8.40637486662632E-6,4.59405635738975));
#52625=CARTESIAN_POINT('',(4.02115458874249,-9.26662433349265E-6,4.59413599269206));
#52626=CARTESIAN_POINT('',(4.,-7.27562663373442E-17,4.5941));
#52627=CARTESIAN_POINT('',(4.,0.254721014554615,3.46322028700965));
#52628=CARTESIAN_POINT('Ctrl Pts',(4.12884541125756,8.40637486662632E-6,
4.59405635738975));
#52629=CARTESIAN_POINT('Ctrl Pts',(4.12564700130467,0.0398130654959074,
4.59407663624518));
#52630=CARTESIAN_POINT('Ctrl Pts',(4.12244859135178,0.079613792300143,4.59013569217808));
#52631=CARTESIAN_POINT('Ctrl Pts',(4.11925018139889,0.118599576779877,4.58219388355888));
#52632=CARTESIAN_POINT('Ctrl Pts',(4.11129754205509,0.215535206692688,4.56244709042845));
#52633=CARTESIAN_POINT('Ctrl Pts',(4.10334490271129,0.30743256945264,4.51796551073728));
#52634=CARTESIAN_POINT('Ctrl Pts',(4.09539226336748,0.383054411795556,4.45418672179759));
#52635=CARTESIAN_POINT('Ctrl Pts',(4.08743962402367,0.458676254138472,4.3904079328579));
#52636=CARTESIAN_POINT('Ctrl Pts',(4.07948698467986,0.518022576064352,4.30733193466969));
#52637=CARTESIAN_POINT('Ctrl Pts',(4.07153434533606,0.553840407547632,4.21511760274296));
#52638=CARTESIAN_POINT('Ctrl Pts',(4.06358170599225,0.589658239030912,4.12290327081622));
#52639=CARTESIAN_POINT('Ctrl Pts',(4.05562906664845,0.601947580071592,4.02155060515096));
#52640=CARTESIAN_POINT('Ctrl Pts',(4.04767642730464,0.589200356533535,3.92344812692479));
#52641=CARTESIAN_POINT('Ctrl Pts',(4.03972378796084,0.576453132995478,3.82534564869861));
#52642=CARTESIAN_POINT('Ctrl Pts',(4.03177114861703,0.538669344878685,3.73049335791153));
#52643=CARTESIAN_POINT('Ctrl Pts',(4.02381850927322,0.480479105222089,3.65049437695417));
#52644=CARTESIAN_POINT('Ctrl Pts',(4.01587900618215,0.422384984811151,3.57062753914914));
#52645=CARTESIAN_POINT('Ctrl Pts',(4.00793950309107,0.343951772361455,3.50556498199611));
#52646=CARTESIAN_POINT('Ctrl Pts',(4.,0.254721014554615,3.46322028700965));
#52647=CARTESIAN_POINT('',(4.,0.254694598474614,4.53673594206822));
#52648=CARTESIAN_POINT('Origin',(4.,0.,4.));
#52649=CARTESIAN_POINT('Ctrl Pts',(3.99999999999998,0.254694598474614,4.53673594206822));
#52650=CARTESIAN_POINT('Ctrl Pts',(4.00705152958082,0.175425736340139,4.5743509952638));
#52651=CARTESIAN_POINT('Ctrl Pts',(4.01410305916165,0.0876996967667308,
4.59405101338575));
#52652=CARTESIAN_POINT('Ctrl Pts',(4.02115458874249,-9.26662433349265E-6,
4.59413599269206));
#52653=CARTESIAN_POINT('Origin',(4.,0.,4.));
#52654=CARTESIAN_POINT('',(4.42884541125756,-2.46302091461148E-6,4.59415045696459));
#52655=CARTESIAN_POINT('',(4.32115458874249,3.58587963140688E-6,4.59404994535016));
#52656=CARTESIAN_POINT('',(4.,-7.27562663373442E-17,4.5941));
#52657=CARTESIAN_POINT('Ctrl Pts',(4.42884541125756,-2.46302091461148E-6,
4.59415045696459));
#52658=CARTESIAN_POINT('Ctrl Pts',(4.42107867343035,0.0966117732708647,
4.59412799973471));
#52659=CARTESIAN_POINT('Ctrl Pts',(4.41331193560314,0.193236775309615,4.57009608476161));
#52660=CARTESIAN_POINT('Ctrl Pts',(4.40554519777592,0.278573173318151,4.52479781884576));
#52661=CARTESIAN_POINT('Ctrl Pts',(4.39759255843212,0.36595214906825,4.47841531183407));
#52662=CARTESIAN_POINT('Ctrl Pts',(4.38963991908831,0.441495654419193,4.40973622444741));
#52663=CARTESIAN_POINT('Ctrl Pts',(4.3816872797445,0.495967466205845,4.32715751007026));
#52664=CARTESIAN_POINT('Ctrl Pts',(4.3737346404007,0.550439277992498,4.24457879569311));
#52665=CARTESIAN_POINT('Ctrl Pts',(4.36578200105689,0.58383939621486,4.14810045432546));
#52666=CARTESIAN_POINT('Ctrl Pts',(4.35782936171309,0.59208420294366,4.04951827803692));
#52667=CARTESIAN_POINT('Ctrl Pts',(4.34987672236928,0.600329009672459,3.95093610174838));
#52668=CARTESIAN_POINT('Ctrl Pts',(4.34192408302547,0.583418504907695,3.85025009053894));
#52669=CARTESIAN_POINT('Ctrl Pts',(4.33397144368167,0.54342022548472,3.75977047903001));
#52670=CARTESIAN_POINT('Ctrl Pts',(4.32601880433786,0.503421946061746,3.66929086752108));
#52671=CARTESIAN_POINT('Ctrl Pts',(4.31806616499406,0.440335891980562,3.58901765571266));
#52672=CARTESIAN_POINT('Ctrl Pts',(4.31011352565025,0.361875197644003,3.52876534000234));
#52673=CARTESIAN_POINT('Ctrl Pts',(4.30216088630644,0.283414503307443,3.46851302429202));
#52674=CARTESIAN_POINT('Ctrl Pts',(4.29420824696263,0.189579168715509,3.4282816046798));
#52675=CARTESIAN_POINT('Ctrl Pts',(4.28625560761883,0.0918418319479975,
3.41298991457491));
#52676=CARTESIAN_POINT('Ctrl Pts',(4.27830296827502,-0.00589550481951406,
3.39769822447003));
#52677=CARTESIAN_POINT('Ctrl Pts',(4.27035032893122,-0.107534843762603,
3.4073462638725));
#52678=CARTESIAN_POINT('Ctrl Pts',(4.26239768958741,-0.200649373295791,
3.44075443909651));
#52679=CARTESIAN_POINT('Ctrl Pts',(4.25444505024361,-0.293763902828979,
3.47416261432052));
#52680=CARTESIAN_POINT('Ctrl Pts',(4.24649241089979,-0.378353622952266,
3.53133092536608));
#52681=CARTESIAN_POINT('Ctrl Pts',(4.23853977155599,-0.444076322467606,
3.60526974769923));
#52682=CARTESIAN_POINT('Ctrl Pts',(4.23058713221218,-0.509799021982947,
3.67920857003239));
#52683=CARTESIAN_POINT('Ctrl Pts',(4.22263449286838,-0.556654700890342,
3.76991790365313));
#52684=CARTESIAN_POINT('Ctrl Pts',(4.21468185352458,-0.578914549750806,
3.86630733464992));
#52685=CARTESIAN_POINT('Ctrl Pts',(4.20672921418077,-0.601174398611269,
3.96269676564671));
#52686=CARTESIAN_POINT('Ctrl Pts',(4.19877657483696,-0.598838417424802,
4.06476629401955));
#52687=CARTESIAN_POINT('Ctrl Pts',(4.19082393549315,-0.5721923335546,4.16003645884502));
#52688=CARTESIAN_POINT('Ctrl Pts',(4.18287129614934,-0.545546249684398,
4.25530662367048));
#52689=CARTESIAN_POINT('Ctrl Pts',(4.17491865680554,-0.494590063130461,
4.34377742494856));
#52690=CARTESIAN_POINT('Ctrl Pts',(4.16696601746173,-0.425553631634784,
4.41463223618795));
#52691=CARTESIAN_POINT('Ctrl Pts',(4.15901337811793,-0.356517200139107,
4.48548704742733));
#52692=CARTESIAN_POINT('Ctrl Pts',(4.15106073877413,-0.269400523701689,
4.53872586862801));
#52693=CARTESIAN_POINT('Ctrl Pts',(4.14310809943032,-0.174855236950146,
4.56783927594351));
#52694=CARTESIAN_POINT('Ctrl Pts',(4.1383538700394,-0.118334381217266,4.5852437891806));
#52695=CARTESIAN_POINT('Ctrl Pts',(4.13359964064848,-0.0591586432141876,
4.59402621418361));
#52696=CARTESIAN_POINT('Ctrl Pts',(4.12884541125756,8.40637486662632E-6,
4.59405635738975));
#52697=CARTESIAN_POINT('Ctrl Pts',(4.02115458874249,-9.26662433349265E-6,
4.59413599269206));
#52698=CARTESIAN_POINT('Ctrl Pts',(4.02205569850546,-0.0112175303500608,
4.59414685213492));
#52699=CARTESIAN_POINT('Ctrl Pts',(4.02295680826843,-0.0224255152200988,
4.5938373961197));
#52700=CARTESIAN_POINT('Ctrl Pts',(4.0238579180314,-0.0336155370699344,
4.59320407706013));
#52701=CARTESIAN_POINT('Ctrl Pts',(4.03181055737521,-0.132371772633995,
4.58761479340425));
#52702=CARTESIAN_POINT('Ctrl Pts',(4.03976319671902,-0.229728915328813,
4.55680066053817));
#52703=CARTESIAN_POINT('Ctrl Pts',(4.04771583606282,-0.31374319278985,4.50455967689729));
#52704=CARTESIAN_POINT('Ctrl Pts',(4.05566847540663,-0.397757470250888,
4.4523186932564));
#52705=CARTESIAN_POINT('Ctrl Pts',(4.06362111475043,-0.468428882478145,
4.37865085884071));
#52706=CARTESIAN_POINT('Ctrl Pts',(4.07157375409424,-0.517135915630147,
4.29254879227412));
#52707=CARTESIAN_POINT('Ctrl Pts',(4.07952639343804,-0.565842948782149,
4.20644672570752));
#52708=CARTESIAN_POINT('Ctrl Pts',(4.08747903278185,-0.592585602858896,
4.10791042699003));
#52709=CARTESIAN_POINT('Ctrl Pts',(4.09543167212566,-0.594084460855775,
4.00899459728238));
#52710=CARTESIAN_POINT('Ctrl Pts',(4.10338431146947,-0.595583318852653,
3.91007876757474));
#52711=CARTESIAN_POINT('Ctrl Pts',(4.11133695081327,-0.571838380769662,
3.81078340687695));
#52712=CARTESIAN_POINT('Ctrl Pts',(4.11928959015708,-0.525757920758293,
3.72324489380985));
#52713=CARTESIAN_POINT('Ctrl Pts',(4.12724222950088,-0.479677460746923,
3.63570638074275));
#52714=CARTESIAN_POINT('Ctrl Pts',(4.13519486884469,-0.411261478807175,
3.55992471530633));
#52715=CARTESIAN_POINT('Ctrl Pts',(4.1431475081885,-0.328872047298013,3.50516726345229));
#52716=CARTESIAN_POINT('Ctrl Pts',(4.1511001475323,-0.246482615788851,3.45040981159825));
#52717=CARTESIAN_POINT('Ctrl Pts',(4.15905278687611,-0.150119734710276,
3.41667657332659));
#52718=CARTESIAN_POINT('Ctrl Pts',(4.16700542621992,-0.0515665150750243,
3.40809082437526));
#52719=CARTESIAN_POINT('Ctrl Pts',(4.17495806556372,0.0469867045602276,
3.39950507542393));
#52720=CARTESIAN_POINT('Ctrl Pts',(4.18291070490753,0.147730262752155,3.41606681579293));
#52721=CARTESIAN_POINT('Ctrl Pts',(4.19086334425134,0.238347648045887,3.45575171487277));
#52722=CARTESIAN_POINT('Ctrl Pts',(4.19881598359514,0.32896503333962,3.49543661395261));
#52723=CARTESIAN_POINT('Ctrl Pts',(4.20676862293895,0.409456245735157,3.55824467174328));
#52724=CARTESIAN_POINT('Ctrl Pts',(4.21472126228276,0.469979735422806,3.63649644709345));
#52725=CARTESIAN_POINT('Ctrl Pts',(4.22267390162656,0.530503225110456,3.71474822244363));
#52726=CARTESIAN_POINT('Ctrl Pts',(4.23062654097037,0.571058992090217,3.80844371535332));
#52727=CARTESIAN_POINT('Ctrl Pts',(4.23857918031417,0.586688754827568,3.90612753493601));
#52728=CARTESIAN_POINT('Ctrl Pts',(4.24653181965798,0.602318517564919,4.0038113545187));
#52729=CARTESIAN_POINT('Ctrl Pts',(4.25448445900178,0.593022276059861,4.10548350077438));
#52730=CARTESIAN_POINT('Ctrl Pts',(4.26243709834559,0.559936509464549,4.19871308474845));
#52731=CARTESIAN_POINT('Ctrl Pts',(4.2703897376894,0.526850742869238,4.29194266872251));
#52732=CARTESIAN_POINT('Ctrl Pts',(4.27834237703321,0.469975451183674,4.37672969041494));
#52733=CARTESIAN_POINT('Ctrl Pts',(4.28629501637701,0.396264473279151,4.44270782630825));
#52734=CARTESIAN_POINT('Ctrl Pts',(4.29424765572082,0.322553495374627,4.50868596220156));
#52735=CARTESIAN_POINT('Ctrl Pts',(4.30220029506462,0.232006831251144,4.55585521229574));
#52736=CARTESIAN_POINT('Ctrl Pts',(4.31015293440843,0.135695012128791,4.57844846968215));
#52737=CARTESIAN_POINT('Ctrl Pts',(4.31382015251978,0.0912825306677821,
4.58886694826517));
#52738=CARTESIAN_POINT('Ctrl Pts',(4.31748737063114,0.0456441298716245,
4.59405951624442));
#52739=CARTESIAN_POINT('Ctrl Pts',(4.32115458874249,3.58587963140688E-6,
4.59404994535016));
#52740=CARTESIAN_POINT('Origin',(4.,0.,4.));
#52741=CARTESIAN_POINT('',(4.72884541125756,-4.67700812217808E-6,4.59405084457266));
#52742=CARTESIAN_POINT('',(4.62115458874249,3.7232086238465E-6,4.59414939806979));
#52743=CARTESIAN_POINT('',(4.,-7.27562663373442E-17,4.5941));
#52744=CARTESIAN_POINT('Ctrl Pts',(4.72884541125756,-4.67700812217808E-6,
4.59405084457266));
#52745=CARTESIAN_POINT('Ctrl Pts',(4.72446298489983,0.0545367878429411,
4.59403588702548));
#52746=CARTESIAN_POINT('Ctrl Pts',(4.7200805585421,0.10908225468116,4.58659074407712));
#52747=CARTESIAN_POINT('Ctrl Pts',(4.71569813218437,0.16154350694756,4.57176871113812));
#52748=CARTESIAN_POINT('Ctrl Pts',(4.70774549284056,0.256743148594298,4.54487167450041));
#52749=CARTESIAN_POINT('Ctrl Pts',(4.69979285349676,0.345079446524661,4.4936824501733));
#52750=CARTESIAN_POINT('Ctrl Pts',(4.69184021415295,0.415752085200636,4.42445961801412));
#52751=CARTESIAN_POINT('Ctrl Pts',(4.68388757480915,0.486424723876611,4.35523678585494));
#52752=CARTESIAN_POINT('Ctrl Pts',(4.67593493546534,0.539433703298198,4.26798034586369));
#52753=CARTESIAN_POINT('Ctrl Pts',(4.66798229612153,0.568297953762936,4.17335858623793));
#52754=CARTESIAN_POINT('Ctrl Pts',(4.66002965677773,0.597162204227674,4.07873682661218));
#52755=CARTESIAN_POINT('Ctrl Pts',(4.65207701743392,0.601881725735563,3.97674974735193));
#52756=CARTESIAN_POINT('Ctrl Pts',(4.64412437809011,0.581879492504365,3.87986665793328));
#52757=CARTESIAN_POINT('Ctrl Pts',(4.63617173874631,0.561877259273167,3.78298356851463));
#52758=CARTESIAN_POINT('Ctrl Pts',(4.6282190994025,0.517153271302883,3.69120446893757));
#52759=CARTESIAN_POINT('Ctrl Pts',(4.6202664600587,0.453175645250056,3.61575060413089));
#52760=CARTESIAN_POINT('Ctrl Pts',(4.61231382071489,0.389198019197228,3.5402967393242));
#52761=CARTESIAN_POINT('Ctrl Pts',(4.60436118137108,0.305966755061857,3.48116810928789));
#52762=CARTESIAN_POINT('Ctrl Pts',(4.59640854202727,0.213658008474022,3.4455939943611));
#52763=CARTESIAN_POINT('Ctrl Pts',(4.58845590268347,0.121349261886187,3.41001987943431));
#52764=CARTESIAN_POINT('Ctrl Pts',(4.58050326333966,0.0199630328458878,
3.39800027961704));
#52765=CARTESIAN_POINT('Ctrl Pts',(4.57255062399586,-0.0781048312986516,
3.41100475468789));
#52766=CARTESIAN_POINT('Ctrl Pts',(4.56459798465205,-0.17617269544319,3.42400922975875));
#52767=CARTESIAN_POINT('Ctrl Pts',(4.55664534530825,-0.270922194691968,
3.46203777971774));
#52768=CARTESIAN_POINT('Ctrl Pts',(4.54869270596444,-0.350768912290741,
3.52044089639904));
#52769=CARTESIAN_POINT('Ctrl Pts',(4.54074006662063,-0.430615629889515,
3.57884401308035));
#52770=CARTESIAN_POINT('Ctrl Pts',(4.53278742727683,-0.495559565838284,
3.65762169648397));
#52771=CARTESIAN_POINT('Ctrl Pts',(4.52483478793302,-0.537660439465301,
3.74714230187364));
#52772=CARTESIAN_POINT('Ctrl Pts',(4.51688214858921,-0.579761313092318,
3.8366629072633));
#52773=CARTESIAN_POINT('Ctrl Pts',(4.50892950924541,-0.599019124397585,
3.936926434639));
#52774=CARTESIAN_POINT('Ctrl Pts',(4.5009768699016,-0.593079343631488,4.03567430223551));
#52775=CARTESIAN_POINT('Ctrl Pts',(4.49302423055779,-0.587139562865391,
4.13442216983203));
#52776=CARTESIAN_POINT('Ctrl Pts',(4.48507159121399,-0.556002190027932,
4.23165437764937));
#52777=CARTESIAN_POINT('Ctrl Pts',(4.47711895187018,-0.503474193090318,
4.31548296397124));
#52778=CARTESIAN_POINT('Ctrl Pts',(4.46916631252638,-0.450946196152703,
4.39931155029312));
#52779=CARTESIAN_POINT('Ctrl Pts',(4.46121367318257,-0.377027575114933,
4.46973651511953));
#52780=CARTESIAN_POINT('Ctrl Pts',(4.45326103383876,-0.290755888038263,
4.51814744739689));
#52781=CARTESIAN_POINT('Ctrl Pts',(4.44530839449495,-0.204484200961595,
4.56655837967425));
#52782=CARTESIAN_POINT('Ctrl Pts',(4.43735575515115,-0.105859447846027,
4.59295527940255));
#52783=CARTESIAN_POINT('Ctrl Pts',(4.42940311580734,-0.00693984821361558,
4.59411076594835));
#52784=CARTESIAN_POINT('Ctrl Pts',(4.42921721429075,-0.0046274959494805,
4.59413777669183));
#52785=CARTESIAN_POINT('Ctrl Pts',(4.42903131277416,-0.00231498256911503,
4.59415099449182));
#52786=CARTESIAN_POINT('Ctrl Pts',(4.42884541125756,-2.46302091461148E-6,
4.59415045696459));
#52787=CARTESIAN_POINT('Ctrl Pts',(4.32115458874249,3.58587963140688E-6,
4.59404994535016));
#52788=CARTESIAN_POINT('Ctrl Pts',(4.32544000997495,-0.0533308355660028,
4.59403876103764));
#52789=CARTESIAN_POINT('Ctrl Pts',(4.3297254312074,-0.106668183692779,4.58692369872924));
#52790=CARTESIAN_POINT('Ctrl Pts',(4.33401085243985,-0.158055593105036,
4.57274269264177));
#52791=CARTESIAN_POINT('Ctrl Pts',(4.34196349178366,-0.253417405095285,
4.54642639353635));
#52792=CARTESIAN_POINT('Ctrl Pts',(4.34991613112746,-0.342064054954561,
4.49577653064689));
#52793=CARTESIAN_POINT('Ctrl Pts',(4.35786877047127,-0.413157291282808,
4.42698573291487));
#52794=CARTESIAN_POINT('Ctrl Pts',(4.36582140981507,-0.484250527611055,
4.35819493518285));
#52795=CARTESIAN_POINT('Ctrl Pts',(4.37377404915888,-0.537790350408272,
4.27126320260829));
#52796=CARTESIAN_POINT('Ctrl Pts',(4.38172668850269,-0.567230782432438,
4.17681912699824));
#52797=CARTESIAN_POINT('Ctrl Pts',(4.3896793278465,-0.596671214456604,4.0823750513882));
#52798=CARTESIAN_POINT('Ctrl Pts',(4.3976319671903,-0.602012255707717,3.98041863274268));
#52799=CARTESIAN_POINT('Ctrl Pts',(4.40558460653411,-0.582600893642323,
3.88341542999892));
#52800=CARTESIAN_POINT('Ctrl Pts',(4.41353724587791,-0.563189531576929,
3.78641222725516));
#52801=CARTESIAN_POINT('Ctrl Pts',(4.42148988522172,-0.519025766195027,
3.69436224041317));
#52802=CARTESIAN_POINT('Ctrl Pts',(4.42944252456553,-0.455509217992651,
3.61851983504546));
#52803=CARTESIAN_POINT('Ctrl Pts',(4.43739516390933,-0.391992669790276,
3.54267742967776));
#52804=CARTESIAN_POINT('Ctrl Pts',(4.44534780325314,-0.309123338767427,
3.48304260578434));
#52805=CARTESIAN_POINT('Ctrl Pts',(4.45330044259694,-0.217033129998519,
3.44690653227429));
#52806=CARTESIAN_POINT('Ctrl Pts',(4.46125308194075,-0.12494292122961,3.41077045876423));
#52807=CARTESIAN_POINT('Ctrl Pts',(4.46920572128456,-0.0236318347146405,
3.39813313563753));
#52808=CARTESIAN_POINT('Ctrl Pts',(4.47715836062837,0.074513469760962,3.41053964803971));
#52809=CARTESIAN_POINT('Ctrl Pts',(4.48511099997217,0.172658774236564,3.42294616044189));
#52810=CARTESIAN_POINT('Ctrl Pts',(4.49306363931598,0.2676382966728,3.46039650837296));
#52811=CARTESIAN_POINT('Ctrl Pts',(4.50101627865978,0.34783949666059,3.51831187658845));
#52812=CARTESIAN_POINT('Ctrl Pts',(4.50896891800359,0.428040696648381,3.57622724480394));
#52813=CARTESIAN_POINT('Ctrl Pts',(4.51692155734739,0.493463574187728,3.65460763330386));
#52814=CARTESIAN_POINT('Ctrl Pts',(4.5248741966912,0.536109291561612,3.74386997215216));
#52815=CARTESIAN_POINT('Ctrl Pts',(4.53282683603501,0.578755008935497,3.83313231100046));
#52816=CARTESIAN_POINT('Ctrl Pts',(4.54077947537881,0.598623566143919,3.93327660019715));
#52817=CARTESIAN_POINT('Ctrl Pts',(4.54873211472262,0.593285761408823,4.03205883640902));
#52818=CARTESIAN_POINT('Ctrl Pts',(4.55668475406643,0.587947956673727,4.1308410726209));
#52819=CARTESIAN_POINT('Ctrl Pts',(4.56463739341024,0.557403789995114,4.22826125584796));
#52820=CARTESIAN_POINT('Ctrl Pts',(4.57259003275404,0.505387701781775,4.31240844187621));
#52821=CARTESIAN_POINT('Ctrl Pts',(4.58054267209785,0.453371613568435,4.39655562790445));
#52822=CARTESIAN_POINT('Ctrl Pts',(4.58849531144165,0.37988360382037,4.46742981673387));
#52823=CARTESIAN_POINT('Ctrl Pts',(4.59644795078546,0.293908582600447,4.51636567348148));
#52824=CARTESIAN_POINT('Ctrl Pts',(4.60440059012926,0.207933561380525,4.56530153022909));
#52825=CARTESIAN_POINT('Ctrl Pts',(4.61235322947307,0.109471528688745,4.59229905489488));
#52826=CARTESIAN_POINT('Ctrl Pts',(4.62030586881688,0.01056080905581,4.59405743239568));
#52827=CARTESIAN_POINT('Ctrl Pts',(4.62058877545875,0.00704216595801619,
4.59411998479525));
#52828=CARTESIAN_POINT('Ctrl Pts',(4.62087168210062,0.00352295504485493,
4.59415059693914));
#52829=CARTESIAN_POINT('Ctrl Pts',(4.62115458874249,3.7232086238465E-6,
4.59414939806979));
#52830=CARTESIAN_POINT('Origin',(4.,0.,4.));
#52831=CARTESIAN_POINT('',(5.02884541125756,1.1583539301252E-5,4.59413174414479));
#52832=CARTESIAN_POINT('',(4.92115458874249,-9.52916733652962E-6,4.59405847898621));
#52833=CARTESIAN_POINT('',(4.,-7.27562663373442E-17,4.5941));
#52834=CARTESIAN_POINT('Ctrl Pts',(5.02884541125756,1.1583539301252E-5,
4.59413174414479));
#52835=CARTESIAN_POINT('Ctrl Pts',(5.02784729636931,0.0124287555737821,
4.59414271605904));
#52836=CARTESIAN_POINT('Ctrl Pts',(5.02684918148107,0.024845254523583,4.59376142828251));
#52837=CARTESIAN_POINT('Ctrl Pts',(5.02585106659282,0.0372368329321061,
4.59298328977014));
#52838=CARTESIAN_POINT('Ctrl Pts',(5.01789842724901,0.135968707532707,4.58678334723719));
#52839=CARTESIAN_POINT('Ctrl Pts',(5.00994578790521,0.233118536601742,4.55538989360237));
#52840=CARTESIAN_POINT('Ctrl Pts',(5.0019931485614,0.316808430381418,4.50264120614281));
#52841=CARTESIAN_POINT('Ctrl Pts',(4.9940405092176,0.400498324161095,4.44989251868324));
#52842=CARTESIAN_POINT('Ctrl Pts',(4.98608786987379,0.470728282651411,4.37578859739892));
#52843=CARTESIAN_POINT('Ctrl Pts',(4.97813523052998,0.518911736914097,4.289389655942));
#52844=CARTESIAN_POINT('Ctrl Pts',(4.97018259118617,0.567095191176782,4.20299071448508));
#52845=CARTESIAN_POINT('Ctrl Pts',(4.96222995184237,0.593232141211837,4.10429675285556));
#52846=CARTESIAN_POINT('Ctrl Pts',(4.95427731249856,0.594126988899363,4.00537445204741));
#52847=CARTESIAN_POINT('Ctrl Pts',(4.94632467315476,0.595021836586889,3.90645215123927));
#52848=CARTESIAN_POINT('Ctrl Pts',(4.93837203381095,0.570674581926886,3.80730151125251));
#52849=CARTESIAN_POINT('Ctrl Pts',(4.93041939446714,0.524062008404491,3.72004504823011));
#52850=CARTESIAN_POINT('Ctrl Pts',(4.92246675512334,0.477449434882097,3.6327885852077));
#52851=CARTESIAN_POINT('Ctrl Pts',(4.91451411577953,0.408571542497308,3.55742629914966));
#52852=CARTESIAN_POINT('Ctrl Pts',(4.90656147643572,0.325849591692228,3.50317225594031));
#52853=CARTESIAN_POINT('Ctrl Pts',(4.89860883709192,0.243127640887147,3.44891821273095));
#52854=CARTESIAN_POINT('Ctrl Pts',(4.89065619774811,0.146561631661773,3.41577241237029));
#52855=CARTESIAN_POINT('Ctrl Pts',(4.88270355840431,0.0479580738465473,
3.40778738038914));
#52856=CARTESIAN_POINT('Ctrl Pts',(4.8747509190605,-0.0506454839686783,
3.39980234840799));
#52857=CARTESIAN_POINT('Ctrl Pts',(4.86679827971669,-0.151286590373755,
3.41697808480634));
#52858=CARTESIAN_POINT('Ctrl Pts',(4.85884564037289,-0.241660499406316,
3.45721462188069));
#52859=CARTESIAN_POINT('Ctrl Pts',(4.85089300102908,-0.332034408438876,
3.49745115895503));
#52860=CARTESIAN_POINT('Ctrl Pts',(4.84294036168527,-0.41214112009892,3.56074849670536));
#52861=CARTESIAN_POINT('Ctrl Pts',(4.83498772234147,-0.472186497854497,
3.63936767349926));
#52862=CARTESIAN_POINT('Ctrl Pts',(4.82703508299766,-0.532231875610076,
3.71798685029316));
#52863=CARTESIAN_POINT('Ctrl Pts',(4.81908244365386,-0.572215919461187,
3.81192786613063));
#52864=CARTESIAN_POINT('Ctrl Pts',(4.81112980431005,-0.587250035475296,
3.9097051523746));
#52865=CARTESIAN_POINT('Ctrl Pts',(4.80317716496624,-0.602284151489406,
4.00748243861856));
#52866=CARTESIAN_POINT('Ctrl Pts',(4.79522452562244,-0.592368339666514,
4.10909599526903));
#52867=CARTESIAN_POINT('Ctrl Pts',(4.78727188627863,-0.558714943052599,
4.20212218107662));
#52868=CARTESIAN_POINT('Ctrl Pts',(4.77931924693482,-0.525061546438685,
4.2951483668842));
#52869=CARTESIAN_POINT('Ctrl Pts',(4.77136660759101,-0.467670565033749,
4.37958718184891));
#52870=CARTESIAN_POINT('Ctrl Pts',(4.76341396824721,-0.393558827964045,
4.44511483080773));
#52871=CARTESIAN_POINT('Ctrl Pts',(4.7554613289034,-0.319447090894342,4.51064247976655));
#52872=CARTESIAN_POINT('Ctrl Pts',(4.7475086895596,-0.228614598159871,4.55725896271948));
#52873=CARTESIAN_POINT('Ctrl Pts',(4.73955605021579,-0.13216685911108,4.5792647797218));
#52874=CARTESIAN_POINT('Ctrl Pts',(4.73598583722972,-0.0888681559330128,
4.58914394690572));
#52875=CARTESIAN_POINT('Ctrl Pts',(4.73241562424364,-0.0444377444908,4.59406302997518));
#52876=CARTESIAN_POINT('Ctrl Pts',(4.72884541125756,-4.67700812217808E-6,
4.59405084457266));
#52877=CARTESIAN_POINT('Ctrl Pts',(4.62115458874249,3.7232086238465E-6,
4.59414939806979));
#52878=CARTESIAN_POINT('Ctrl Pts',(4.62882432144443,-0.0954043143036648,
4.59411689615543));
#52879=CARTESIAN_POINT('Ctrl Pts',(4.63649405414636,-0.190827729806029,
4.57070400848325));
#52880=CARTESIAN_POINT('Ctrl Pts',(4.6441637868483,-0.275369369969159,4.52648596729292));
#52881=CARTESIAN_POINT('Ctrl Pts',(4.65211642619211,-0.363029422787103,
4.48063689435358));
#52882=CARTESIAN_POINT('Ctrl Pts',(4.66006906553591,-0.438990121848901,
4.4124195181391));
#52883=CARTESIAN_POINT('Ctrl Pts',(4.66802170487971,-0.493964237128006,
4.33017434199545));
#52884=CARTESIAN_POINT('Ctrl Pts',(4.67597434422352,-0.548938352407109,
4.24792916585179));
#52885=CARTESIAN_POINT('Ctrl Pts',(4.68392698356733,-0.582925883903521,
4.15165618977896));
#52886=CARTESIAN_POINT('Ctrl Pts',(4.69187962291114,-0.591771392992132,
4.05312609631255));
#52887=CARTESIAN_POINT('Ctrl Pts',(4.69983226225494,-0.600616902080743,
3.95459600284613));
#52888=CARTESIAN_POINT('Ctrl Pts',(4.70778490159875,-0.584320388761555,
3.85380879198612));
#52889=CARTESIAN_POINT('Ctrl Pts',(4.71573754094256,-0.544874323741249,
3.76308707295491));
#52890=CARTESIAN_POINT('Ctrl Pts',(4.72369018028636,-0.505428258720944,
3.6723653539237));
#52891=CARTESIAN_POINT('Ctrl Pts',(4.73164281963017,-0.442832641999522,
3.59170912672127));
#52892=CARTESIAN_POINT('Ctrl Pts',(4.73959545897397,-0.364740640256699,
3.53097971363863));
#52893=CARTESIAN_POINT('Ctrl Pts',(4.74754809831778,-0.286648638513876,
3.47025030055599));
#52894=CARTESIAN_POINT('Ctrl Pts',(4.75550073766158,-0.193060251749651,
3.42944770159313));
#52895=CARTESIAN_POINT('Ctrl Pts',(4.76345337700539,-0.095417934894009,
3.41356059019365));
#52896=CARTESIAN_POINT('Ctrl Pts',(4.7714060163492,0.00222438196163176,
3.39767347879416));
#52897=CARTESIAN_POINT('Ctrl Pts',(4.77935865569301,0.10392062890869,3.40670185495805));
#52898=CARTESIAN_POINT('Ctrl Pts',(4.78731129503681,0.19723705468272,3.43954187673519));
#52899=CARTESIAN_POINT('Ctrl Pts',(4.79526393438062,0.290553480456751,3.47238189851233));
#52900=CARTESIAN_POINT('Ctrl Pts',(4.80321657372443,0.375490085057754,3.52903356590271));
#52901=CARTESIAN_POINT('Ctrl Pts',(4.81116921306823,0.441662211759978,3.60257044098769));
#52902=CARTESIAN_POINT('Ctrl Pts',(4.81912185241204,0.507834338462201,3.67610731607267));
#52903=CARTESIAN_POINT('Ctrl Pts',(4.82707449175584,0.555241987265645,3.76652939885225));
#52904=CARTESIAN_POINT('Ctrl Pts',(4.83502713109965,0.57808892742485,3.86278135818256));
#52905=CARTESIAN_POINT('Ctrl Pts',(4.84297977044346,0.600935867584054,3.95903331751286));
#52906=CARTESIAN_POINT('Ctrl Pts',(4.85093240978726,0.599222099099018,4.0611151533939));
#52907=CARTESIAN_POINT('Ctrl Pts',(4.85888504913107,0.573157153508111,4.15654597106253));
#52908=CARTESIAN_POINT('Ctrl Pts',(4.86683768847488,0.547092207917203,4.25197678873116));
#52909=CARTESIAN_POINT('Ctrl Pts',(4.87479032781868,0.496676085220424,4.34075658818739));
#52910=CARTESIAN_POINT('Ctrl Pts',(4.88274296716249,0.428072843071251,4.41203082979109));
#52911=CARTESIAN_POINT('Ctrl Pts',(4.89069560650629,0.359469600922078,4.48330507139479));
#52912=CARTESIAN_POINT('Ctrl Pts',(4.8986482458501,0.272679239320511,4.53707375514596));
#52913=CARTESIAN_POINT('Ctrl Pts',(4.90660088519391,0.178313062033339,4.56676292714126));
#52914=CARTESIAN_POINT('Ctrl Pts',(4.9114521197101,0.120748216373203,4.58487378690922));
#52915=CARTESIAN_POINT('Ctrl Pts',(4.9163033542263,0.0603642649825261,4.59402420038378));
#52916=CARTESIAN_POINT('Ctrl Pts',(4.92115458874249,-9.52916733652962E-6,
4.59405847898621));
#52917=CARTESIAN_POINT('Origin',(4.,0.,4.));
#52918=CARTESIAN_POINT('',(5.32884541125756,-1.45357002139801E-5,4.59407911932661));
#52919=CARTESIAN_POINT('',(5.22115458874249,1.46139895546772E-5,4.59411444380891));
#52920=CARTESIAN_POINT('',(4.,-7.27562663373442E-17,4.5941));
#52921=CARTESIAN_POINT('Ctrl Pts',(5.32884541125756,-1.45357002139801E-5,
4.59407911932661));
#52922=CARTESIAN_POINT('Ctrl Pts',(5.32327896849499,0.0692531541268509,
4.59401614001471));
#52923=CARTESIAN_POINT('Ctrl Pts',(5.31771252573242,0.138542285837495,4.5819075943171));
#52924=CARTESIAN_POINT('Ctrl Pts',(5.31214608296985,0.203593590158122,4.55818044906639));
#52925=CARTESIAN_POINT('Ctrl Pts',(5.30419344362604,0.296530782575621,4.5242820624512));
#52926=CARTESIAN_POINT('Ctrl Pts',(5.29624080428224,0.380818089806801,4.46666879957728));
#52927=CARTESIAN_POINT('Ctrl Pts',(5.28828816493843,0.446150240572578,4.39238466650784));
#52928=CARTESIAN_POINT('Ctrl Pts',(5.28033552559462,0.511482391338355,4.3181005334384));
#52929=CARTESIAN_POINT('Ctrl Pts',(5.27238288625081,0.557859385638729,4.22714553017344));
#52930=CARTESIAN_POINT('Ctrl Pts',(5.26443024690701,0.579611004278495,4.13064014464439));
#52931=CARTESIAN_POINT('Ctrl Pts',(5.2564776075632,0.601362622918262,4.03413475911534));
#52932=CARTESIAN_POINT('Ctrl Pts',(5.2485249682194,0.598488865897423,3.93207899132219));
#52933=CARTESIAN_POINT('Ctrl Pts',(5.24057232887559,0.571341089151559,3.8369505488493));
#52934=CARTESIAN_POINT('Ctrl Pts',(5.23261968953179,0.544193312405696,3.74182210637642));
#52935=CARTESIAN_POINT('Ctrl Pts',(5.22466705018798,0.492771515934809,3.65362098922379));
#52936=CARTESIAN_POINT('Ctrl Pts',(5.21671441084417,0.423362714708271,3.58313098523844));
#52937=CARTESIAN_POINT('Ctrl Pts',(5.20876177150037,0.353953913481732,3.51264098125308));
#52938=CARTESIAN_POINT('Ctrl Pts',(5.20080913215656,0.266558107499543,3.45986209043499));
#52939=CARTESIAN_POINT('Ctrl Pts',(5.19285649281275,0.171860624350003,3.43124725102074));
#52940=CARTESIAN_POINT('Ctrl Pts',(5.18490385346895,0.0771631412004631,
3.40263241160649));
#52941=CARTESIAN_POINT('Ctrl Pts',(5.17695121412514,-0.0248360191164267,
3.39818162359609));
#52942=CARTESIAN_POINT('Ctrl Pts',(5.16899857478133,-0.121666070051256,
3.41843905644231));
#52943=CARTESIAN_POINT('Ctrl Pts',(5.16104593543753,-0.218496120986084,
3.43869648928852));
#52944=CARTESIAN_POINT('Ctrl Pts',(5.15309329609372,-0.310157062538852,
3.48366214299137));
#52945=CARTESIAN_POINT('Ctrl Pts',(5.14514065674991,-0.385442096207774,
3.54783835396576));
#52946=CARTESIAN_POINT('Ctrl Pts',(5.13718801740611,-0.460727129876697,
3.61201456494015));
#52947=CARTESIAN_POINT('Ctrl Pts',(5.1292353780623,-0.519636255661773,3.6954013331861));
#52948=CARTESIAN_POINT('Ctrl Pts',(5.1212827387185,-0.554967030609594,3.78780349058054));
#52949=CARTESIAN_POINT('Ctrl Pts',(5.11333009937469,-0.590297805557415,
3.88020564797498));
#52950=CARTESIAN_POINT('Ctrl Pts',(5.10537746003088,-0.60205022966798,3.98162319451792));
#52951=CARTESIAN_POINT('Ctrl Pts',(5.09742482068708,-0.588787409028971,
4.07965645386523));
#52952=CARTESIAN_POINT('Ctrl Pts',(5.08947218134327,-0.575524588389962,
4.17768971321255));
#52953=CARTESIAN_POINT('Ctrl Pts',(5.08151954199946,-0.537246523001379,
4.27233868536424));
#52954=CARTESIAN_POINT('Ctrl Pts',(5.07356690265566,-0.47863322769376,4.35203124438164));
#52955=CARTESIAN_POINT('Ctrl Pts',(5.06561426331185,-0.42001993238614,4.43172380339905));
#52956=CARTESIAN_POINT('Ctrl Pts',(5.05766162396805,-0.341071407159484,
4.49645994928216));
#52957=CARTESIAN_POINT('Ctrl Pts',(5.04970898462424,-0.251440184480074,
4.53832480650817));
#52958=CARTESIAN_POINT('Ctrl Pts',(5.04275446016868,-0.1730583412759,4.5749353153996));
#52959=CARTESIAN_POINT('Ctrl Pts',(5.03579993571312,-0.0865070403179845,
4.59405529558476));
#52960=CARTESIAN_POINT('Ctrl Pts',(5.02884541125756,1.1583539301252E-5,
4.59413174414479));
#52961=CARTESIAN_POINT('Ctrl Pts',(4.92115458874249,-9.52916733652962E-6,
4.59405847898621));
#52962=CARTESIAN_POINT('Ctrl Pts',(4.9242559935701,-0.0386066277022544,
4.59408039337166));
#52963=CARTESIAN_POINT('Ctrl Pts',(4.92735739839772,-0.0771995748988638,
4.59037647703175));
#52964=CARTESIAN_POINT('Ctrl Pts',(4.93045880322533,-0.115049119822012,
4.58290605049323));
#52965=CARTESIAN_POINT('Ctrl Pts',(4.93841144256913,-0.212103131417409,
4.56375034161047));
#52966=CARTESIAN_POINT('Ctrl Pts',(4.94636408191294,-0.304269161635426,
4.51982926360553));
#52967=CARTESIAN_POINT('Ctrl Pts',(4.95431672125675,-0.380278658005779,
4.45651276645759));
#52968=CARTESIAN_POINT('Ctrl Pts',(4.96226936060055,-0.456288154376132,
4.39319626930964));
#52969=CARTESIAN_POINT('Ctrl Pts',(4.97022199994436,-0.516141116898821,
4.31048435301868));
#52970=CARTESIAN_POINT('Ctrl Pts',(4.97817463928816,-0.552519705724467,
4.21848967586497));
#52971=CARTESIAN_POINT('Ctrl Pts',(4.98612727863197,-0.588898294550112,
4.12649499871126));
#52972=CARTESIAN_POINT('Ctrl Pts',(4.99407991797578,-0.601802509678713,
4.0252175606948));
#52973=CARTESIAN_POINT('Ctrl Pts',(5.00203255731958,-0.589654635058918,
3.92703990798411));
#52974=CARTESIAN_POINT('Ctrl Pts',(5.00998519666339,-0.577506760439122,
3.82886225527341));
#52975=CARTESIAN_POINT('Ctrl Pts',(5.0179378360072,-0.540306796070929,3.73378438786847));
#52976=CARTESIAN_POINT('Ctrl Pts',(5.025890475351,-0.482602944251693,3.65343086999412));
#52977=CARTESIAN_POINT('Ctrl Pts',(5.03384311469481,-0.424899092432456,
3.57307735211977));
#52978=CARTESIAN_POINT('Ctrl Pts',(5.04179575403862,-0.346691353162178,
3.50744818377599));
#52979=CARTESIAN_POINT('Ctrl Pts',(5.04974839338242,-0.257541687734669,
3.46456742464414));
#52980=CARTESIAN_POINT('Ctrl Pts',(5.05770103272623,-0.16839202230716,3.42168666551229));
#52981=CARTESIAN_POINT('Ctrl Pts',(5.06565367207003,-0.0683004307224215,
3.40155431559236));
#52982=CARTESIAN_POINT('Ctrl Pts',(5.07360631141384,0.0304955267282049,
3.40663182885918));
#52983=CARTESIAN_POINT('Ctrl Pts',(5.08155895075765,0.129291484178831,3.41170934212599));
#52984=CARTESIAN_POINT('Ctrl Pts',(5.08951159010146,0.226791807495345,3.44199671857955));
#52985=CARTESIAN_POINT('Ctrl Pts',(5.09746422944526,0.311075754224562,3.49379091394262));
#52986=CARTESIAN_POINT('Ctrl Pts',(5.10541686878907,0.395359700953779,3.54558510930568));
#52987=CARTESIAN_POINT('Ctrl Pts',(5.11336950813287,0.466427271095698,3.61888612357825));
#52988=CARTESIAN_POINT('Ctrl Pts',(5.12132214747668,0.515589486279599,3.70473190942573));
#52989=CARTESIAN_POINT('Ctrl Pts',(5.12927478682048,0.564751701463499,3.79057769527322));
#52990=CARTESIAN_POINT('Ctrl Pts',(5.13722742616429,0.592008561689381,3.88896825269562));
#52991=CARTESIAN_POINT('Ctrl Pts',(5.1451800655081,0.594027544563649,3.98787399599556));
#52992=CARTESIAN_POINT('Ctrl Pts',(5.1531327048519,0.596046527437917,4.0867797392955));
#52993=CARTESIAN_POINT('Ctrl Pts',(5.16108534419571,0.572827632960568,4.18620066847299));
#52994=CARTESIAN_POINT('Ctrl Pts',(5.16903798353952,0.527209687216453,4.2739812208502));
#52995=CARTESIAN_POINT('Ctrl Pts',(5.17699062288332,0.481591741472338,4.3617617732274));
#52996=CARTESIAN_POINT('Ctrl Pts',(5.18494326222713,0.413574744461461,4.43790194880433));
#52997=CARTESIAN_POINT('Ctrl Pts',(5.19289590157094,0.331474700441294,4.49309257410834));
#52998=CARTESIAN_POINT('Ctrl Pts',(5.20084854091474,0.24937465642113,4.54828319941234));
#52999=CARTESIAN_POINT('Ctrl Pts',(5.20880118025855,0.153191565391677,4.58252427444343));
#53000=CARTESIAN_POINT('Ctrl Pts',(5.21675381960235,0.0546851202186884,
4.59162936142496));
#53001=CARTESIAN_POINT('Ctrl Pts',(5.21822074264906,0.0365148790664279,
4.59330886194775));
#53002=CARTESIAN_POINT('Ctrl Pts',(5.21968766569578,0.018265586889787,4.59413312238171));
#53003=CARTESIAN_POINT('Ctrl Pts',(5.22115458874249,1.46139895546772E-5,
4.59411444380891));
#53004=CARTESIAN_POINT('Origin',(4.,0.,4.));
#53005=CARTESIAN_POINT('',(5.62884541125756,1.52328526200479E-5,4.59408648697874));
#53006=CARTESIAN_POINT('',(5.52115458874249,-1.55733839743342E-5,4.59409663347568));
#53007=CARTESIAN_POINT('',(4.,-7.27562663373442E-17,4.5941));
#53008=CARTESIAN_POINT('Ctrl Pts',(5.62884541125756,1.52328526200479E-5,
4.59408648697874));
#53009=CARTESIAN_POINT('Ctrl Pts',(5.62666327996447,0.0271682673899915,
4.59411287463303));
#53010=CARTESIAN_POINT('Ctrl Pts',(5.62448114867138,0.054317778225707,4.59228554395034));
#53011=CARTESIAN_POINT('Ctrl Pts',(5.62229901737829,0.0812075234320336,
4.58857548522516));
#53012=CARTESIAN_POINT('Ctrl Pts',(5.61434637803449,0.179205497408217,4.57505441109036));
#53013=CARTESIAN_POINT('Ctrl Pts',(5.60639373869068,0.273753285393806,4.53652709601604));
#53014=CARTESIAN_POINT('Ctrl Pts',(5.59844109934688,0.353291132582354,4.47770402899113));
#53015=CARTESIAN_POINT('Ctrl Pts',(5.59048846000307,0.432828979770902,4.41888096196622));
#53016=CARTESIAN_POINT('Ctrl Pts',(5.58253582065927,0.497356886162411,4.33976214299073));
#53017=CARTESIAN_POINT('Ctrl Pts',(5.57458318131546,0.538985436353474,4.25002092526659));
#53018=CARTESIAN_POINT('Ctrl Pts',(5.56663054197165,0.580613986544537,4.16027970754245));
#53019=CARTESIAN_POINT('Ctrl Pts',(5.55867790262784,0.599343180535155,4.05991609106967));
#53020=CARTESIAN_POINT('Ctrl Pts',(5.55072526328404,0.592883119270616,3.96120089488413));
#53021=CARTESIAN_POINT('Ctrl Pts',(5.54277262394023,0.586423058006077,3.86248569869858));
#53022=CARTESIAN_POINT('Ctrl Pts',(5.53481998459642,0.554773741486382,3.76541892280029));
#53023=CARTESIAN_POINT('Ctrl Pts',(5.52686734525262,0.501804729712613,3.68186830256729));
#53024=CARTESIAN_POINT('Ctrl Pts',(5.51891470590881,0.448835717938844,3.5983176823343));
#53025=CARTESIAN_POINT('Ctrl Pts',(5.51096206656501,0.374547010911001,3.52828321776661));
#53026=CARTESIAN_POINT('Ctrl Pts',(5.5030094272212,0.288021414854312,3.48032757600706));
#53027=CARTESIAN_POINT('Ctrl Pts',(5.4950567878774,0.201495818797622,3.4323719342475));
#53028=CARTESIAN_POINT('Ctrl Pts',(5.48710414853359,0.102733333712086,3.40649511529609));
#53029=CARTESIAN_POINT('Ctrl Pts',(5.47915150918978,0.00380901851787326,
3.40586091270526));
#53030=CARTESIAN_POINT('Ctrl Pts',(5.47119886984597,-0.0951152966763399,
3.40522671011442));
#53031=CARTESIAN_POINT('Ctrl Pts',(5.46324623050217,-0.194201441979227,
3.42983512388417));
#53032=CARTESIAN_POINT('Ctrl Pts',(5.45529359115836,-0.281334786601535,
3.47667744027106));
#53033=CARTESIAN_POINT('Ctrl Pts',(5.44734095181456,-0.368468131223842,
3.52351975665794));
#53034=CARTESIAN_POINT('Ctrl Pts',(5.43938831247075,-0.443648675165568,
3.59259597566196));
#53035=CARTESIAN_POINT('Ctrl Pts',(5.43143567312694,-0.497684572991269,
3.67546058871077));
#53036=CARTESIAN_POINT('Ctrl Pts',(5.42348303378314,-0.551720470816969,
3.75832520175959));
#53037=CARTESIAN_POINT('Ctrl Pts',(5.41553039443933,-0.584611722526643,
3.85497820885321));
#53038=CARTESIAN_POINT('Ctrl Pts',(5.40757775509553,-0.592336924628993,
3.95360246348684));
#53039=CARTESIAN_POINT('Ctrl Pts',(5.39962511575172,-0.600062126731343,
4.05222671812048));
#53040=CARTESIAN_POINT('Ctrl Pts',(5.39167247640791,-0.582621279226368,
4.15282222029412));
#53041=CARTESIAN_POINT('Ctrl Pts',(5.3837198370641,-0.542146763261091,4.24308979978386));
#53042=CARTESIAN_POINT('Ctrl Pts',(5.3757671977203,-0.501672247295815,4.3333573792736));
#53043=CARTESIAN_POINT('Ctrl Pts',(5.36781455837649,-0.438164062870237,
4.41329703607943));
#53044=CARTESIAN_POINT('Ctrl Pts',(5.35986191903269,-0.359386950494509,
4.47313505840055));
#53045=CARTESIAN_POINT('Ctrl Pts',(5.35190927968888,-0.28060983811878,4.53297308072167));
#53046=CARTESIAN_POINT('Ctrl Pts',(5.34395664034507,-0.1865637977929,4.57270946855809));
#53047=CARTESIAN_POINT('Ctrl Pts',(5.33600400100126,-0.0887472388280498,
4.58748590729807));
#53048=CARTESIAN_POINT('Ctrl Pts',(5.33361780442003,-0.0593972924141157,
4.59191959101989));
#53049=CARTESIAN_POINT('Ctrl Pts',(5.3312316078388,-0.0297078841644672,
4.59410611700271));
#53050=CARTESIAN_POINT('Ctrl Pts',(5.32884541125756,-1.45357002139801E-5,
4.59407911932661));
#53051=CARTESIAN_POINT('Ctrl Pts',(5.22115458874249,1.46139895546772E-5,
4.59411444380891));
#53052=CARTESIAN_POINT('Ctrl Pts',(5.22764030503958,-0.0806785298274998,
4.59403186011492));
#53053=CARTESIAN_POINT('Ctrl Pts',(5.23412602133668,-0.161404528346198,
4.57747154641029));
#53054=CARTESIAN_POINT('Ctrl Pts',(5.24061173763377,-0.235476461490165,
4.54549665421293));
#53055=CARTESIAN_POINT('Ctrl Pts',(5.24856437697758,-0.32630179870949,4.50628976108741));
#53056=CARTESIAN_POINT('Ctrl Pts',(5.25651701632139,-0.407122673831612,
4.44390687590439));
#53057=CARTESIAN_POINT('Ctrl Pts',(5.26446965566519,-0.468057634114636,
4.36597515601533));
#53058=CARTESIAN_POINT('Ctrl Pts',(5.272422295009,-0.52899259439766,4.28804343612627));
#53059=CARTESIAN_POINT('Ctrl Pts',(5.28037493435281,-0.570041639841584,
4.19456288153117));
#53060=CARTESIAN_POINT('Ctrl Pts',(5.28832757369661,-0.586185965564114,
4.09696276320888));
#53061=CARTESIAN_POINT('Ctrl Pts',(5.29628021304042,-0.602330291286644,
3.99936264488659));
#53062=CARTESIAN_POINT('Ctrl Pts',(5.30423285238423,-0.59356989728778,3.89764296283709));
#53063=CARTESIAN_POINT('Ctrl Pts',(5.31218549172803,-0.560975861048054,
3.80424033358521));
#53064=CARTESIAN_POINT('Ctrl Pts',(5.32013813107184,-0.528381824808328,
3.71083770433334));
#53065=CARTESIAN_POINT('Ctrl Pts',(5.32809077041564,-0.471954146327742,
3.62575212787907));
#53066=CARTESIAN_POINT('Ctrl Pts',(5.33604340975945,-0.398591877830097,
3.55938647478623));
#53067=CARTESIAN_POINT('Ctrl Pts',(5.34399604910326,-0.325229609332449,
3.49302082169338));
#53068=CARTESIAN_POINT('Ctrl Pts',(5.35194868844707,-0.234932750817741,
3.44537509196196));
#53069=CARTESIAN_POINT('Ctrl Pts',(5.35990132779087,-0.138741323057917,
3.42227462497344));
#53070=CARTESIAN_POINT('Ctrl Pts',(5.36785396713468,-0.042549895298095,
3.39917415798493));
#53071=CARTESIAN_POINT('Ctrl Pts',(5.37580660647848,0.059536101706843,3.40061895373932));
#53072=CARTESIAN_POINT('Ctrl Pts',(5.38375924582229,0.155035264439678,3.42643236627792));
#53073=CARTESIAN_POINT('Ctrl Pts',(5.39171188516609,0.250534427172515,3.45224577881651));
#53074=CARTESIAN_POINT('Ctrl Pts',(5.3996645245099,0.339446755633248,3.5024278081393));
#53075=CARTESIAN_POINT('Ctrl Pts',(5.40761716385371,0.41090150670596,3.57084301769608));
#53076=CARTESIAN_POINT('Ctrl Pts',(5.41556980319751,0.482356257778672,3.63925822725286));
#53077=CARTESIAN_POINT('Ctrl Pts',(5.42352244254132,0.536353431463363,3.72590661704362));
#53078=CARTESIAN_POINT('Ctrl Pts',(5.43147508188513,0.566291137850326,3.82019424128906));
#53079=CARTESIAN_POINT('Ctrl Pts',(5.43942772122893,0.596228844237288,3.91448186553449));
#53080=CARTESIAN_POINT('Ctrl Pts',(5.44738036057274,0.602107083326521,4.01640872423458));
#53081=CARTESIAN_POINT('Ctrl Pts',(5.45533299991655,0.583207160329387,4.11351287069736));
#53082=CARTESIAN_POINT('Ctrl Pts',(5.46328563926035,0.564307237332252,4.21061701716013));
#53083=CARTESIAN_POINT('Ctrl Pts',(5.47123827860416,0.520629152248751,4.30289845138559));
#53084=CARTESIAN_POINT('Ctrl Pts',(5.47919091794796,0.457513145863858,4.37907451119169));
#53085=CARTESIAN_POINT('Ctrl Pts',(5.48714355729177,0.394397139478966,4.45525057099779));
#53086=CARTESIAN_POINT('Ctrl Pts',(5.49509619663558,0.311843211792683,4.51532125638452));
#53087=CARTESIAN_POINT('Ctrl Pts',(5.50304883597938,0.219944704826683,4.5519421079172));
#53088=CARTESIAN_POINT('Ctrl Pts',(5.50908408690042,0.150203009669811,4.5797336395568));
#53089=CARTESIAN_POINT('Ctrl Pts',(5.51511933782146,0.0750795109720808,
4.59401975858331));
#53090=CARTESIAN_POINT('Ctrl Pts',(5.52115458874249,-1.55733839743342E-5,
4.59409663347568));
#53091=CARTESIAN_POINT('Origin',(4.,0.,4.));
#53092=CARTESIAN_POINT('',(5.92884541125757,-1.3134308860685E-5,4.59412454375027));
#53093=CARTESIAN_POINT('',(5.82115458874249,1.31105368646138E-5,4.59407040741879));
#53094=CARTESIAN_POINT('',(4.,-7.27562663373442E-17,4.5941));
#53095=CARTESIAN_POINT('Ctrl Pts',(5.92884541125757,-1.3134308860685E-5,
4.59412454375027));
#53096=CARTESIAN_POINT('Ctrl Pts',(5.92209495209015,0.0839697382976411,
4.5940436242297));
#53097=CARTESIAN_POINT('Ctrl Pts',(5.91534449292274,0.16798613900316,4.57606223573506));
#53098=CARTESIAN_POINT('Ctrl Pts',(5.90859403375532,0.244517407380453,4.54150437939301));
#53099=CARTESIAN_POINT('Ctrl Pts',(5.90064139441152,0.334678026211646,4.50079216098422));
#53100=CARTESIAN_POINT('Ctrl Pts',(5.89268875506771,0.41445008323119,4.43707358099086));
#53101=CARTESIAN_POINT('Ctrl Pts',(5.8847361157239,0.474080337065587,4.35813908232779));
#53102=CARTESIAN_POINT('Ctrl Pts',(5.8767834763801,0.533710590899983,4.27920458366471));
#53103=CARTESIAN_POINT('Ctrl Pts',(5.86883083703629,0.573199041549232,4.18505416633191));
#53104=CARTESIAN_POINT('Ctrl Pts',(5.86087819769249,0.587717699183782,4.08719901244189));
#53105=CARTESIAN_POINT('Ctrl Pts',(5.85292555834868,0.602236356818331,3.98934385855186));
#53106=CARTESIAN_POINT('Ctrl Pts',(5.84497291900487,0.591785221438181,3.88778396810461));
#53107=CARTESIAN_POINT('Ctrl Pts',(5.83702027966107,0.557642080814915,3.79493641494568));
#53108=CARTESIAN_POINT('Ctrl Pts',(5.82906764031726,0.523498940191649,3.70208886178675));
#53109=CARTESIAN_POINT('Ctrl Pts',(5.82111500097346,0.465663794325265,3.61795364591614));
#53110=CARTESIAN_POINT('Ctrl Pts',(5.81316236162965,0.391207780605707,3.55281744653948));
#53111=CARTESIAN_POINT('Ctrl Pts',(5.80520972228584,0.31675176688615,3.48768124716281));
#53112=CARTESIAN_POINT('Ctrl Pts',(5.79725708294203,0.225674885313418,3.44154406428009));
#53113=CARTESIAN_POINT('Ctrl Pts',(5.78930444359823,0.129112523455512,3.42004679519738));
#53114=CARTESIAN_POINT('Ctrl Pts',(5.78135180425442,0.0325501615976049,
3.39854952611466));
#53115=CARTESIAN_POINT('Ctrl Pts',(5.77339916491062,-0.0694976805454773,
3.40169217083197));
#53116=CARTESIAN_POINT('Ctrl Pts',(5.76544652556681,-0.164554263536051,
3.42909049911887));
#53117=CARTESIAN_POINT('Ctrl Pts',(5.75749388622301,-0.259610846526622,
3.45648882740576));
#53118=CARTESIAN_POINT('Ctrl Pts',(5.7495412468792,-0.347676170364685,3.50814283926225));
#53119=CARTESIAN_POINT('Ctrl Pts',(5.74158860753539,-0.417983050247216,
3.57773712775495));
#53120=CARTESIAN_POINT('Ctrl Pts',(5.73363596819158,-0.488289930129746,
3.64733141624764));
#53121=CARTESIAN_POINT('Ctrl Pts',(5.72568332884778,-0.540838366056745,
3.73486598137654));
#53122=CARTESIAN_POINT('Ctrl Pts',(5.71773068950397,-0.569203595796233,
3.82963853060694));
#53123=CARTESIAN_POINT('Ctrl Pts',(5.70977805016017,-0.597568825535722,
3.92441107983734));
#53124=CARTESIAN_POINT('Ctrl Pts',(5.70182541081636,-0.6017508490877,4.02642161316923));
#53125=CARTESIAN_POINT('Ctrl Pts',(5.69387277147255,-0.581238357244447,
4.12319795341528));
#53126=CARTESIAN_POINT('Ctrl Pts',(5.68592013212875,-0.560725865401195,
4.21997429366132));
#53127=CARTESIAN_POINT('Ctrl Pts',(5.67796749278494,-0.515518858162713,
4.31151644082153));
#53128=CARTESIAN_POINT('Ctrl Pts',(5.67001485344113,-0.451144507802385,
4.38663212069642));
#53129=CARTESIAN_POINT('Ctrl Pts',(5.66206221409732,-0.386770157442057,
4.46174780057131));
#53130=CARTESIAN_POINT('Ctrl Pts',(5.65410957475352,-0.303228463959881,
4.52043701316089));
#53131=CARTESIAN_POINT('Ctrl Pts',(5.64615693540972,-0.210733537235404,
4.55552420285805));
#53132=CARTESIAN_POINT('Ctrl Pts',(5.640386427359,-0.143618370026196,4.5809837895275));
#53133=CARTESIAN_POINT('Ctrl Pts',(5.63461591930828,-0.07178924788396,4.59401670649762));
#53134=CARTESIAN_POINT('Ctrl Pts',(5.62884541125756,1.52328526200479E-5,
4.59408648697874));
#53135=CARTESIAN_POINT('Ctrl Pts',(5.52115458874249,-1.55733839743342E-5,
4.59409663347568));
#53136=CARTESIAN_POINT('Ctrl Pts',(5.52307197716526,-0.0238731473664388,
4.59412105649149));
#53137=CARTESIAN_POINT('Ctrl Pts',(5.52498936558803,-0.0477278534282068,
4.59271130989713));
#53138=CARTESIAN_POINT('Ctrl Pts',(5.5269067540108,-0.0714062077139717,
4.58984482465595));
#53139=CARTESIAN_POINT('Ctrl Pts',(5.53485939335461,-0.169615527042917,
4.57795567218339));
#53140=CARTESIAN_POINT('Ctrl Pts',(5.54281203269841,-0.264791079455087,
4.54100634955965));
#53141=CARTESIAN_POINT('Ctrl Pts',(5.55076467204222,-0.345296357402727,
4.48351441471562));
#53142=CARTESIAN_POINT('Ctrl Pts',(5.55871731138603,-0.425801635350366,
4.4260224798716));
#53143=CARTESIAN_POINT('Ctrl Pts',(5.56666995072984,-0.491636638833473,
4.34798793280729));
#53144=CARTESIAN_POINT('Ctrl Pts',(5.57462259007364,-0.534752142022197,
4.2589515597096));
#53145=CARTESIAN_POINT('Ctrl Pts',(5.58257522941745,-0.577867645210921,
4.16991518661191));
#53146=CARTESIAN_POINT('Ctrl Pts',(5.59052786876125,-0.598263648105263,
4.06987698748084));
#53147=CARTESIAN_POINT('Ctrl Pts',(5.59848050810506,-0.59344646156208,3.97106799465478));
#53148=CARTESIAN_POINT('Ctrl Pts',(5.60643314744886,-0.588629275018896,
3.87225900182873));
#53149=CARTESIAN_POINT('Ctrl Pts',(5.61438578679267,-0.558598899038186,
3.77467921530768));
#53150=CARTESIAN_POINT('Ctrl Pts',(5.62233842613648,-0.50702695609161,3.69025909300064));
#53151=CARTESIAN_POINT('Ctrl Pts',(5.63029106548029,-0.455455013145033,
3.6058389706936));
#53152=CARTESIAN_POINT('Ctrl Pts',(5.63824370482409,-0.382341503232591,
3.53457851260056));
#53153=CARTESIAN_POINT('Ctrl Pts',(5.6461963441679,-0.296625548722353,3.48519028027742));
#53154=CARTESIAN_POINT('Ctrl Pts',(5.6541489835117,-0.210909594212113,3.43580204795428));
#53155=CARTESIAN_POINT('Ctrl Pts',(5.66210162285551,-0.112591195104077,
3.40828604140104));
#53156=CARTESIAN_POINT('Ctrl Pts',(5.67005426219932,-0.0136911147678568,
3.40600646716786));
#53157=CARTESIAN_POINT('Ctrl Pts',(5.67800690154312,0.0852089655683624,
3.40372689293467));
#53158=CARTESIAN_POINT('Ctrl Pts',(5.68595954088693,0.184690727132768,3.42668375102154));
#53159=CARTESIAN_POINT('Ctrl Pts',(5.69391218023074,0.272591169676606,3.47207025288287));
#53160=CARTESIAN_POINT('Ctrl Pts',(5.70186481957454,0.360491612220445,3.51745675474419));
#53161=CARTESIAN_POINT('Ctrl Pts',(5.70981745891835,0.436810735743714,3.58527290037998));
#53162=CARTESIAN_POINT('Ctrl Pts',(5.71777009826216,0.492217487918224,3.667227242308));
#53163=CARTESIAN_POINT('Ctrl Pts',(5.72572273760596,0.547624240092733,3.74918158423602));
#53164=CARTESIAN_POINT('Ctrl Pts',(5.73367537694977,0.582118620918482,3.84527412245626));
#53165=CARTESIAN_POINT('Ctrl Pts',(5.74162801629357,0.591483222595687,3.94375623549444));
#53166=CARTESIAN_POINT('Ctrl Pts',(5.74958065563738,0.600847824272892,4.04223834853263));
#53167=CARTESIAN_POINT('Ctrl Pts',(5.75753329498119,0.585082646801554,4.14311003638875));
#53168=CARTESIAN_POINT('Ctrl Pts',(5.76548593432499,0.546115197731279,4.23403836123177));
#53169=CARTESIAN_POINT('Ctrl Pts',(5.7734385736688,0.507147748661005,4.32496668607478));
#53170=CARTESIAN_POINT('Ctrl Pts',(5.78139121301261,0.444978027991796,4.4059516479047));
#53171=CARTESIAN_POINT('Ctrl Pts',(5.78934385235641,0.367207131024688,4.46709173242012));
#53172=CARTESIAN_POINT('Ctrl Pts',(5.79729649170022,0.28943623405758,4.52823181693554));
#53173=CARTESIAN_POINT('Ctrl Pts',(5.80524913104403,0.196064160792572,4.56952702413646));
#53174=CARTESIAN_POINT('Ctrl Pts',(5.81320177038783,0.0985069184831505,
4.58592845199323));
#53175=CARTESIAN_POINT('Ctrl Pts',(5.81585270983939,0.0659871057213339,
4.59139571767544));
#53176=CARTESIAN_POINT('Ctrl Pts',(5.81850364929094,0.0330022532417819,
4.59409688335147));
#53177=CARTESIAN_POINT('Ctrl Pts',(5.82115458874249,1.31105368646138E-5,
4.59407040741879));
#53178=CARTESIAN_POINT('Origin',(4.,0.,4.));
#53179=CARTESIAN_POINT('',(6.22884541125756,-1.27841859475647E-5,4.5940334609955));
#53180=CARTESIAN_POINT('',(6.12115458874249,-9.50793186244619E-6,4.59413936148612));
#53181=CARTESIAN_POINT('',(4.,-7.27562663373442E-17,4.5941));
#53182=CARTESIAN_POINT('Ctrl Pts',(6.22884541125756,-1.27841859475647E-5,
4.5940334609955));
#53183=CARTESIAN_POINT('Ctrl Pts',(6.22547926355963,0.0418951881409122,
4.59406590912705));
#53184=CARTESIAN_POINT('Ctrl Pts',(6.2221131158617,0.0838018877146867,4.58971510200585));
#53185=CARTESIAN_POINT('Ctrl Pts',(6.21874696816377,0.124749109322564,4.58093223526196));
#53186=CARTESIAN_POINT('Ctrl Pts',(6.21079432881996,0.22148832423537,4.56018241146135));
#53187=CARTESIAN_POINT('Ctrl Pts',(6.20284168947616,0.31287214740051,4.51469474440412));
#53188=CARTESIAN_POINT('Ctrl Pts',(6.19488905013236,0.387808805213989,4.4501133836823));
#53189=CARTESIAN_POINT('Ctrl Pts',(6.18693641078855,0.462745463027469,4.38553202296047));
#53190=CARTESIAN_POINT('Ctrl Pts',(6.17898377144474,0.521234955489287,4.30185696857405));
#53191=CARTESIAN_POINT('Ctrl Pts',(6.17103113210093,0.556083161424236,4.20927485003939));
#53192=CARTESIAN_POINT('Ctrl Pts',(6.16307849275713,0.590931367359184,4.11669273150472));
#53193=CARTESIAN_POINT('Ctrl Pts',(6.15512585341332,0.602138286767263,4.0152035488218));
#53194=CARTESIAN_POINT('Ctrl Pts',(6.14717321406952,0.588356486924291,3.9172389266648));
#53195=CARTESIAN_POINT('Ctrl Pts',(6.13922057472571,0.574574687081318,3.81927430450779));
#53196=CARTESIAN_POINT('Ctrl Pts',(6.1312679353819,0.535804167987293,3.7248342428767));
#53197=CARTESIAN_POINT('Ctrl Pts',(6.12331529603809,0.476773096629474,3.64545304401991));
#53198=CARTESIAN_POINT('Ctrl Pts',(6.11536265669429,0.417742025271657,3.56607184516312));
#53199=CARTESIAN_POINT('Ctrl Pts',(6.10741001735048,0.338450401650047,3.50174950908064));
#53200=CARTESIAN_POINT('Ctrl Pts',(6.09945737800668,0.248599092144812,3.46035682177302));
#53201=CARTESIAN_POINT('Ctrl Pts',(6.09150473866287,0.158747782639575,3.41896413446539));
#53202=CARTESIAN_POINT('Ctrl Pts',(6.08355209931906,0.0583367872507115,
3.40050109593262));
#53203=CARTESIAN_POINT('Ctrl Pts',(6.07559945997526,-0.0403606640336046,
3.40722161935946));
#53204=CARTESIAN_POINT('Ctrl Pts',(6.06764682063145,-0.139058115317921,
3.4139421427863));
#53205=CARTESIAN_POINT('Ctrl Pts',(6.05969418128764,-0.23604202249769,3.44584622817275));
#53206=CARTESIAN_POINT('Ctrl Pts',(6.05174154194384,-0.319452991027635,
3.49903499090221));
#53207=CARTESIAN_POINT('Ctrl Pts',(6.04378890260003,-0.40286395955758,3.55222375363166));
#53208=CARTESIAN_POINT('Ctrl Pts',(6.03583626325623,-0.472701989437702,
3.62669719370411));
#53209=CARTESIAN_POINT('Ctrl Pts',(6.02788362391242,-0.520429378860104,
3.71334895258148));
#53210=CARTESIAN_POINT('Ctrl Pts',(6.01993098456861,-0.568156768282506,
3.80000071145885));
#53211=CARTESIAN_POINT('Ctrl Pts',(6.0119783452248,-0.593773517247188,3.89883078914114));
#53212=CARTESIAN_POINT('Ctrl Pts',(6.004025705881,-0.594147126960238,3.99775637428654));
#53213=CARTESIAN_POINT('Ctrl Pts',(5.99607306653719,-0.594520736673288,
4.09668195943193));
#53214=CARTESIAN_POINT('Ctrl Pts',(5.98812042719339,-0.569651207134705,
4.19570305204043));
#53215=CARTESIAN_POINT('Ctrl Pts',(5.98016778784958,-0.52257944308796,4.28271270390554));
#53216=CARTESIAN_POINT('Ctrl Pts',(5.97221514850578,-0.475507679041215,
4.36972235577065));
#53217=CARTESIAN_POINT('Ctrl Pts',(5.96426250916196,-0.406233680486307,
4.44472056689237));
#53218=CARTESIAN_POINT('Ctrl Pts',(5.95630986981816,-0.323226996343023,
4.49853792802592));
#53219=CARTESIAN_POINT('Ctrl Pts',(5.94835723047435,-0.240220312199739,
4.55235528915947));
#53220=CARTESIAN_POINT('Ctrl Pts',(5.94040459113055,-0.143480942468078,
4.58499180030486));
#53221=CARTESIAN_POINT('Ctrl Pts',(5.93245195178675,-0.0448366672808267,
4.59245712746544));
#53222=CARTESIAN_POINT('Ctrl Pts',(5.93124977161035,-0.0299248641651563,
4.59358564190382));
#53223=CARTESIAN_POINT('Ctrl Pts',(5.93004759143396,-0.0149695309183627,
4.59413895459864));
#53224=CARTESIAN_POINT('Ctrl Pts',(5.92884541125757,-1.3134308860685E-5,
4.59412454375027));
#53225=CARTESIAN_POINT('Ctrl Pts',(5.82115458874249,1.31105368646138E-5,
4.59407040741879));
#53226=CARTESIAN_POINT('Ctrl Pts',(5.82645628863475,-0.0659629472043463,
4.59401745734129));
#53227=CARTESIAN_POINT('Ctrl Pts',(5.831757988527,-0.131956164688202,4.58305467757793));
#53228=CARTESIAN_POINT('Ctrl Pts',(5.83705968841925,-0.194280919321303,
4.56148970414564));
#53229=CARTESIAN_POINT('Ctrl Pts',(5.84501232776306,-0.287769103462499,
4.52914187992864));
#53230=CARTESIAN_POINT('Ctrl Pts',(5.85296496710686,-0.373003060391055,
4.47293858298203));
#53231=CARTESIAN_POINT('Ctrl Pts',(5.86091760645067,-0.439561779454174,
4.39975142997742));
#53232=CARTESIAN_POINT('Ctrl Pts',(5.86887024579447,-0.506120498517293,
4.32656427697281));
#53233=CARTESIAN_POINT('Ctrl Pts',(5.87682288513828,-0.554003979714975,
4.2363932679102));
#53234=CARTESIAN_POINT('Ctrl Pts',(5.88477552448209,-0.577357812582609,
4.14026304025204));
#53235=CARTESIAN_POINT('Ctrl Pts',(5.8927281638259,-0.600711645450243,4.04413281259387));
#53236=CARTESIAN_POINT('Ctrl Pts',(5.9006808031697,-0.59953582998783,3.94204336634015));
#53237=CARTESIAN_POINT('Ctrl Pts',(5.90863344251351,-0.573974130801472,
3.84647652011691));
#53238=CARTESIAN_POINT('Ctrl Pts',(5.91658608185731,-0.548412431615114,
3.75090967389367));
#53239=CARTESIAN_POINT('Ctrl Pts',(5.92453872120112,-0.498464848704808,
3.66186542770092));
#53240=CARTESIAN_POINT('Ctrl Pts',(5.93249136054493,-0.430238144626613,
3.59023066587279));
#53241=CARTESIAN_POINT('Ctrl Pts',(5.94044399988873,-0.362011440548417,
3.51859590404466));
#53242=CARTESIAN_POINT('Ctrl Pts',(5.94839663923254,-0.275505615302329,
3.46437062658116));
#53243=CARTESIAN_POINT('Ctrl Pts',(5.95634927857635,-0.181297202577209,
3.43418458862315));
#53244=CARTESIAN_POINT('Ctrl Pts',(5.96430191792015,-0.087088789852092,
3.40399855066514));
#53245=CARTESIAN_POINT('Ctrl Pts',(5.97225455726396,0.0148222103520573,
3.39785175221263));
#53246=CARTESIAN_POINT('Ctrl Pts',(5.98020719660777,0.111975824940657,3.41649576758492));
#53247=CARTESIAN_POINT('Ctrl Pts',(5.98815983595157,0.209129439529257,3.43513978295721));
#53248=CARTESIAN_POINT('Ctrl Pts',(5.99611247529537,0.301525668502307,3.47857461215431));
#53249=CARTESIAN_POINT('Ctrl Pts',(6.00406511463918,0.377867748972965,3.54148967172874));
#53250=CARTESIAN_POINT('Ctrl Pts',(6.01201775398299,0.454209829443624,3.60440473130317));
#53251=CARTESIAN_POINT('Ctrl Pts',(6.0199703933268,0.514497761411887,3.68680002125492));
#53252=CARTESIAN_POINT('Ctrl Pts',(6.02792303267061,0.551360647735685,3.77860175380959));
#53253=CARTESIAN_POINT('Ctrl Pts',(6.03587567201441,0.588223534059482,3.87040348636426));
#53254=CARTESIAN_POINT('Ctrl Pts',(6.04382831135821,0.601661374738811,3.97161166152184));
#53255=CARTESIAN_POINT('Ctrl Pts',(6.05178095070202,0.590030977261751,4.06985190192822));
#53256=CARTESIAN_POINT('Ctrl Pts',(6.05973359004583,0.578400579784692,4.16809214233459));
#53257=CARTESIAN_POINT('Ctrl Pts',(6.06768622938964,0.541701944151245,4.26336444798975));
#53258=CARTESIAN_POINT('Ctrl Pts',(6.07563886873345,0.484422419230229,4.3440210474869));
#53259=CARTESIAN_POINT('Ctrl Pts',(6.08359150807725,0.427142894309213,4.42467764698404));
#53260=CARTESIAN_POINT('Ctrl Pts',(6.09154414742105,0.349282480100627,4.49071854032316));
#53261=CARTESIAN_POINT('Ctrl Pts',(6.09949678676486,0.26035984028865,4.53406826097581));
#53262=CARTESIAN_POINT('Ctrl Pts',(6.10671605409073,0.179637418414302,4.5734203814938));
#53263=CARTESIAN_POINT('Ctrl Pts',(6.11393532141662,0.0897989573399868,
4.59407340590587));
#53264=CARTESIAN_POINT('Ctrl Pts',(6.12115458874249,-9.50793186244619E-6,
4.59413936148612));
#53265=CARTESIAN_POINT('Origin',(4.,0.,4.));
#53266=CARTESIAN_POINT('',(6.52884541125757,2.61457539729726E-5,4.59508370962656));
#53267=CARTESIAN_POINT('',(6.42115458874249,-0.000630941829811112,4.59394485456974));
#53268=CARTESIAN_POINT('',(4.,-7.27562663373442E-17,4.5941));
#53269=CARTESIAN_POINT('Ctrl Pts',(6.52884541125757,2.61457539729726E-5,
4.59508370962656));
#53270=CARTESIAN_POINT('Ctrl Pts',(6.5129582963415,0.196771080344787,4.59506033873941));
#53271=CARTESIAN_POINT('Ctrl Pts',(6.49707118142544,0.393450480974957,4.48779253427891));
#53272=CARTESIAN_POINT('Ctrl Pts',(6.48118406650938,0.500111739713094,4.32240987211318));
#53273=CARTESIAN_POINT('Ctrl Pts',(6.46527878782176,0.606894944490356,4.15683812760557));
#53274=CARTESIAN_POINT('Ctrl Pts',(6.44937350913416,0.623454053851315,3.93301856375293));
#53275=CARTESIAN_POINT('Ctrl Pts',(6.43346823044654,0.541809843535619,3.75368369989414));
#53276=CARTESIAN_POINT('Ctrl Pts',(6.41756295175893,0.460165633219924,3.57434883603535));
#53277=CARTESIAN_POINT('Ctrl Pts',(6.40165767307132,0.280318103227576,3.43949867217041));
#53278=CARTESIAN_POINT('Ctrl Pts',(6.3857523943837,0.085604811340831,3.41110814665827));
#53279=CARTESIAN_POINT('Ctrl Pts',(6.36984711569609,-0.109108480545914,
3.38271762114613));
#53280=CARTESIAN_POINT('Ctrl Pts',(6.35394183700848,-0.318687534327053,
3.46078673398678));
#53281=CARTESIAN_POINT('Ctrl Pts',(6.33803655832087,-0.448733343985475,
3.60951691634857));
#53282=CARTESIAN_POINT('Ctrl Pts',(6.33008391897706,-0.513756248814686,
3.68388200752946));
#53283=CARTESIAN_POINT('Ctrl Pts',(6.32213127963325,-0.558895842613217,
3.77591236609064));
#53284=CARTESIAN_POINT('Ctrl Pts',(6.31417864028945,-0.579995970841135,
3.87270290659392));
#53285=CARTESIAN_POINT('Ctrl Pts',(6.30622600094564,-0.601096099069052,
3.9694934470972));
#53286=CARTESIAN_POINT('Ctrl Pts',(6.29827336160184,-0.598156761726356,
4.07104416954258));
#53287=CARTESIAN_POINT('Ctrl Pts',(6.29032072225803,-0.570614590620327,
4.16591643177432));
#53288=CARTESIAN_POINT('Ctrl Pts',(6.28236808291422,-0.543072419514299,
4.26078869400605));
#53289=CARTESIAN_POINT('Ctrl Pts',(6.27441544357042,-0.490927414644939,
4.34898249602413));
#53290=CARTESIAN_POINT('Ctrl Pts',(6.26646280422661,-0.421087730399527,
4.41916768405122));
#53291=CARTESIAN_POINT('Ctrl Pts',(6.2585101648828,-0.351248046154114,4.48935287207832));
#53292=CARTESIAN_POINT('Ctrl Pts',(6.250557525539,-0.263713682532649,4.54152944611444));
#53293=CARTESIAN_POINT('Ctrl Pts',(6.24260488619519,-0.168899197391682,
4.5696117428605));
#53294=CARTESIAN_POINT('Ctrl Pts',(6.23801839454932,-0.114217245248871,
4.58580752565092));
#53295=CARTESIAN_POINT('Ctrl Pts',(6.23343190290344,-0.0571138332845632,
4.59398924930378));
#53296=CARTESIAN_POINT('Ctrl Pts',(6.22884541125756,-1.27841859475647E-5,
4.5940334609955));
#53297=CARTESIAN_POINT('Ctrl Pts',(6.12115458874249,-9.50793186244619E-6,
4.59413936148612));
#53298=CARTESIAN_POINT('Ctrl Pts',(6.12188796076042,-0.00913273504488762,
4.59414606160884));
#53299=CARTESIAN_POINT('Ctrl Pts',(6.12262133277835,-0.0182556526135436,
4.59394031163173));
#53300=CARTESIAN_POINT('Ctrl Pts',(6.12335470479628,-0.0273686726716501,
4.59352013235631));
#53301=CARTESIAN_POINT('Ctrl Pts',(6.13130734414009,-0.126189680404606,
4.58896373511797));
#53302=CARTESIAN_POINT('Ctrl Pts',(6.13925998348389,-0.223846830455152,
4.55919239267511));
#53303=CARTESIAN_POINT('Ctrl Pts',(6.14721262282769,-0.308403173896691,
4.50784224986958));
#53304=CARTESIAN_POINT('Ctrl Pts',(6.1551652621715,-0.392959517338232,4.45649210706404));
#53305=CARTESIAN_POINT('Ctrl Pts',(6.16311790151532,-0.464415054170765,
4.38356316389581));
#53306=CARTESIAN_POINT('Ctrl Pts',(6.17107054085912,-0.514027768136376,
4.29797916579711));
#53307=CARTESIAN_POINT('Ctrl Pts',(6.17902318020293,-0.563640482101988,
4.2123951676984));
#53308=CARTESIAN_POINT('Ctrl Pts',(6.18697581954673,-0.591410373200678,
4.11415611466921));
#53309=CARTESIAN_POINT('Ctrl Pts',(6.19492845889053,-0.593952774873424,
4.0152594949342));
#53310=CARTESIAN_POINT('Ctrl Pts',(6.20288109823434,-0.59649517654617,3.9163628751992));
#53311=CARTESIAN_POINT('Ctrl Pts',(6.21083373757815,-0.573810088792972,
3.81680868875837));
#53312=CARTESIAN_POINT('Ctrl Pts',(6.21878637692196,-0.528651094032059,
3.72879442104321));
#53313=CARTESIAN_POINT('Ctrl Pts',(6.22673901626577,-0.483492099271145,
3.64078015332805));
#53314=CARTESIAN_POINT('Ctrl Pts',(6.23469165560957,-0.415859197502516,
3.56430580433857));
#53315=CARTESIAN_POINT('Ctrl Pts',(6.24264429495337,-0.334059153459168,
3.50867301156809));
#53316=CARTESIAN_POINT('Ctrl Pts',(6.25059693429718,-0.252259109415819,
3.45304021879761));
#53317=CARTESIAN_POINT('Ctrl Pts',(6.25854957364099,-0.156291923097747,
3.41824898224614));
#53318=CARTESIAN_POINT('Ctrl Pts',(6.2665022129848,-0.057819682214149,3.40864436538418));
#53319=CARTESIAN_POINT('Ctrl Pts',(6.2744548523286,0.0406525586694487,3.39903974852221));
#53320=CARTESIAN_POINT('Ctrl Pts',(6.28240749167241,0.141629854118573,3.41462175134974));
#53321=CARTESIAN_POINT('Ctrl Pts',(6.29036013101621,0.232632044389671,3.453312878872));
#53322=CARTESIAN_POINT('Ctrl Pts',(6.29831277036002,0.323634234660771,3.49200400639426));
#53323=CARTESIAN_POINT('Ctrl Pts',(6.30626540970382,0.404661319753841,3.55380425861124));
#53324=CARTESIAN_POINT('Ctrl Pts',(6.31421804904763,0.466059055789261,3.63148218419904));
#53325=CARTESIAN_POINT('Ctrl Pts',(6.32217068839144,0.527456791824679,3.70916010978684));
#53326=CARTESIAN_POINT('Ctrl Pts',(6.33012332773525,0.569225178802449,3.80271570874544));
#53327=CARTESIAN_POINT('Ctrl Pts',(6.33807596707905,0.585790493249255,3.90010619949006));
#53328=CARTESIAN_POINT('Ctrl Pts',(6.34602860642286,0.602355807696062,3.99749669023468));
#53329=CARTESIAN_POINT('Ctrl Pts',(6.35398124576666,0.593718049611903,4.09872207276531));
#53330=CARTESIAN_POINT('Ctrl Pts',(6.36193388511047,0.56173881546021,4.19248215342453));
#53331=CARTESIAN_POINT('Ctrl Pts',(6.36988652445427,0.529759581308516,4.28624223408375));
#53332=CARTESIAN_POINT('Ctrl Pts',(6.37783916379808,0.474438871089287,4.37253701287156));
#53333=CARTESIAN_POINT('Ctrl Pts',(6.38579180314189,0.401374624788453,4.4390182948332));
#53334=CARTESIAN_POINT('Ctrl Pts',(6.39757939834209,0.293077024234899,4.53755846574697));
#53335=CARTESIAN_POINT('Ctrl Pts',(6.40936699354229,0.145797072855576,4.59256860517148));
#53336=CARTESIAN_POINT('Ctrl Pts',(6.42115458874249,-0.000630941829811112,
4.59394485456974));
#53337=CARTESIAN_POINT('Origin',(4.,0.,4.));
#53338=CARTESIAN_POINT('',(6.82884541125756,0.000528213615369061,4.5937871332276));
#53339=CARTESIAN_POINT('',(6.72115458874249,0.000109070110168276,4.59505938903171));
#53340=CARTESIAN_POINT('',(4.,-7.27562663373442E-17,4.5941));
#53341=CARTESIAN_POINT('Ctrl Pts',(6.82884541125756,0.000528213615369061,
4.5937871332276));
#53342=CARTESIAN_POINT('Ctrl Pts',(6.82429524715479,0.0572034606387535,
4.59426930340541));
#53343=CARTESIAN_POINT('Ctrl Pts',(6.81974508305202,0.113754426020979,4.58681959872387));
#53344=CARTESIAN_POINT('Ctrl Pts',(6.81519491894924,0.167823213394864,4.57092612439125));
#53345=CARTESIAN_POINT('Ctrl Pts',(6.79928964026163,0.356822799356826,4.51536985589957));
#53346=CARTESIAN_POINT('Ctrl Pts',(6.78338436157403,0.515493156338912,4.35664088088147));
#53347=CARTESIAN_POINT('Ctrl Pts',(6.76747908288642,0.570983871223461,4.16762126762428));
#53348=CARTESIAN_POINT('Ctrl Pts',(6.7515738041988,0.626474586108011,3.97860165436708));
#53349=CARTESIAN_POINT('Ctrl Pts',(6.73566852551118,0.578785658895023,3.75929140287077));
#53350=CARTESIAN_POINT('Ctrl Pts',(6.71976324682357,0.449805704301045,3.61038767491097));
#53351=CARTESIAN_POINT('Ctrl Pts',(6.70385796813595,0.320825749707067,3.46148394695116));
#53352=CARTESIAN_POINT('Ctrl Pts',(6.68795268944834,0.110554767732096,3.38298674252784));
#53353=CARTESIAN_POINT('Ctrl Pts',(6.67204741076073,-0.0844443642884844,
3.4109402193496));
#53354=CARTESIAN_POINT('Ctrl Pts',(6.65614213207312,-0.279443496309066,
3.43889369617135));
#53355=CARTESIAN_POINT('Ctrl Pts',(6.64023685338551,-0.459170778375258,
3.57329785423817));
#53356=CARTESIAN_POINT('Ctrl Pts',(6.6243315746979,-0.541132009270427,3.75243704050979));
#53357=CARTESIAN_POINT('Ctrl Pts',(6.60842629601029,-0.623093240165596,
3.9315762267814));
#53358=CARTESIAN_POINT('Ctrl Pts',(6.59252101732267,-0.60728841988974,4.15545044125781));
#53359=CARTESIAN_POINT('Ctrl Pts',(6.57661573863506,-0.500919754058047,
4.32127168369798));
#53360=CARTESIAN_POINT('Ctrl Pts',(6.56069229617589,-0.394429615589227,
4.48728229340579));
#53361=CARTESIAN_POINT('Ctrl Pts',(6.54476885371673,-0.197168666623305,
4.59510713395368));
#53362=CARTESIAN_POINT('Ctrl Pts',(6.52884541125757,2.61457539729726E-5,
4.59508370962656));
#53363=CARTESIAN_POINT('Ctrl Pts',(6.42115458874249,-0.000630941829811112,
4.59394485456974));
#53364=CARTESIAN_POINT('Ctrl Pts',(6.4252722722299,-0.0517816819022344,
4.59442561076518));
#53365=CARTESIAN_POINT('Ctrl Pts',(6.42938995571731,-0.102828462800867,
4.58836159088269));
#53366=CARTESIAN_POINT('Ctrl Pts',(6.43350763920472,-0.152073274319339,
4.5753220992581));
#53367=CARTESIAN_POINT('Ctrl Pts',(6.44941291789233,-0.342290043897387,
4.52495476314113));
#53368=CARTESIAN_POINT('Ctrl Pts',(6.46531819657995,-0.5056209461254,4.37051151428857));
#53369=CARTESIAN_POINT('Ctrl Pts',(6.48122347526756,-0.56632363157735,4.18304963962536));
#53370=CARTESIAN_POINT('Ctrl Pts',(6.49712875395518,-0.627026317029301,
3.99558776496215));
#53371=CARTESIAN_POINT('Ctrl Pts',(6.51303403264279,-0.58510078570519,3.77510726448829));
#53372=CARTESIAN_POINT('Ctrl Pts',(6.5289393113304,-0.460166914262479,3.62276494217392));
#53373=CARTESIAN_POINT('Ctrl Pts',(6.54484459001801,-0.335233042819767,
3.47042261985956));
#53374=CARTESIAN_POINT('Ctrl Pts',(6.56074986870563,-0.127290831258456,
3.38621847570468));
#53375=CARTESIAN_POINT('Ctrl Pts',(6.57665514739324,0.068373869747762,3.4088573345089));
#53376=CARTESIAN_POINT('Ctrl Pts',(6.59256042608085,0.26403857075398,3.43149619331313));
#53377=CARTESIAN_POINT('Ctrl Pts',(6.60846570476847,0.447425761205104,3.56097805507645));
#53378=CARTESIAN_POINT('Ctrl Pts',(6.62437098345608,0.534230294511761,3.73782813427527));
#53379=CARTESIAN_POINT('Ctrl Pts',(6.64027626214369,0.621034827818418,3.91467821347409));
#53380=CARTESIAN_POINT('Ctrl Pts',(6.65618154083131,0.611256703980608,4.1388965101084));
#53381=CARTESIAN_POINT('Ctrl Pts',(6.67208681951892,0.509439333868548,4.30754322537844));
#53382=CARTESIAN_POINT('Ctrl Pts',(6.68799209820653,0.40762196375649,4.47618994064847));
#53383=CARTESIAN_POINT('Ctrl Pts',(6.70389737689414,0.213765347370184,4.58926507455422));
#53384=CARTESIAN_POINT('Ctrl Pts',(6.71980265558175,0.016851802420978,4.59484308232941));
#53385=CARTESIAN_POINT('Ctrl Pts',(6.72025329996867,0.0112726493937942,
4.59500112406784));
#53386=CARTESIAN_POINT('Ctrl Pts',(6.72070394435558,0.00569104238866241,
4.59507287148453));
#53387=CARTESIAN_POINT('Ctrl Pts',(6.72115458874249,0.000109070110168276,
4.59505938903171));
#53388=CARTESIAN_POINT('Origin',(4.,0.,4.));
#53389=CARTESIAN_POINT('',(7.12884541125757,-0.000233413975479213,4.59320261234329));
#53390=CARTESIAN_POINT('',(7.02115458874249,0.000491936389841303,4.5936290357477));
#53391=CARTESIAN_POINT('',(4.,-7.27562663373442E-17,4.5941));
#53392=CARTESIAN_POINT('Ctrl Pts',(7.12884541125757,-0.000233413975479213,
4.59320261234329));
#53393=CARTESIAN_POINT('Ctrl Pts',(7.11972691928047,0.113624805666132,4.59280158872514));
#53394=CARTESIAN_POINT('Ctrl Pts',(7.11060842730338,0.227688545642871,4.56127879346404));
#53395=CARTESIAN_POINT('Ctrl Pts',(7.10148993532628,0.322592019514134,4.50005536307953));
#53396=CARTESIAN_POINT('Ctrl Pts',(7.08558465663867,0.488131036726243,4.39326405099382));
#53397=CARTESIAN_POINT('Ctrl Pts',(7.06967937795105,0.595374147168556,4.19610732087965));
#53398=CARTESIAN_POINT('Ctrl Pts',(7.05377409926343,0.595079946532544,3.99911121186167));
#53399=CARTESIAN_POINT('Ctrl Pts',(7.03786882057582,0.594785745896532,3.80211510284369));
#53400=CARTESIAN_POINT('Ctrl Pts',(7.02196354188821,0.486954234182196,3.60527961492189));
#53401=CARTESIAN_POINT('Ctrl Pts',(7.0060582632006,0.321096900356496,3.49898325846904));
#53402=CARTESIAN_POINT('Ctrl Pts',(6.99015298451299,0.155239566530797,3.3926869020162));
#53403=CARTESIAN_POINT('Ctrl Pts',(6.97424770582538,-0.0686435894062663,
3.37692967703231));
#53404=CARTESIAN_POINT('Ctrl Pts',(6.95834242713776,-0.247754555527299,
3.45894666907189));
#53405=CARTESIAN_POINT('Ctrl Pts',(6.94243714845015,-0.426865521648332,
3.54096366111146));
#53406=CARTESIAN_POINT('Ctrl Pts',(6.92653186976253,-0.561204297953336,
3.72075487017451));
#53407=CARTESIAN_POINT('Ctrl Pts',(6.91062659107492,-0.589088840804576,
3.91576771430201));
#53408=CARTESIAN_POINT('Ctrl Pts',(6.89472131238731,-0.616973383655816,
4.11078055842951));
#53409=CARTESIAN_POINT('Ctrl Pts',(6.8788160336997,-0.538403693053295,4.32101503762147));
#53410=CARTESIAN_POINT('Ctrl Pts',(6.86291075501209,-0.389454440281117,
4.44994049623482));
#53411=CARTESIAN_POINT('Ctrl Pts',(6.85155564042725,-0.283116420949728,
4.54198310574898));
#53412=CARTESIAN_POINT('Ctrl Pts',(6.8402005258424,-0.140907108175025,4.59258385846765));
#53413=CARTESIAN_POINT('Ctrl Pts',(6.82884541125756,0.000528213615369061,
4.5937871332276));
#53414=CARTESIAN_POINT('Ctrl Pts',(6.72115458874249,0.000109070110168276,
4.59505938903171));
#53415=CARTESIAN_POINT('Ctrl Pts',(6.73660922304319,-0.191322006690816,
4.59459701474307));
#53416=CARTESIAN_POINT('Ctrl Pts',(6.75206385734389,-0.38318268672033,4.49389457135631));
#53417=CARTESIAN_POINT('Ctrl Pts',(6.76751849164459,-0.49122657597837,4.33588597251985));
#53418=CARTESIAN_POINT('Ctrl Pts',(6.78342377033221,-0.60242093591639,4.17326997329048));
#53419=CARTESIAN_POINT('Ctrl Pts',(6.79932904901982,-0.624839182280325,
3.94995709318712));
#53420=CARTESIAN_POINT('Ctrl Pts',(6.81523432770743,-0.548195780923551,
3.76848141254984));
#53421=CARTESIAN_POINT('Ctrl Pts',(6.83113960639504,-0.471552379566775,
3.58700573191256));
#53422=CARTESIAN_POINT('Ctrl Pts',(6.84704488508266,-0.295847330489284,
3.44736725074137));
#53423=CARTESIAN_POINT('Ctrl Pts',(6.86295016377027,-0.101752734572189,
3.41368297698799));
#53424=CARTESIAN_POINT('Ctrl Pts',(6.87885544245788,0.0923418613449005,
3.37999870323461));
#53425=CARTESIAN_POINT('Ctrl Pts',(6.8947607211455,0.304826004101594,3.45226863689903));
#53426=CARTESIAN_POINT('Ctrl Pts',(6.91066599983311,0.438133727661537,3.59730899203965));
#53427=CARTESIAN_POINT('Ctrl Pts',(6.92657127852072,0.571441451221483,3.74234934718029));
#53428=CARTESIAN_POINT('Ctrl Pts',(6.94247655720833,0.625572755584675,3.96016012379713));
#53429=CARTESIAN_POINT('Ctrl Pts',(6.95838183589594,0.57567402069499,4.15073208753033));
#53430=CARTESIAN_POINT('Ctrl Pts',(6.97428711458356,0.525775285805305,4.34130405126353));
#53431=CARTESIAN_POINT('Ctrl Pts',(6.99019239327118,0.371846511662747,4.5046372021131));
#53432=CARTESIAN_POINT('Ctrl Pts',(7.00609767195879,0.184564651688987,4.56573572985967));
#53433=CARTESIAN_POINT('Ctrl Pts',(7.01111664422002,0.125467135782336,4.58501560681028));
#53434=CARTESIAN_POINT('Ctrl Pts',(7.01613561648126,0.0630485115161635,
4.59411554829291));
#53435=CARTESIAN_POINT('Ctrl Pts',(7.02115458874249,0.000491936389841303,
4.5936290357477));
#53436=CARTESIAN_POINT('Origin',(4.,0.,4.));
#53437=CARTESIAN_POINT('',(7.42884541125756,-0.000438237927964824,4.59464495791636));
#53438=CARTESIAN_POINT('',(7.32115458874249,-0.000317338366111653,4.59328419319629));
#53439=CARTESIAN_POINT('',(4.,-7.27562663373442E-17,4.5941));
#53440=CARTESIAN_POINT('Ctrl Pts',(7.42884541125756,-0.000438237927964824,
4.59464495791636));
#53441=CARTESIAN_POINT('Ctrl Pts',(7.41515859140615,0.169409178821721,4.5932420274804));
#53442=CARTESIAN_POINT('Ctrl Pts',(7.40147177155473,0.340360224580004,4.51673272682389));
#53443=CARTESIAN_POINT('Ctrl Pts',(7.38778495170331,0.450965110664874,4.38826722161738));
#53444=CARTESIAN_POINT('Ctrl Pts',(7.37187967301569,0.579497637321094,4.23897909740477));
#53445=CARTESIAN_POINT('Ctrl Pts',(7.35597439432808,0.626535888751401,4.01952688559808));
#53446=CARTESIAN_POINT('Ctrl Pts',(7.34006911564046,0.570481892017836,3.83067375781486));
#53447=CARTESIAN_POINT('Ctrl Pts',(7.32416383695285,0.51442789528427,3.64182063003164));
#53448=CARTESIAN_POINT('Ctrl Pts',(7.30825855826524,0.355281650386831,3.48356658627189));
#53449=CARTESIAN_POINT('Ctrl Pts',(7.29235327957763,0.166116376105148,3.42857518785077));
#53450=CARTESIAN_POINT('Ctrl Pts',(7.27644800089002,-0.023048898176535,
3.37358378942964));
#53451=CARTESIAN_POINT('Ctrl Pts',(7.2605427222024,-0.242233201842457,3.42185503634715));
#53452=CARTESIAN_POINT('Ctrl Pts',(7.24463744351479,-0.390796368104757,
3.5512248149675));
#53453=CARTESIAN_POINT('Ctrl Pts',(7.22873216482718,-0.539359534367058,
3.68059459358785));
#53454=CARTESIAN_POINT('Ctrl Pts',(7.21282688613957,-0.617301563225728,
3.89106290391106));
#53455=CARTESIAN_POINT('Ctrl Pts',(7.19692160745195,-0.588834786584626,
4.08599160058025));
#53456=CARTESIAN_POINT('Ctrl Pts',(7.18101632876434,-0.560368009943526,
4.28092029724944));
#53457=CARTESIAN_POINT('Ctrl Pts',(7.16511105007672,-0.425492427802657,
4.46030938026461));
#53458=CARTESIAN_POINT('Ctrl Pts',(7.14920577138911,-0.24613717474127,4.54179097474357));
#53459=CARTESIAN_POINT('Ctrl Pts',(7.1424189846786,-0.169606239833077,4.57655919310821));
#53460=CARTESIAN_POINT('Ctrl Pts',(7.13563219796808,-0.0849767524450092,
4.59350108952231));
#53461=CARTESIAN_POINT('Ctrl Pts',(7.12884541125757,-0.000233413975479213,
4.59320261234329));
#53462=CARTESIAN_POINT('Ctrl Pts',(7.02115458874249,0.000491936389841303,
4.5936290357477));
#53463=CARTESIAN_POINT('Ctrl Pts',(7.03204089516887,-0.135195214358064,
4.59257377495492));
#53464=CARTESIAN_POINT('Ctrl Pts',(7.04292720159524,-0.271531381894462,
4.54641716720817));
#53465=CARTESIAN_POINT('Ctrl Pts',(7.05381350802162,-0.376033620593693,
4.46121547122365));
#53466=CARTESIAN_POINT('Ctrl Pts',(7.06971878670923,-0.528715087097646,
4.33673278019746));
#53467=CARTESIAN_POINT('Ctrl Pts',(7.08562406539685,-0.613443074300594,
4.1289034935015));
#53468=CARTESIAN_POINT('Ctrl Pts',(7.10152934408446,-0.591314251018945,
3.93315398851514));
#53469=CARTESIAN_POINT('Ctrl Pts',(7.11743462277207,-0.569185427737295,
3.73740448352876));
#53470=CARTESIAN_POINT('Ctrl Pts',(7.13333990145968,-0.440199793971044,
3.55373476025198));
#53471=CARTESIAN_POINT('Ctrl Pts',(7.14924518014729,-0.263582002606135,
3.46647820559892));
#53472=CARTESIAN_POINT('Ctrl Pts',(7.16515045883491,-0.0869642112412332,
3.37922165094586));
#53473=CARTESIAN_POINT('Ctrl Pts',(7.18105573752253,0.137285737722324,3.38837826491652));
#53474=CARTESIAN_POINT('Ctrl Pts',(7.19696101621014,0.306201705590428,3.48974370695041));
#53475=CARTESIAN_POINT('Ctrl Pts',(7.21286629489775,0.47511767345854,3.59110914898431));
#53476=CARTESIAN_POINT('Ctrl Pts',(7.22877157358536,0.588699660231196,3.78468341908144));
#53477=CARTESIAN_POINT('Ctrl Pts',(7.24467685227297,0.594795648982816,3.98158540759));
#53478=CARTESIAN_POINT('Ctrl Pts',(7.26058213096058,0.600891637734436,4.17848739609855));
#53479=CARTESIAN_POINT('Ctrl Pts',(7.2764874096482,0.499501628465021,4.37871710301853));
#53480=CARTESIAN_POINT('Ctrl Pts',(7.29239268833581,0.337179610128186,4.49033751492072));
#53481=CARTESIAN_POINT('Ctrl Pts',(7.30197998847137,0.239335998647354,4.5576194790522));
#53482=CARTESIAN_POINT('Ctrl Pts',(7.31156728860693,0.119353510611835,4.59270637405629));
#53483=CARTESIAN_POINT('Ctrl Pts',(7.32115458874249,-0.000317338366111653,
4.59328419319629));
#53484=CARTESIAN_POINT('Origin',(4.,0.,4.));
#53485=CARTESIAN_POINT('',(7.72884541125757,0.000455182276646732,4.59460030787683));
#53486=CARTESIAN_POINT('',(7.62115458874249,-0.000367422317862595,4.59479267874092));
#53487=CARTESIAN_POINT('',(4.,-7.27562663373442E-17,4.5941));
#53488=CARTESIAN_POINT('Ctrl Pts',(7.72884541125757,0.000455182276646732,
4.59460030787683));
#53489=CARTESIAN_POINT('Ctrl Pts',(7.72649554221944,0.0296217258780686,
4.59484761241511));
#53490=CARTESIAN_POINT('Ctrl Pts',(7.72414567318131,0.0587549042441869,
4.59288776399295));
#53491=CARTESIAN_POINT('Ctrl Pts',(7.72179580414318,0.0875427725731367,
4.58860617484604));
#53492=CARTESIAN_POINT('Ctrl Pts',(7.70589052545556,0.282395788279217,4.55962589232715));
#53493=CARTESIAN_POINT('Ctrl Pts',(7.68998524676794,0.461428877889185,4.42427810603975));
#53494=CARTESIAN_POINT('Ctrl Pts',(7.67407996808033,0.542437620895056,4.24470879335187));
#53495=CARTESIAN_POINT('Ctrl Pts',(7.65817468939272,0.623446363900926,4.065139480664));
#53496=CARTESIAN_POINT('Ctrl Pts',(7.64226941070511,0.606430760302702,3.84134864157567));
#53497=CARTESIAN_POINT('Ctrl Pts',(7.6263641320175,0.499203655448083,3.67609156159133));
#53498=CARTESIAN_POINT('Ctrl Pts',(7.61045885332988,0.391976550593464,3.51083448160699));
#53499=CARTESIAN_POINT('Ctrl Pts',(7.59455357464227,0.19453794448245,3.40411116072664));
#53500=CARTESIAN_POINT('Ctrl Pts',(7.57864829595466,-0.00245670798462758,
3.40492443279829));
#53501=CARTESIAN_POINT('Ctrl Pts',(7.56274301726704,-0.199451360451705,
3.40573770486994));
#53502=CARTESIAN_POINT('Ctrl Pts',(7.54683773857943,-0.396002059274846,
3.5140875698936));
#53503=CARTESIAN_POINT('Ctrl Pts',(7.53093245989182,-0.50186103876401,3.68022435377194));
#53504=CARTESIAN_POINT('Ctrl Pts',(7.51502718120421,-0.607720018253171,
3.84636113765028));
#53505=CARTESIAN_POINT('Ctrl Pts',(7.4991219025166,-0.622887278408357,4.07028484038331));
#53506=CARTESIAN_POINT('Ctrl Pts',(7.48321662382898,-0.540398655351294,
4.24917917107494));
#53507=CARTESIAN_POINT('Ctrl Pts',(7.46731134514137,-0.45791003229423,4.42807350176658));
#53508=CARTESIAN_POINT('Ctrl Pts',(7.45140606645375,-0.277765526024924,
4.56193846041682));
#53509=CARTESIAN_POINT('Ctrl Pts',(7.43550078776614,-0.0826798719492015,
4.58930892143267));
#53510=CARTESIAN_POINT('Ctrl Pts',(7.43328232892995,-0.0554694406452989,
4.59312653709876));
#53511=CARTESIAN_POINT('Ctrl Pts',(7.43106387009376,-0.0279683367079049,
4.5948723550368));
#53512=CARTESIAN_POINT('Ctrl Pts',(7.42884541125756,-0.000438237927964824,
4.59464495791636));
#53513=CARTESIAN_POINT('Ctrl Pts',(7.32115458874249,-0.000317338366111653,
4.59328419319629));
#53514=CARTESIAN_POINT('Ctrl Pts',(7.32747256729455,-0.0791797758050172,
4.59366497286126));
#53515=CARTESIAN_POINT('Ctrl Pts',(7.3337905458466,-0.157906876560309,4.57905936436794));
#53516=CARTESIAN_POINT('Ctrl Pts',(7.34010852439865,-0.230073660466993,
4.54880513582638));
#53517=CARTESIAN_POINT('Ctrl Pts',(7.35601380308626,-0.411750885321067,
4.47264122794544));
#53518=CARTESIAN_POINT('Ctrl Pts',(7.37191908177388,-0.551851307624962,
4.29730229529918));
#53519=CARTESIAN_POINT('Ctrl Pts',(7.38782436046149,-0.586046744500155,
4.10329655692985));
#53520=CARTESIAN_POINT('Ctrl Pts',(7.4037296391491,-0.620242181375348,3.90929081856053));
#53521=CARTESIAN_POINT('Ctrl Pts',(7.41963491783671,-0.548532632821828,
3.69661827446815));
#53522=CARTESIAN_POINT('Ctrl Pts',(7.43554019652432,-0.403844087697925,
3.56292915991696));
#53523=CARTESIAN_POINT('Ctrl Pts',(7.45144547521194,-0.259155542574025,
3.42924004536577));
#53524=CARTESIAN_POINT('Ctrl Pts',(7.46735075389955,-0.0414880008797467,
3.37453436035576));
#53525=CARTESIAN_POINT('Ctrl Pts',(7.48325603258717,0.149214809903968,3.42393064079835));
#53526=CARTESIAN_POINT('Ctrl Pts',(7.49916131127478,0.339917620687686,3.47332692124094));
#53527=CARTESIAN_POINT('Ctrl Pts',(7.51506658996239,0.50365570056084,3.62682516713614));
#53528=CARTESIAN_POINT('Ctrl Pts',(7.53097186865001,0.56524745100941,3.81394547807041));
#53529=CARTESIAN_POINT('Ctrl Pts',(7.54687714733762,0.626839201457978,4.00106578900469));
#53530=CARTESIAN_POINT('Ctrl Pts',(7.56278242602523,0.58628462248197,4.22180816497804));
#53531=CARTESIAN_POINT('Ctrl Pts',(7.57868770471284,0.462204660718925,4.3748170457164));
#53532=CARTESIAN_POINT('Ctrl Pts',(7.59284333272272,0.351774041004839,4.51099427596058));
#53533=CARTESIAN_POINT('Ctrl Pts',(7.60699896073261,0.175183620117616,4.59352033541115));
#53534=CARTESIAN_POINT('Ctrl Pts',(7.62115458874249,-0.000367422317862596,
4.59479267874092));
#53535=CARTESIAN_POINT('Origin',(4.,0.,4.));
#53536=CARTESIAN_POINT('',(8.02884541125756,0.000208508845897126,4.59318438507865));
#53537=CARTESIAN_POINT('',(7.92115458874249,0.000504499356536197,4.59443266285439));
#53538=CARTESIAN_POINT('',(4.,-7.27562663373442E-17,4.5941));
#53539=CARTESIAN_POINT('Ctrl Pts',(8.02884541125756,0.000208508845897126,
4.59318438507865));
#53540=CARTESIAN_POINT('Ctrl Pts',(8.02192721434511,0.0865993248636432,
4.5934556945658));
#53541=CARTESIAN_POINT('Ctrl Pts',(8.01500901743265,0.17288466952141,4.57582457789876));
#53542=CARTESIAN_POINT('Ctrl Pts',(8.0080908205202,0.250602156771344,4.53974023855861));
#53543=CARTESIAN_POINT('Ctrl Pts',(7.99218554183259,0.42927852421987,4.4567805482338));
#53544=CARTESIAN_POINT('Ctrl Pts',(7.97628026314498,0.562668370741438,4.27628395749428));
#53545=CARTESIAN_POINT('Ctrl Pts',(7.96037498445736,0.589524722071826,4.08112686462655));
#53546=CARTESIAN_POINT('Ctrl Pts',(7.94446970576975,0.616381073402214,3.88596977175883));
#53547=CARTESIAN_POINT('Ctrl Pts',(7.92856442708213,0.536703929541425,3.67615217676291));
#53548=CARTESIAN_POINT('Ctrl Pts',(7.91265914839452,0.387077664089382,3.54801344261061));
#53549=CARTESIAN_POINT('Ctrl Pts',(7.89675386970691,0.237451398637336,3.41987470845831));
#53550=CARTESIAN_POINT('Ctrl Pts',(7.88084859101929,0.0178760115940344,
3.37341483514963));
#53551=CARTESIAN_POINT('Ctrl Pts',(7.86494331233168,-0.170828768780714,
3.42996623095257));
#53552=CARTESIAN_POINT('Ctrl Pts',(7.84903803364407,-0.359533549155462,
3.48651762675552));
#53553=CARTESIAN_POINT('Ctrl Pts',(7.83313275495647,-0.517367722861657,
3.64608029167009));
#53554=CARTESIAN_POINT('Ctrl Pts',(7.81722747626885,-0.571860514742998,
3.83538980050754));
#53555=CARTESIAN_POINT('Ctrl Pts',(7.80132219758124,-0.626353306624339,
4.02469930934499));
#53556=CARTESIAN_POINT('Ctrl Pts',(7.78541691889362,-0.577504716680827,
4.24375566210532));
#53557=CARTESIAN_POINT('Ctrl Pts',(7.769511640206,-0.447743950807975,4.3919774491103));
#53558=CARTESIAN_POINT('Ctrl Pts',(7.75595623055652,-0.337154229471824,
4.51830073342946));
#53559=CARTESIAN_POINT('Ctrl Pts',(7.74240082090705,-0.16779438404434,4.593173711641));
#53560=CARTESIAN_POINT('Ctrl Pts',(7.72884541125757,0.000455182276646732,
4.59460030787683));
#53561=CARTESIAN_POINT('Ctrl Pts',(7.62115458874249,-0.000367422317862596,
4.59479267874092));
#53562=CARTESIAN_POINT('Ctrl Pts',(7.62290423942022,-0.022065717876263,
4.59494994172972));
#53563=CARTESIAN_POINT('Ctrl Pts',(7.62465389009795,-0.043748134618359,
4.59386587358433));
#53564=CARTESIAN_POINT('Ctrl Pts',(7.62640354077568,-0.0652877816099521,
4.59148835294282));
#53565=CARTESIAN_POINT('Ctrl Pts',(7.64230881946329,-0.261094917625702,
4.56987539392751));
#53566=CARTESIAN_POINT('Ctrl Pts',(7.6582140981509,-0.445103845107109,4.44137409039354));
#53567=CARTESIAN_POINT('Ctrl Pts',(7.67411937683852,-0.532825449416136,
4.2649868044631));
#53568=CARTESIAN_POINT('Ctrl Pts',(7.69002465552613,-0.620547053725161,
4.08859951853267));
#53569=CARTESIAN_POINT('Ctrl Pts',(7.70592993421374,-0.611981334861803,
3.86432625020577));
#53570=CARTESIAN_POINT('Ctrl Pts',(7.72183521290136,-0.511061308497056,
3.69514379608856));
#53571=CARTESIAN_POINT('Ctrl Pts',(7.73774049158897,-0.410141282132307,
3.52596134197134));
#53572=CARTESIAN_POINT('Ctrl Pts',(7.75364577027658,-0.216866948266163,
3.4118697020638));
#53573=CARTESIAN_POINT('Ctrl Pts',(7.76955104896419,-0.0199817042712483,
3.40525493058698));
#53574=CARTESIAN_POINT('Ctrl Pts',(7.78545632765181,0.176903539723664,3.39864015911017));
#53575=CARTESIAN_POINT('Ctrl Pts',(7.80136160633942,0.377399693847348,3.49950225606407));
#53576=CARTESIAN_POINT('Ctrl Pts',(7.81726688502703,0.489447406431712,3.66152961365368));
#53577=CARTESIAN_POINT('Ctrl Pts',(7.83317216371464,0.601495119016078,3.82355697124329));
#53578=CARTESIAN_POINT('Ctrl Pts',(7.84907744240226,0.625094390061116,4.04674958946861));
#53579=CARTESIAN_POINT('Ctrl Pts',(7.86498272108987,0.549409432699027,4.22862686054007));
#53580=CARTESIAN_POINT('Ctrl Pts',(7.88088799977748,0.473724475336938,4.41050413161152));
#53581=CARTESIAN_POINT('Ctrl Pts',(7.89679327846509,0.298755289567731,4.55106605552911));
#53582=CARTESIAN_POINT('Ctrl Pts',(7.91269855715271,0.104840323164387,4.58577254351526));
#53583=CARTESIAN_POINT('Ctrl Pts',(7.9155172343493,0.0704753991278659,4.59192310448195));
#53584=CARTESIAN_POINT('Ctrl Pts',(7.91833591154589,0.0355154700816755,
4.59474920414003));
#53585=CARTESIAN_POINT('Ctrl Pts',(7.92115458874249,0.000504499356536197,
4.59443266285439));
#53586=CARTESIAN_POINT('Origin',(4.,0.,4.));
#53587=CARTESIAN_POINT('',(8.32884541125757,-0.000534402448739424,4.5938336238991));
#53588=CARTESIAN_POINT('',(8.2211545887425,0.000116005647334215,4.59313666129657));
#53589=CARTESIAN_POINT('',(4.,-7.27562663373442E-17,4.5941));
#53590=CARTESIAN_POINT('Ctrl Pts',(8.32884541125757,-0.000534402448739424,
4.5938336238991));
#53591=CARTESIAN_POINT('Ctrl Pts',(8.31735888647079,0.142509087977489,4.59259298046846));
#53592=CARTESIAN_POINT('Ctrl Pts',(8.30587236168401,0.286359812054371,4.54070236535691));
#53593=CARTESIAN_POINT('Ctrl Pts',(8.29438583689723,0.393155811111917,4.44670960845581));
#53594=CARTESIAN_POINT('Ctrl Pts',(8.27848055820962,0.541035187969857,4.31655875596735));
#53595=CARTESIAN_POINT('Ctrl Pts',(8.262575279522,0.617867056310918,4.10568264439756));
#53596=CARTESIAN_POINT('Ctrl Pts',(8.24667000083439,0.588373472681163,3.91090666274675));
#53597=CARTESIAN_POINT('Ctrl Pts',(8.23076472214677,0.558879889051408,3.71613068109593));
#53598=CARTESIAN_POINT('Ctrl Pts',(8.21485944345917,0.423060853450833,3.53745482936408));
#53599=CARTESIAN_POINT('Ctrl Pts',(8.19895416477155,0.243278720997716,3.45691949951456));
#53600=CARTESIAN_POINT('Ctrl Pts',(8.18304888608394,0.0634965885445972,
3.37638416966503));
#53601=CARTESIAN_POINT('Ctrl Pts',(8.16714360739632,-0.160248640761069,
3.39398936169784));
#53602=CARTESIAN_POINT('Ctrl Pts',(8.15123832870871,-0.325222623502191,
3.50165151624576));
#53603=CARTESIAN_POINT('Ctrl Pts',(8.1353330500211,-0.490196606243315,3.60931367079368));
#53604=CARTESIAN_POINT('Ctrl Pts',(8.11942777133349,-0.59639934241989,3.80703278785672));
#53605=CARTESIAN_POINT('Ctrl Pts',(8.10352249264588,-0.595067028646789,
4.00402461368555));
#53606=CARTESIAN_POINT('Ctrl Pts',(8.08761721395827,-0.593734714873688,
4.20101643951437));
#53607=CARTESIAN_POINT('Ctrl Pts',(8.07171193527065,-0.484867351150922,
4.39728097410898));
#53608=CARTESIAN_POINT('Ctrl Pts',(8.05580665658303,-0.3184522251018,4.50270184645125));
#53609=CARTESIAN_POINT('Ctrl Pts',(8.04681957480788,-0.224421408301879,
4.56226861162124));
#53610=CARTESIAN_POINT('Ctrl Pts',(8.03783249303272,-0.112017456676448,
4.59283194056482));
#53611=CARTESIAN_POINT('Ctrl Pts',(8.02884541125756,0.000208508845897126,
4.59318438507865));
#53612=CARTESIAN_POINT('Ctrl Pts',(7.92115458874249,0.000504499356536197,
4.59443266285439));
#53613=CARTESIAN_POINT('Ctrl Pts',(7.93424119023351,-0.162045019349314,
4.59296301969496));
#53614=CARTESIAN_POINT('Ctrl Pts',(7.94732779172453,-0.325694779556815,
4.52375140444135));
#53615=CARTESIAN_POINT('Ctrl Pts',(7.96041439321555,-0.436005268305889,
4.40499428651169));
#53616=CARTESIAN_POINT('Ctrl Pts',(7.97631967190316,-0.570075146335334,
4.26065848946726));
#53617=CARTESIAN_POINT('Ctrl Pts',(7.99222495059077,-0.625354155356748,
4.04313584332371));
#53618=CARTESIAN_POINT('Ctrl Pts',(8.00813022927838,-0.576460513088508,
3.85230354456612));
#53619=CARTESIAN_POINT('Ctrl Pts',(8.024035507966,-0.527566870820267,3.66147124580852));
#53620=CARTESIAN_POINT('Ctrl Pts',(8.03994078665361,-0.374500577262366,
3.49732929443689));
#53621=CARTESIAN_POINT('Ctrl Pts',(8.05584606534123,-0.187543198716277,
3.43524473024767));
#53622=CARTESIAN_POINT('Ctrl Pts',(8.07175134402884,-0.000585820170193818,
3.37316016605846));
#53623=CARTESIAN_POINT('Ctrl Pts',(8.08765662271645,0.220262643364076,3.41313298905166));
#53624=CARTESIAN_POINT('Ctrl Pts',(8.10356190140406,0.37359792075985,3.53680937001953));
#53625=CARTESIAN_POINT('Ctrl Pts',(8.11946718009167,0.526933198155627,3.66048575098741));
#53626=CARTESIAN_POINT('Ctrl Pts',(8.13537245877928,0.612755289412907,3.86786568992997));
#53627=CARTESIAN_POINT('Ctrl Pts',(8.1512777374669,0.591658321059451,4.06372909240644));
#53628=CARTESIAN_POINT('Ctrl Pts',(8.16718301615451,0.570561352705995,4.2595924948829));
#53629=CARTESIAN_POINT('Ctrl Pts',(8.18308829484212,0.44254532474181,4.44393936089328));
#53630=CARTESIAN_POINT('Ctrl Pts',(8.19899357352974,0.266389781296621,4.53212540863836));
#53631=CARTESIAN_POINT('Ctrl Pts',(8.20638057860065,0.184576572093718,4.57308230066594));
#53632=CARTESIAN_POINT('Ctrl Pts',(8.21376758367158,0.0923795717789203,
4.59329710918813));
#53633=CARTESIAN_POINT('Ctrl Pts',(8.2211545887425,0.000116005647334215,
4.59313666129657));
#53634=CARTESIAN_POINT('Origin',(4.,0.,4.));
#53635=CARTESIAN_POINT('',(8.62884541125757,3.48566139269993E-5,4.59507810043999));
#53636=CARTESIAN_POINT('',(8.5211545887425,-0.000547905086566465,4.594005652201));
#53637=CARTESIAN_POINT('',(4.,-7.27562663373442E-17,4.5941));
#53638=CARTESIAN_POINT('Ctrl Pts',(8.62884541125757,3.48566139269993E-5,
4.59507810043999));
#53639=CARTESIAN_POINT('Ctrl Pts',(8.62869583728408,0.00188744051982823,
4.59507966949126));
#53640=CARTESIAN_POINT('Ctrl Pts',(8.62854626331059,0.00374001065808006,
4.59507176912216));
#53641=CARTESIAN_POINT('Ctrl Pts',(8.6283966893371,0.00559249142073073,
4.59505435897699));
#53642=CARTESIAN_POINT('Ctrl Pts',(8.61249141064948,0.202580123064263,4.59320301275402));
#53643=CARTESIAN_POINT('Ctrl Pts',(8.59658613196187,0.398557131004382,4.48381890612783));
#53644=CARTESIAN_POINT('Ctrl Pts',(8.58068085327426,0.503539164298441,4.31712659320126));
#53645=CARTESIAN_POINT('Ctrl Pts',(8.56477557458664,0.608521197592498,4.15043428027469));
#53646=CARTESIAN_POINT('Ctrl Pts',(8.54887029589904,0.622508256240502,3.92643376104774));
#53647=CARTESIAN_POINT('Ctrl Pts',(8.53296501721142,0.539078074654942,3.74797659726896));
#53648=CARTESIAN_POINT('Ctrl Pts',(8.51705973852381,0.455647893069379,3.56951943349019));
#53649=CARTESIAN_POINT('Ctrl Pts',(8.50115445983619,0.274800471250253,3.43660562515959));
#53650=CARTESIAN_POINT('Ctrl Pts',(8.48524918114857,0.0795732942734406,
3.41026356994308));
#53651=CARTESIAN_POINT('Ctrl Pts',(8.46934390246096,-0.115653882703369,
3.38392151472657));
#53652=CARTESIAN_POINT('Ctrl Pts',(8.45343862377335,-0.32526081483786,3.46415121262414));
#53653=CARTESIAN_POINT('Ctrl Pts',(8.43753334508574,-0.453004866631874,
3.61411458059983));
#53654=CARTESIAN_POINT('Ctrl Pts',(8.42162806639813,-0.580748918425883,
3.76407794857552));
#53655=CARTESIAN_POINT('Ctrl Pts',(8.40572278771052,-0.626630089879422,
3.98377498662932));
#53656=CARTESIAN_POINT('Ctrl Pts',(8.3898175090229,-0.569581688133314,4.17233010950212));
#53657=CARTESIAN_POINT('Ctrl Pts',(8.37391223033529,-0.512533286387202,
4.36088523237493));
#53658=CARTESIAN_POINT('Ctrl Pts',(8.35800695164768,-0.352555311441432,
4.51829844006673));
#53659=CARTESIAN_POINT('Ctrl Pts',(8.34210167296007,-0.163102881281137,
4.57229224720906));
#53660=CARTESIAN_POINT('Ctrl Pts',(8.33768291905923,-0.110469810133188,
4.58729263485501));
#53661=CARTESIAN_POINT('Ctrl Pts',(8.3332641651584,-0.0555618361628184,
4.59431088730997));
#53662=CARTESIAN_POINT('Ctrl Pts',(8.32884541125757,-0.000534402448739424,
4.5938336238991));
#53663=CARTESIAN_POINT('Ctrl Pts',(8.2211545887425,0.000116005647334215,
4.59313666129657));
#53664=CARTESIAN_POINT('Ctrl Pts',(8.22967286235919,-0.106277085140544,
4.59295164192424));
#53665=CARTESIAN_POINT('Ctrl Pts',(8.23819113597589,-0.212758691085218,
4.56567285125378));
#53666=CARTESIAN_POINT('Ctrl Pts',(8.24670940959258,-0.303508593564514,
4.51186277431583));
#53667=CARTESIAN_POINT('Ctrl Pts',(8.26261468828019,-0.472956366054245,
4.41138886276846));
#53668=CARTESIAN_POINT('Ctrl Pts',(8.2785199669678,-0.587556852107514,4.21841581019395));
#53669=CARTESIAN_POINT('Ctrl Pts',(8.29442524565541,-0.594690356875377,
4.02154867831793));
#53670=CARTESIAN_POINT('Ctrl Pts',(8.31033052434302,-0.60182386164324,3.82468154644191));
#53671=CARTESIAN_POINT('Ctrl Pts',(8.32623580303064,-0.501490385125681,
3.62392033526436));
#53672=CARTESIAN_POINT('Ctrl Pts',(8.34214108171825,-0.339758814980244,
3.51144609945163));
#53673=CARTESIAN_POINT('Ctrl Pts',(8.35804636040587,-0.178027244834812,
3.3989718636389));
#53674=CARTESIAN_POINT('Ctrl Pts',(8.37395163909348,0.0451024189384938,
3.37478460319097));
#53675=CARTESIAN_POINT('Ctrl Pts',(8.38985691778109,0.227178474572579,3.44999008482693));
#53676=CARTESIAN_POINT('Ctrl Pts',(8.4057621964687,0.40925453020667,3.5251955664629));
#53677=CARTESIAN_POINT('Ctrl Pts',(8.42166747515631,0.550276977701535,3.69979379018275));
#53678=CARTESIAN_POINT('Ctrl Pts',(8.43757275384392,0.585494275335268,3.89361663829603));
#53679=CARTESIAN_POINT('Ctrl Pts',(8.45347803253154,0.620711572969,4.0874394864093));
#53680=CARTESIAN_POINT('Ctrl Pts',(8.46938331121915,0.550123720741606,4.30048695891599));
#53681=CARTESIAN_POINT('Ctrl Pts',(8.48528858990677,0.406141674070155,4.4349366697363));
#53682=CARTESIAN_POINT('Ctrl Pts',(8.49724392285201,0.297916389879728,4.53599689564107));
#53683=CARTESIAN_POINT('Ctrl Pts',(8.50919925579725,0.148224117540273,4.59265016978245));
#53684=CARTESIAN_POINT('Ctrl Pts',(8.5211545887425,-0.000547905086566465,
4.594005652201));
#53685=CARTESIAN_POINT('Origin',(4.,0.,4.));
#53686=CARTESIAN_POINT('',(8.92884541125757,0.000516595407308196,4.59372894893997));
#53687=CARTESIAN_POINT('',(8.82115458874249,0.000142235148737217,4.59503945166131));
#53688=CARTESIAN_POINT('',(4.,-7.27562663373442E-17,4.5941));
#53689=CARTESIAN_POINT('Ctrl Pts',(8.92884541125757,0.000516595407308196,
4.59372894893997));
#53690=CARTESIAN_POINT('Ctrl Pts',(8.92412750940976,0.0592956068199462,
4.59421507565108));
#53691=CARTESIAN_POINT('Ctrl Pts',(8.91940960756194,0.117944888069788,4.58619493689145));
#53692=CARTESIAN_POINT('Ctrl Pts',(8.91469170571413,0.17383025386194,4.56912565303288));
#53693=CARTESIAN_POINT('Ctrl Pts',(8.89878642702651,0.362234410233906,4.51158064138869));
#53694=CARTESIAN_POINT('Ctrl Pts',(8.8828811483389,0.519225559109383,4.35118846702123));
#53695=CARTESIAN_POINT('Ctrl Pts',(8.86697586965128,0.572720006672535,4.16159443076672));
#53696=CARTESIAN_POINT('Ctrl Pts',(8.85107059096367,0.626214454235688,3.97200039451221));
#53697=CARTESIAN_POINT('Ctrl Pts',(8.83516531227606,0.576212200486512,3.75320449637065));
#53698=CARTESIAN_POINT('Ctrl Pts',(8.81926003358845,0.445672164925724,3.60566855627755));
#53699=CARTESIAN_POINT('Ctrl Pts',(8.80335475490084,0.315132129364936,3.45813261618446));
#53700=CARTESIAN_POINT('Ctrl Pts',(8.78744947621322,0.104054311992536,3.38185663413984));
#53701=CARTESIAN_POINT('Ctrl Pts',(8.77154419752561,-0.0906432834200916,
3.41186331412789));
#53702=CARTESIAN_POINT('Ctrl Pts',(8.755638918838,-0.285340878832719,3.44186999411594));
#53703=CARTESIAN_POINT('Ctrl Pts',(8.73973364015038,-0.463658252285575,
3.57815933613666));
#53704=CARTESIAN_POINT('Ctrl Pts',(8.72382836146277,-0.543719609875046,
3.75815304026071));
#53705=CARTESIAN_POINT('Ctrl Pts',(8.70792308277515,-0.623780967464517,
3.93814674438476));
#53706=CARTESIAN_POINT('Ctrl Pts',(8.69201780408754,-0.605586309190603,
4.16184481061213));
#53707=CARTESIAN_POINT('Ctrl Pts',(8.67611252539993,-0.497489852380174,
4.32653455081593));
#53708=CARTESIAN_POINT('Ctrl Pts',(8.66035682068581,-0.390409939629295,
4.48967554111606));
#53709=CARTESIAN_POINT('Ctrl Pts',(8.64460111597169,-0.195111159088962,
4.59491282095998));
#53710=CARTESIAN_POINT('Ctrl Pts',(8.62884541125757,3.48566139269993E-5,
4.59507810043999));
#53711=CARTESIAN_POINT('Ctrl Pts',(8.5211545887425,-0.000547905086566465,
4.594005652201));
#53712=CARTESIAN_POINT('Ctrl Pts',(8.52510453448487,-0.0497009834700827,
4.59445349267793));
#53713=CARTESIAN_POINT('Ctrl Pts',(8.52905448022724,-0.0987536084630192,
4.58886509038946));
#53714=CARTESIAN_POINT('Ctrl Pts',(8.53300442596961,-0.146177075786514,
4.57684766499685));
#53715=CARTESIAN_POINT('Ctrl Pts',(8.54890970465722,-0.337137537856201,
4.52845700030318));
#53716=CARTESIAN_POINT('Ctrl Pts',(8.56481498334483,-0.501682220880061,
4.37582372178193));
#53717=CARTESIAN_POINT('Ctrl Pts',(8.58072026203244,-0.564259167724997,
4.18903057354857));
#53718=CARTESIAN_POINT('Ctrl Pts',(8.59662554072005,-0.626836114569933,
4.00223742531521));
#53719=CARTESIAN_POINT('Ctrl Pts',(8.61253081940767,-0.587445325235947,
3.78128440736974));
#53720=CARTESIAN_POINT('Ctrl Pts',(8.62843609809528,-0.464173383698336,
3.62762379780141));
#53721=CARTESIAN_POINT('Ctrl Pts',(8.6443413767829,-0.340901442160722,3.47396318823307));
#53722=CARTESIAN_POINT('Ctrl Pts',(8.66024665547051,-0.133748348419481,
3.38759498704188));
#53723=CARTESIAN_POINT('Ctrl Pts',(8.67615193415812,0.0621699608040676,
3.40817581827756));
#53724=CARTESIAN_POINT('Ctrl Pts',(8.69205721284573,0.25808827002761,3.42875664951325));
#53725=CARTESIAN_POINT('Ctrl Pts',(8.70796249153334,0.44277179473346,3.55628651317581));
#53726=CARTESIAN_POINT('Ctrl Pts',(8.72386777022095,0.531421673692279,3.73220909121499));
#53727=CARTESIAN_POINT('Ctrl Pts',(8.73977304890857,0.620071552651101,3.90813166925417));
#53728=CARTESIAN_POINT('Ctrl Pts',(8.75567832759618,0.612687785862888,4.13244696166997));
#53729=CARTESIAN_POINT('Ctrl Pts',(8.7715836062838,0.512660686655375,4.30215887618246));
#53730=CARTESIAN_POINT('Ctrl Pts',(8.78748888497141,0.412633587447865,4.47187079069495));
#53731=CARTESIAN_POINT('Ctrl Pts',(8.80339416365902,0.21996315582106,4.58697932730413));
#53732=CARTESIAN_POINT('Ctrl Pts',(8.81929944234663,0.0231155027642346,
4.59463151583965));
#53733=CARTESIAN_POINT('Ctrl Pts',(8.81991782447859,0.0154622529370322,
4.59492902566351));
#53734=CARTESIAN_POINT('Ctrl Pts',(8.82053620661054,0.00780268890311657,
4.59506410656044));
#53735=CARTESIAN_POINT('Ctrl Pts',(8.82115458874249,0.000142235148737217,
4.59503945166131));
#53736=CARTESIAN_POINT('Origin',(4.,0.,4.));
#53737=CARTESIAN_POINT('',(9.22884541125756,-0.000264402795292107,4.59322887297718));
#53738=CARTESIAN_POINT('',(9.12115458874249,0.000475196148639644,4.59357609051269));
#53739=CARTESIAN_POINT('',(4.,-7.27562663373442E-17,4.5941));
#53740=CARTESIAN_POINT('Ctrl Pts',(9.22884541125756,-0.000264402795292107,
4.59322887297718));
#53741=CARTESIAN_POINT('Ctrl Pts',(9.21955918153543,0.115675446261185,4.59276508993807));
#53742=CARTESIAN_POINT('Ctrl Pts',(9.21027295181329,0.231857423975292,4.55999255403315));
#53743=CARTESIAN_POINT('Ctrl Pts',(9.20098672209116,0.327844211240712,4.49662776730038));
#53744=CARTESIAN_POINT('Ctrl Pts',(9.18508144340355,0.492248565587605,4.38809775866155));
#53745=CARTESIAN_POINT('Ctrl Pts',(9.16917616471593,0.597407924103304,4.18982173958679));
#53746=CARTESIAN_POINT('Ctrl Pts',(9.15327088602831,0.595037558282966,3.99283966966863));
#53747=CARTESIAN_POINT('Ctrl Pts',(9.1373656073407,0.592667192462628,3.79585759975047));
#53748=CARTESIAN_POINT('Ctrl Pts',(9.12146032865309,0.482767102306254,3.60016947898891));
#53749=CARTESIAN_POINT('Ctrl Pts',(9.10555504996548,0.315798759724268,3.49562701355602));
#53750=CARTESIAN_POINT('Ctrl Pts',(9.08964977127787,0.148830417142278,3.39108454812312));
#53751=CARTESIAN_POINT('Ctrl Pts',(9.07374449259025,-0.0752061778653251,
3.37768773801888));
#53752=CARTESIAN_POINT('Ctrl Pts',(9.05783921390264,-0.253442899077741,
3.46158783167087));
#53753=CARTESIAN_POINT('Ctrl Pts',(9.04193393521502,-0.431679620290152,
3.54548792532286));
#53754=CARTESIAN_POINT('Ctrl Pts',(9.02602865652741,-0.56411646770738,3.72668492273107));
#53755=CARTESIAN_POINT('Ctrl Pts',(9.0101233778398,-0.589944043936388,3.92198082849844));
#53756=CARTESIAN_POINT('Ctrl Pts',(8.99421809915219,-0.615771620165397,
4.11727673426582));
#53757=CARTESIAN_POINT('Ctrl Pts',(8.97831282046457,-0.534989925206181,
4.32667154839236));
#53758=CARTESIAN_POINT('Ctrl Pts',(8.96240754177696,-0.384690495792338,
4.45402003099517));
#53759=CARTESIAN_POINT('Ctrl Pts',(8.95122016493716,-0.278973620993485,
4.54359378149875));
#53760=CARTESIAN_POINT('Ctrl Pts',(8.94003278809737,-0.138863784294423,
4.59257621560968));
#53761=CARTESIAN_POINT('Ctrl Pts',(8.92884541125757,0.000516595407308196,
4.59372894893997));
#53762=CARTESIAN_POINT('Ctrl Pts',(8.82115458874249,0.000142235148737217,
4.59503945166131));
#53763=CARTESIAN_POINT('Ctrl Pts',(8.83644148529816,-0.189230254871984,
4.59442996300828));
#53764=CARTESIAN_POINT('Ctrl Pts',(8.85172838185382,-0.379146468724227,
4.49620311855542));
#53765=CARTESIAN_POINT('Ctrl Pts',(8.86701527840948,-0.487657002993039,
4.34104488491935));
#53766=CARTESIAN_POINT('Ctrl Pts',(8.88292055709709,-0.600556981206626,
4.17961022500168));
#53767=CARTESIAN_POINT('Ctrl Pts',(8.89882583578469,-0.62533206314696,3.95654506470448));
#53768=CARTESIAN_POINT('Ctrl Pts',(8.91473111447231,-0.550606579334316,
3.77427148852754));
#53769=CARTESIAN_POINT('Ctrl Pts',(8.93063639315992,-0.47588109552167,3.5919979123506));
#53770=CARTESIAN_POINT('Ctrl Pts',(8.94654167184753,-0.301655045956043,
3.45051592029392));
#53771=CARTESIAN_POINT('Ctrl Pts',(8.96244695053515,-0.107925661701669,
3.41478805750048));
#53772=CARTESIAN_POINT('Ctrl Pts',(8.97835222922276,0.0858037225526985,
3.37906019470703));
#53773=CARTESIAN_POINT('Ctrl Pts',(8.99425750791037,0.299036441495806,3.4490864611768));
#53774=CARTESIAN_POINT('Ctrl Pts',(9.01016278659798,0.433865051721373,3.5927137579139));
#53775=CARTESIAN_POINT('Ctrl Pts',(9.0260680652856,0.568693661946943,3.736341054651));
#53776=CARTESIAN_POINT('Ctrl Pts',(9.04197334397321,0.625118163454969,3.95356938165542));
#53777=CARTESIAN_POINT('Ctrl Pts',(9.05787862266082,0.577230812276762,4.14465668133936));
#53778=CARTESIAN_POINT('Ctrl Pts',(9.07378390134844,0.529343461098555,4.3357439810233));
#53779=CARTESIAN_POINT('Ctrl Pts',(9.08968918003605,0.377144257234124,4.50069025338676));
#53780=CARTESIAN_POINT('Ctrl Pts',(9.10559445872366,0.190516636080703,4.56375914846174));
#53781=CARTESIAN_POINT('Ctrl Pts',(9.11078116872994,0.129657384941762,4.58432590969837));
#53782=CARTESIAN_POINT('Ctrl Pts',(9.11596787873622,0.0651369761893139,
4.59405891310139));
#53783=CARTESIAN_POINT('Ctrl Pts',(9.12115458874249,0.000475196148639644,
4.59357609051269));
#53784=CARTESIAN_POINT('Origin',(4.,0.,4.));
#53785=CARTESIAN_POINT('',(9.52884541125756,-0.000414715089906426,4.59470005288553));
#53786=CARTESIAN_POINT('',(9.4211545887425,-0.000345133784900094,4.59331940772745));
#53787=CARTESIAN_POINT('',(4.,-7.27562663373442E-17,4.5941));
#53788=CARTESIAN_POINT('Ctrl Pts',(9.52884541125756,-0.000414715089906426,
4.59470005288553));
#53789=CARTESIAN_POINT('Ctrl Pts',(9.5149908536611,0.17147269131647,4.59333531965569));
#53790=CARTESIAN_POINT('Ctrl Pts',(9.50113629606464,0.344448366351018,4.51470554290992));
#53791=CARTESIAN_POINT('Ctrl Pts',(9.48728173846818,0.455032043431697,4.38349290156166));
#53792=CARTESIAN_POINT('Ctrl Pts',(9.47137645978057,0.581984072756561,4.23285845412795));
#53793=CARTESIAN_POINT('Ctrl Pts',(9.45547118109296,0.626706888961734,4.01292269047354));
#53794=CARTESIAN_POINT('Ctrl Pts',(9.43956590240535,0.56866566691212,3.82467080855373));
#53795=CARTESIAN_POINT('Ctrl Pts',(9.42366062371773,0.510624444862503,3.63641892663391));
#53796=CARTESIAN_POINT('Ctrl Pts',(9.40775534503012,0.349819184558098,3.47985092644869));
#53797=CARTESIAN_POINT('Ctrl Pts',(9.39185006634251,0.160084858421151,3.42685620983728));
#53798=CARTESIAN_POINT('Ctrl Pts',(9.37594478765489,-0.0296494677157886,
3.37386149322587));
#53799=CARTESIAN_POINT('Ctrl Pts',(9.36003950896728,-0.248312859685263,
3.42444006018826));
#53800=CARTESIAN_POINT('Ctrl Pts',(9.34413423027966,-0.395504338780113,
3.55536837257802));
#53801=CARTESIAN_POINT('Ctrl Pts',(9.32822895159205,-0.542695817874971,
3.6862966849678));
#53802=CARTESIAN_POINT('Ctrl Pts',(9.31232367290444,-0.618415384095196,
3.89757474278496));
#53803=CARTESIAN_POINT('Ctrl Pts',(9.29641839421683,-0.587895816063128,
4.09219260031737));
#53804=CARTESIAN_POINT('Ctrl Pts',(9.28051311552922,-0.55737624803106,4.28681045784976));
#53805=CARTESIAN_POINT('Ctrl Pts',(9.26460783684159,-0.42061754574671,4.4647681150974));
#53806=CARTESIAN_POINT('Ctrl Pts',(9.24870255815398,-0.240413519515492,
4.54435494461976));
#53807=CARTESIAN_POINT('Ctrl Pts',(9.24208350918851,-0.165420852186184,
4.57747534017911));
#53808=CARTESIAN_POINT('Ctrl Pts',(9.23546446022304,-0.0829041350566004,
4.59355944875842));
#53809=CARTESIAN_POINT('Ctrl Pts',(9.22884541125756,-0.000264402795292107,
4.59322887297718));
#53810=CARTESIAN_POINT('Ctrl Pts',(9.12115458874249,0.000475196148639644,
4.59357609051269));
#53811=CARTESIAN_POINT('Ctrl Pts',(9.13187315742383,-0.133151270259641,
4.59257831599443));
#53812=CARTESIAN_POINT('Ctrl Pts',(9.14259172610516,-0.267381477949042,
4.54795275857003));
#53813=CARTESIAN_POINT('Ctrl Pts',(9.1533102947865,-0.371151898503526,4.46515291500219));
#53814=CARTESIAN_POINT('Ctrl Pts',(9.16921557347411,-0.525136773491911,
4.34228626868117));
#53815=CARTESIAN_POINT('Ctrl Pts',(9.18512085216173,-0.612050485026272,
4.13536145825263));
#53816=CARTESIAN_POINT('Ctrl Pts',(9.20102613084934,-0.591985933785934,
3.93938960239856));
#53817=CARTESIAN_POINT('Ctrl Pts',(9.21693140953695,-0.571921382545595,
3.74341774654449));
#53818=CARTESIAN_POINT('Ctrl Pts',(9.23283668822456,-0.444878568530549,
3.55839884526489));
#53819=CARTESIAN_POINT('Ctrl Pts',(9.24874196691217,-0.269190177198291,
3.46928575052316));
#53820=CARTESIAN_POINT('Ctrl Pts',(9.26464724559978,-0.0935017858660342,
3.38017265578144));
#53821=CARTESIAN_POINT('Ctrl Pts',(9.28055252428739,0.130832182783434,3.38696536757758));
#53822=CARTESIAN_POINT('Ctrl Pts',(9.29645780297501,0.300807061133818,3.48654496003073));
#53823=CARTESIAN_POINT('Ctrl Pts',(9.31236308166262,0.470781939484206,3.58612455248389));
#53824=CARTESIAN_POINT('Ctrl Pts',(9.32826836035024,0.586397727535503,3.77849102559406));
#53825=CARTESIAN_POINT('Ctrl Pts',(9.34417363903785,0.594568546715174,3.97531783326339));
#53826=CARTESIAN_POINT('Ctrl Pts',(9.36007891772546,0.602739365894845,4.17214464093271));
#53827=CARTESIAN_POINT('Ctrl Pts',(9.37598419641307,0.503465216202894,4.37343178316119));
#53828=CARTESIAN_POINT('Ctrl Pts',(9.39188947510069,0.342328587234952,4.48675671999422));
#53829=CARTESIAN_POINT('Ctrl Pts',(9.40164451298129,0.243500144778355,4.55626125828842));
#53830=CARTESIAN_POINT('Ctrl Pts',(9.41139955086189,0.121401365174849,4.59267772446372));
#53831=CARTESIAN_POINT('Ctrl Pts',(9.4211545887425,-0.000345133784900094,
4.59331940772745));
#53832=CARTESIAN_POINT('Origin',(4.,0.,4.));
#53833=CARTESIAN_POINT('',(9.82884541125756,0.000474857175501747,4.59454166667424));
#53834=CARTESIAN_POINT('',(9.7211545887425,-0.000338423355870402,4.59484023865297));
#53835=CARTESIAN_POINT('',(4.,-7.27562663373442E-17,4.5941));
#53836=CARTESIAN_POINT('Ctrl Pts',(9.82884541125756,0.000474857175501747,
4.59454166667424));
#53837=CARTESIAN_POINT('Ctrl Pts',(9.82632780447438,0.0317313679687054,
4.59481419231428));
#53838=CARTESIAN_POINT('Ctrl Pts',(9.82381019769121,0.0629485386443197,
4.59256288124703));
#53839=CARTESIAN_POINT('Ctrl Pts',(9.82129259090804,0.093741277189286,4.58765086492638));
#53840=CARTESIAN_POINT('Ctrl Pts',(9.80538731222043,0.288278045752977,4.55661862072519));
#53841=CARTESIAN_POINT('Ctrl Pts',(9.78948203353282,0.465874751366426,4.41939150759219));
#53842=CARTESIAN_POINT('Ctrl Pts',(9.77357675484521,0.54498650030893,4.23897841027765));
#53843=CARTESIAN_POINT('Ctrl Pts',(9.7576714761576,0.624098249251433,4.05856531296313));
#53844=CARTESIAN_POINT('Ctrl Pts',(9.74176619746998,0.604725041522997,3.83496623146707));
#53845=CARTESIAN_POINT('Ctrl Pts',(9.72586091878237,0.495762234499694,3.67084840431546));
#53846=CARTESIAN_POINT('Ctrl Pts',(9.70995564009475,0.386799427476386,3.50673057716384));
#53847=CARTESIAN_POINT('Ctrl Pts',(9.69405036140714,0.188247021158209,3.40209400435668));
#53848=CARTESIAN_POINT('Ctrl Pts',(9.67814508271953,-0.00872811953311764,
3.40498337331868));
#53849=CARTESIAN_POINT('Ctrl Pts',(9.66223980403192,-0.205703260224436,
3.40787274228067));
#53850=CARTESIAN_POINT('Ctrl Pts',(9.6463345253443,-0.4011011352889,3.51828805301183));
#53851=CARTESIAN_POINT('Ctrl Pts',(9.63042924665669,-0.505203307099277,
3.68553126611098));
#53852=CARTESIAN_POINT('Ctrl Pts',(9.61452396796908,-0.609305478909656,
3.85277447921013));
#53853=CARTESIAN_POINT('Ctrl Pts',(9.59861868928147,-0.622111947465945,
4.07684559467727));
#53854=CARTESIAN_POINT('Ctrl Pts',(9.58271341059386,-0.537742524204099,
4.25486063595701));
#53855=CARTESIAN_POINT('Ctrl Pts',(9.56680813190624,-0.453373100942255,
4.43287567723675));
#53856=CARTESIAN_POINT('Ctrl Pts',(9.55090285321863,-0.271827785862281,
4.5648346443291));
#53857=CARTESIAN_POINT('Ctrl Pts',(9.53499757453102,-0.0764645071000137,
4.59014756226876));
#53858=CARTESIAN_POINT('Ctrl Pts',(9.53294685343987,-0.0512756623106346,
4.5934112419387));
#53859=CARTESIAN_POINT('Ctrl Pts',(9.53089613234871,-0.025857110284879,
4.59490205769144));
#53860=CARTESIAN_POINT('Ctrl Pts',(9.52884541125756,-0.000414715089906426,
4.59470005288553));
#53861=CARTESIAN_POINT('Ctrl Pts',(9.4211545887425,-0.000345133784900094,
4.59331940772745));
#53862=CARTESIAN_POINT('Ctrl Pts',(9.42730482954951,-0.0771024252662454,
4.59372396859559));
#53863=CARTESIAN_POINT('Ctrl Pts',(9.43345507035652,-0.153719688677923,
4.57990840728947));
#53864=CARTESIAN_POINT('Ctrl Pts',(9.43960531116353,-0.224276981305518,
4.55119942103951));
#53865=CARTESIAN_POINT('Ctrl Pts',(9.45551058985114,-0.406746812634079,
4.47695445381419));
#53866=CARTESIAN_POINT('Ctrl Pts',(9.47141586853875,-0.548687367047265,
4.30310178792596));
#53867=CARTESIAN_POINT('Ctrl Pts',(9.48732114722636,-0.58492554696818,4.10946721245096));
#53868=CARTESIAN_POINT('Ctrl Pts',(9.50322642591398,-0.621163726889096,
3.91583263697596));
#53869=CARTESIAN_POINT('Ctrl Pts',(9.5191317046016,-0.55169953231774,3.70241615191419));
#53870=CARTESIAN_POINT('Ctrl Pts',(9.53503698328921,-0.408427982613559,
3.56720957829912));
#53871=CARTESIAN_POINT('Ctrl Pts',(9.55094226197682,-0.265156432909381,
3.43200300468405));
#53872=CARTESIAN_POINT('Ctrl Pts',(9.56684754066442,-0.0480775280723801,
3.37500634251568));
#53873=CARTESIAN_POINT('Ctrl Pts',(9.58275281935204,0.14313528264739,3.42239004773181));
#53874=CARTESIAN_POINT('Ctrl Pts',(9.59865809803965,0.334348093367161,3.46977375294793));
#53875=CARTESIAN_POINT('Ctrl Pts',(9.61456337672728,0.499694809969701,3.62153782554855));
#53876=CARTESIAN_POINT('Ctrl Pts',(9.63046865541489,0.563255215433827,3.80799862400389));
#53877=CARTESIAN_POINT('Ctrl Pts',(9.6463739341025,0.626815620897955,3.99445942245922));
#53878=CARTESIAN_POINT('Ctrl Pts',(9.6622792127901,0.588589715223662,4.21561694676927));
#53879=CARTESIAN_POINT('Ctrl Pts',(9.67818449147771,0.466129217091882,4.36992501817411));
#53880=CARTESIAN_POINT('Ctrl Pts',(9.69250785723264,0.355848439261942,4.50888586187125));
#53881=CARTESIAN_POINT('Ctrl Pts',(9.70683122298757,0.177255492135987,4.59363345408847));
#53882=CARTESIAN_POINT('Ctrl Pts',(9.7211545887425,-0.000338423355870402,
4.59484023865297));
#53883=CARTESIAN_POINT('Origin',(4.,0.,4.));
#53884=CARTESIAN_POINT('',(10.1288454112576,0.000175993811045716,4.59316417414361));
#53885=CARTESIAN_POINT('',(10.0211545887425,0.000517772199431355,4.59437035498519));
#53886=CARTESIAN_POINT('',(4.,-7.27562663373442E-17,4.5941));
#53887=CARTESIAN_POINT('Ctrl Pts',(10.1288454112576,0.000175993811045716,
4.59316417414361));
#53888=CARTESIAN_POINT('Ctrl Pts',(10.1217594766001,0.0886689559287146,
4.59339827721605));
#53889=CARTESIAN_POINT('Ctrl Pts',(10.1146735419426,0.177068724884878,4.57486525982572));
#53890=CARTESIAN_POINT('Ctrl Pts',(10.1075876072851,0.256276603526552,4.53706914692868));
#53891=CARTESIAN_POINT('Ctrl Pts',(10.0916823285975,0.434068729046268,4.45223097977176));
#53892=CARTESIAN_POINT('Ctrl Pts',(10.0757770499098,0.565548899719798,4.27033860735548));
#53893=CARTESIAN_POINT('Ctrl Pts',(10.0598717712222,0.590346983641159,4.0749093118617));
#53894=CARTESIAN_POINT('Ctrl Pts',(10.0439664925346,0.61514506756252,3.87948001636793));
#53895=CARTESIAN_POINT('Ctrl Pts',(10.028061213847,0.533261064731712,3.67051379779667));
#53896=CARTESIAN_POINT('Ctrl Pts',(10.0121559351594,0.382292645022166,3.5439591030842));
#53897=CARTESIAN_POINT('Ctrl Pts',(9.99625065647179,0.231324225312614,3.41740440837173));
#53898=CARTESIAN_POINT('Ctrl Pts',(9.98034537778417,0.011271388724311,3.37326123751805));
#53899=CARTESIAN_POINT('Ctrl Pts',(9.96444009909655,-0.17682691184915,3.43179826703564));
#53900=CARTESIAN_POINT('Ctrl Pts',(9.94853482040894,-0.364925212422603,
3.49033529655323));
#53901=CARTESIAN_POINT('Ctrl Pts',(9.93262954172133,-0.521068976981223,
3.65155252644206));
#53902=CARTESIAN_POINT('Ctrl Pts',(9.91672426303372,-0.573563594737602,
3.84142582527571));
#53903=CARTESIAN_POINT('Ctrl Pts',(9.90081898434611,-0.626058212493981,
4.03129912410937));
#53904=CARTESIAN_POINT('Ctrl Pts',(9.8849137056585,-0.574903683448118,4.24982849188785));
#53905=CARTESIAN_POINT('Ctrl Pts',(9.86900842697089,-0.443588003168223,
4.39667448814241));
#53906=CARTESIAN_POINT('Ctrl Pts',(9.85562075506645,-0.333057953489513,
4.52027659892262));
#53907=CARTESIAN_POINT('Ctrl Pts',(9.842233083162,-0.165735336637852,4.59309247934331));
#53908=CARTESIAN_POINT('Ctrl Pts',(9.82884541125756,0.000474857175501747,
4.59454166667424));
#53909=CARTESIAN_POINT('Ctrl Pts',(9.7211545887425,-0.000338423355870402,
4.59484023865297));
#53910=CARTESIAN_POINT('Ctrl Pts',(9.72273650167518,-0.0199523965301825,
4.59497351934566));
#53911=CARTESIAN_POINT('Ctrl Pts',(9.72431841460787,-0.0395541838993478,
4.59408780127083));
#53912=CARTESIAN_POINT('Ctrl Pts',(9.72590032754056,-0.0590504136254521,
4.592143576127));
#53913=CARTESIAN_POINT('Ctrl Pts',(9.74180560622817,-0.255074455621757,
4.57259544417541));
#53914=CARTESIAN_POINT('Ctrl Pts',(9.75771088491579,-0.4404274490251,4.4460405617726));
#53915=CARTESIAN_POINT('Ctrl Pts',(9.7736161636034,-0.530003140903138,4.2705875768224));
#53916=CARTESIAN_POINT('Ctrl Pts',(9.78952144229101,-0.619578832781174,
4.0951345918722));
#53917=CARTESIAN_POINT('Ctrl Pts',(9.80542672097862,-0.61337722313391,3.87078350437461));
#53918=CARTESIAN_POINT('Ctrl Pts',(9.82133199966623,-0.514245828742901,
3.70054684219675));
#53919=CARTESIAN_POINT('Ctrl Pts',(9.83723727835384,-0.41511443435189,3.53031018001889));
#53920=CARTESIAN_POINT('Ctrl Pts',(9.85314255704146,-0.223053255217129,
3.41418794316076));
#53921=CARTESIAN_POINT('Ctrl Pts',(9.86904783572907,-0.0262486593588972,
3.40549855006092));
#53922=CARTESIAN_POINT('Ctrl Pts',(9.88495311441669,0.170555936499329,3.39680915696108));
#53923=CARTESIAN_POINT('Ctrl Pts',(9.9008583931043,0.372103949081026,3.49555260761951));
#53924=CARTESIAN_POINT('Ctrl Pts',(9.91676367179191,0.485853057801912,3.65639008698476));
#53925=CARTESIAN_POINT('Ctrl Pts',(9.93266895047952,0.5996021665228,3.81722756635002));
#53926=CARTESIAN_POINT('Ctrl Pts',(9.94857422916713,0.625552371382872,4.04015907442209));
#53927=CARTESIAN_POINT('Ctrl Pts',(9.96447950785475,0.551788436173011,4.22282389414861));
#53928=CARTESIAN_POINT('Ctrl Pts',(9.98038478654236,0.478024500963153,4.40548871387512));
#53929=CARTESIAN_POINT('Ctrl Pts',(9.99629006522997,0.304546425683368,4.54788684525607));
#53930=CARTESIAN_POINT('Ctrl Pts',(10.0121953439176,0.111008003250015,4.58463509072946));
#53931=CARTESIAN_POINT('Ctrl Pts',(10.0151817588592,0.0746687445744621,
4.59153503329043));
#53932=CARTESIAN_POINT('Ctrl Pts',(10.0181681738009,0.0376222632219309,
4.59471031472953));
#53933=CARTESIAN_POINT('Ctrl Pts',(10.0211545887425,0.000517772199431355,
4.59437035498519));
#53934=CARTESIAN_POINT('Origin',(4.,0.,4.));
#53935=CARTESIAN_POINT('',(10.4288454112576,-0.000541293539476018,4.59389423388278));
#53936=CARTESIAN_POINT('',(10.3211545887425,8.19078234495683E-5,4.59312629593825));
#53937=CARTESIAN_POINT('',(4.,-7.27562663373442E-17,4.5941));
#53938=CARTESIAN_POINT('Ctrl Pts',(10.4288454112576,-0.000541293539476018,
4.59389423388278));
#53939=CARTESIAN_POINT('Ctrl Pts',(10.4171911487257,0.144553461780974,4.59260897165526));
#53940=CARTESIAN_POINT('Ctrl Pts',(10.4055368861939,0.290497422953868,4.53904330389552));
#53941=CARTESIAN_POINT('Ctrl Pts',(10.3938826236621,0.397841883685798,4.4425412994096));
#53942=CARTESIAN_POINT('Ctrl Pts',(10.3779773449745,0.544341377656434,4.31083916286766));
#53943=CARTESIAN_POINT('Ctrl Pts',(10.3620720662869,0.618946539098701,4.09916502578488));
#53944=CARTESIAN_POINT('Ctrl Pts',(10.3461667875993,0.587401834162399,3.90471069671543));
#53945=CARTESIAN_POINT('Ctrl Pts',(10.3302615089117,0.555857129226098,3.710256367646));
#53946=CARTESIAN_POINT('Ctrl Pts',(10.314356230224,0.418162557911234,3.5330218465899));
#53947=CARTESIAN_POINT('Ctrl Pts',(10.2984509515364,0.237541641988682,3.45438572744188));
#53948=CARTESIAN_POINT('Ctrl Pts',(10.2825456728488,0.0569207260661262,
3.37574960829385));
#53949=CARTESIAN_POINT('Ctrl Pts',(10.2666403941612,-0.16662653446412,3.3957118910539));
#53950=CARTESIAN_POINT('Ctrl Pts',(10.2507351154736,-0.330456695071223,
3.50510674001315));
#53951=CARTESIAN_POINT('Ctrl Pts',(10.234829836786,-0.494286855678321,3.61450158897239));
#53952=CARTESIAN_POINT('Ctrl Pts',(10.2189245580984,-0.59839991636228,3.81332900413083));
#53953=CARTESIAN_POINT('Ctrl Pts',(10.2030192794108,-0.594991564317383,
4.01029584814195));
#53954=CARTESIAN_POINT('Ctrl Pts',(10.1871140007231,-0.591583212272486,
4.20726269215308));
#53955=CARTESIAN_POINT('Ctrl Pts',(10.1712087220355,-0.480653447498727,
4.40236896501689));
#53956=CARTESIAN_POINT('Ctrl Pts',(10.1553034433479,-0.313136524928893,
4.50603012050002));
#53957=CARTESIAN_POINT('Ctrl Pts',(10.1464840993178,-0.220249792163878,
4.56350936438632));
#53958=CARTESIAN_POINT('Ctrl Pts',(10.1376647552877,-0.109964716607974,
4.59287280319057));
#53959=CARTESIAN_POINT('Ctrl Pts',(10.1288454112576,0.000175993811045716,
4.59316417414361));
#53960=CARTESIAN_POINT('Ctrl Pts',(10.0211545887425,0.000517772199431355,
4.59437035498519));
#53961=CARTESIAN_POINT('Ctrl Pts',(10.0340734524885,-0.159991692577292,
4.59289973094197));
#53962=CARTESIAN_POINT('Ctrl Pts',(10.0469923162344,-0.321586704601994,
4.52564765365589));
#53963=CARTESIAN_POINT('Ctrl Pts',(10.0599111799804,-0.431712787135162,
4.40956688772629));
#53964=CARTESIAN_POINT('Ctrl Pts',(10.075816458668,-0.567296385500051,4.2666520796839));
#53965=CARTESIAN_POINT('Ctrl Pts',(10.0917217373556,-0.624864812642908,
4.04972410403331));
#53966=CARTESIAN_POINT('Ctrl Pts',(10.1076270160433,-0.577985082339038,
3.85838710972745));
#53967=CARTESIAN_POINT('Ctrl Pts',(10.1235322947309,-0.531105352035168,
3.6670501154216));
#53968=CARTESIAN_POINT('Ctrl Pts',(10.1394375734185,-0.379777464284567,
3.50130410246047));
#53969=CARTESIAN_POINT('Ctrl Pts',(10.1553428521061,-0.193484782987353,
3.43725262786029));
#53970=CARTESIAN_POINT('Ctrl Pts',(10.1712481307937,-0.00719210169012799,
3.37320115326011));
#53971=CARTESIAN_POINT('Ctrl Pts',(10.1871534094813,0.214065373153706,3.41084421702088));
#53972=CARTESIAN_POINT('Ctrl Pts',(10.2030586881689,0.368695569727689,3.53289771681035));
#53973=CARTESIAN_POINT('Ctrl Pts',(10.2189639668565,0.523325766301663,3.65495121659981));
#53974=CARTESIAN_POINT('Ctrl Pts',(10.2348692455442,0.611328684605784,3.86141515241798));
#53975=CARTESIAN_POINT('Ctrl Pts',(10.2507745242318,0.592297107651237,4.05749001970593));
#53976=CARTESIAN_POINT('Ctrl Pts',(10.2666798029194,0.573265530696689,4.25356488699388));
#53977=CARTESIAN_POINT('Ctrl Pts',(10.282585081607,0.447199458483466,4.43925068575162));
#53978=CARTESIAN_POINT('Ctrl Pts',(10.2984903602946,0.271983097956201,4.5292883529079));
#53979=CARTESIAN_POINT('Ctrl Pts',(10.3060451031106,0.188758241169316,4.57205474716445));
#53980=CARTESIAN_POINT('Ctrl Pts',(10.3135998459265,0.0944446272328244,
4.59324204311815));
#53981=CARTESIAN_POINT('Ctrl Pts',(10.3211545887425,8.19078234495684E-5,
4.59312629593825));
#53982=CARTESIAN_POINT('Origin',(4.,0.,4.));
#53983=CARTESIAN_POINT('',(10.7288454112576,7.37317986114466E-5,4.59506942345298));
#53984=CARTESIAN_POINT('',(10.6211545887425,-0.000548317120500629,4.59406879148573));
#53985=CARTESIAN_POINT('',(4.,-7.27562663373442E-17,4.5941));
#53986=CARTESIAN_POINT('Ctrl Pts',(10.7288454112576,7.37317986114466E-5,
4.59506942345298));
#53987=CARTESIAN_POINT('Ctrl Pts',(10.728528099539,0.00400402563557926,
4.59507627971693));
#53988=CARTESIAN_POINT('Ctrl Pts',(10.7282107878205,0.00793419209028873,
4.59504072157671));
#53989=CARTESIAN_POINT('Ctrl Pts',(10.727893476102,0.0118635052742893,4.59496237136513));
#53990=CARTESIAN_POINT('Ctrl Pts',(10.7119881974144,0.208820685209451,4.59103505989901));
#53991=CARTESIAN_POINT('Ctrl Pts',(10.6960829187267,0.403634001393415,4.47959161118634));
#53992=CARTESIAN_POINT('Ctrl Pts',(10.6801776400391,0.506853420906232,4.31180214209248));
#53993=CARTESIAN_POINT('Ctrl Pts',(10.6642723613515,0.610072840419052,4.14401267299861));
#53994=CARTESIAN_POINT('Ctrl Pts',(10.6483670826639,0.621698363260717,3.91987718352354));
#53995=CARTESIAN_POINT('Ctrl Pts',(10.6324618039763,0.536392041177647,3.74230920804366));
#53996=CARTESIAN_POINT('Ctrl Pts',(10.6165565252887,0.451085719094577,3.56474123256377));
#53997=CARTESIAN_POINT('Ctrl Pts',(10.6006512466011,0.26884755208677,3.43374077107907));
#53998=CARTESIAN_POINT('Ctrl Pts',(10.5847459679135,0.0733535965831807,
3.40945769333085));
#53999=CARTESIAN_POINT('Ctrl Pts',(10.5688406892258,-0.122140358920403,
3.38517461558263));
#54000=CARTESIAN_POINT('Ctrl Pts',(10.5529354105382,-0.33089010291977,3.46760892157089));
#54001=CARTESIAN_POINT('Ctrl Pts',(10.5370301318506,-0.457046584443773,
3.61891026549369));
#54002=CARTESIAN_POINT('Ctrl Pts',(10.521124853163,-0.583203065967777,3.7702116094165));
#54003=CARTESIAN_POINT('Ctrl Pts',(10.5052195744754,-0.626766285016417,
3.99037999127385));
#54004=CARTESIAN_POINT('Ctrl Pts',(10.4893142957878,-0.567733854410369,
4.17832340467295));
#54005=CARTESIAN_POINT('Ctrl Pts',(10.4734090171002,-0.508701423804317,
4.36626681807206));
#54006=CARTESIAN_POINT('Ctrl Pts',(10.4575037384126,-0.347073343543565,
4.52198526301292));
#54007=CARTESIAN_POINT('Ctrl Pts',(10.4415984597249,-0.157062390163684,
4.57397941748279));
#54008=CARTESIAN_POINT('Ctrl Pts',(10.4373474435692,-0.106278015462724,
4.58787593542499));
#54009=CARTESIAN_POINT('Ctrl Pts',(10.4330964274134,-0.0534661480554494,
4.59436304694399));
#54010=CARTESIAN_POINT('Ctrl Pts',(10.4288454112576,-0.000541293539476018,
4.59389423388278));
#54011=CARTESIAN_POINT('Ctrl Pts',(10.3211545887425,8.19078234495684E-5,
4.59312629593825));
#54012=CARTESIAN_POINT('Ctrl Pts',(10.3295051246142,-0.104220686264852,
4.59299835631127));
#54013=CARTESIAN_POINT('Ctrl Pts',(10.3378556604858,-0.208583275928277,
4.56684300569277));
#54014=CARTESIAN_POINT('Ctrl Pts',(10.3462061963575,-0.298097175589899,
4.5150330474864));
#54015=CARTESIAN_POINT('Ctrl Pts',(10.3621114750451,-0.468594439767441,
4.41635053935381));
#54016=CARTESIAN_POINT('Ctrl Pts',(10.3780167537327,-0.585222319281217,
4.22459598753381));
#54017=CARTESIAN_POINT('Ctrl Pts',(10.3939220324203,-0.594430225977177,
4.02781496975607));
#54018=CARTESIAN_POINT('Ctrl Pts',(10.4098273111079,-0.603638132673137,
3.83103395197833));
#54019=CARTESIAN_POINT('Ctrl Pts',(10.4257325897955,-0.505426066551287,
3.62922646824286));
#54020=CARTESIAN_POINT('Ctrl Pts',(10.4416378684831,-0.344888853364916,
3.51505397731042));
#54021=CARTESIAN_POINT('Ctrl Pts',(10.4575431471707,-0.184351640178541,
3.40088148637798));
#54022=CARTESIAN_POINT('Ctrl Pts',(10.4734484258584,0.0385107200723601,
3.37434398824859));
#54023=CARTESIAN_POINT('Ctrl Pts',(10.489353704546,0.221369260089487,3.4476263793543));
#54024=CARTESIAN_POINT('Ctrl Pts',(10.5052589832336,0.40422780010661,3.52090877046001));
#54025=CARTESIAN_POINT('Ctrl Pts',(10.5211642619212,0.54708251988996,3.69401105080081));
#54026=CARTESIAN_POINT('Ctrl Pts',(10.5370695406088,0.584340575799814,3.88745197659776));
#54027=CARTESIAN_POINT('Ctrl Pts',(10.5529748192964,0.621598631709669,4.08089290239472));
#54028=CARTESIAN_POINT('Ctrl Pts',(10.568880097984,0.55326002374602,4.29467247364782));
#54029=CARTESIAN_POINT('Ctrl Pts',(10.5847853766716,0.4107029495177,4.43063215550545));
#54030=CARTESIAN_POINT('Ctrl Pts',(10.5969084473619,0.302045344566967,4.53426120008624));
#54031=CARTESIAN_POINT('Ctrl Pts',(10.6090315180522,0.150270129189204,4.59268036842864));
#54032=CARTESIAN_POINT('Ctrl Pts',(10.6211545887425,-0.000548317120500629,
4.59406879148573));
#54033=CARTESIAN_POINT('Origin',(4.,0.,4.));
#54034=CARTESIAN_POINT('',(11.0288454112576,0.000503618959454472,4.59367252935801));
#54035=CARTESIAN_POINT('',(10.9211545887425,0.000179316795020235,4.59501533910171));
#54036=CARTESIAN_POINT('',(4.,-7.27562663373442E-17,4.5941));
#54037=CARTESIAN_POINT('Ctrl Pts',(11.0288454112576,0.000503618959454472,
4.59367252935801));
#54038=CARTESIAN_POINT('Ctrl Pts',(11.0239597716647,0.0613870506829751,
4.59415995979602));
#54039=CARTESIAN_POINT('Ctrl Pts',(11.0190741320719,0.122135879976345,4.58554712933309));
#54040=CARTESIAN_POINT('Ctrl Pts',(11.014188492479,0.179818659528701,4.56726203449827));
#54041=CARTESIAN_POINT('Ctrl Pts',(10.9982832137914,0.36760588100072,4.50773461262244));
#54042=CARTESIAN_POINT('Ctrl Pts',(10.9823779351038,0.52289792528528,4.34569680405454));
#54043=CARTESIAN_POINT('Ctrl Pts',(10.9664726564162,0.574391255511512,4.15554951523459));
#54044=CARTESIAN_POINT('Ctrl Pts',(10.9505673777285,0.625884585737745,3.96540222641464));
#54045=CARTESIAN_POINT('Ctrl Pts',(10.9346620990409,0.573579201905647,3.74714545734266));
#54046=CARTESIAN_POINT('Ctrl Pts',(10.9187568203533,0.441491523412615,3.60099348269406));
#54047=CARTESIAN_POINT('Ctrl Pts',(10.9028515416657,0.309403844919578,3.45484150804546));
#54048=CARTESIAN_POINT('Ctrl Pts',(10.8869462629781,0.0975338717655902,
3.38079432782024));
#54049=CARTESIAN_POINT('Ctrl Pts',(10.8710409842905,-0.0968366678563846,
3.41285127449999));
#54050=CARTESIAN_POINT('Ctrl Pts',(10.8551357056029,-0.291207207478354,
3.44490822117975));
#54051=CARTESIAN_POINT('Ctrl Pts',(10.8392304269153,-0.468078313568319,
3.58306929476445));
#54052=CARTESIAN_POINT('Ctrl Pts',(10.8233251482276,-0.546238257009186,
3.76389677537701));
#54053=CARTESIAN_POINT('Ctrl Pts',(10.80741986954,-0.624398200450053,3.94472425598957));
#54054=CARTESIAN_POINT('Ctrl Pts',(10.7915145908524,-0.603846981241821,
4.16821814362997));
#54055=CARTESIAN_POINT('Ctrl Pts',(10.7756093121648,-0.494020849794526,
4.33175950034039));
#54056=CARTESIAN_POINT('Ctrl Pts',(10.7600213451957,-0.386385759396791,
4.49203819249975));
#54057=CARTESIAN_POINT('Ctrl Pts',(10.7444333782267,-0.193002309618558,
4.59473260886404));
#54058=CARTESIAN_POINT('Ctrl Pts',(10.7288454112576,7.37317986114466E-5,
4.59506942345298));
#54059=CARTESIAN_POINT('Ctrl Pts',(10.6211545887425,-0.000548317120500629,
4.59406879148573));
#54060=CARTESIAN_POINT('Ctrl Pts',(10.6249367967398,-0.0476013079303647,
4.5945019577127));
#54061=CARTESIAN_POINT('Ctrl Pts',(10.6287190047372,-0.0945611723716044,
4.58938408097059));
#54062=CARTESIAN_POINT('Ctrl Pts',(10.6325012127345,-0.140089514783682,
4.57835619988505));
#54063=CARTESIAN_POINT('Ctrl Pts',(10.6484064914221,-0.331549364363767,
4.53198076994489));
#54064=CARTESIAN_POINT('Ctrl Pts',(10.6643117701097,-0.497693523030948,
4.38109011760241));
#54065=CARTESIAN_POINT('Ctrl Pts',(10.6802170487973,-0.562235622104956,
4.19496684675621));
#54066=CARTESIAN_POINT('Ctrl Pts',(10.6961223274849,-0.626777721178965,
4.00884357591002));
#54067=CARTESIAN_POINT('Ctrl Pts',(10.7120276061725,-0.589717760659791,
3.78748768656011));
#54068=CARTESIAN_POINT('Ctrl Pts',(10.7279328848602,-0.468072106540212,
3.63253643830059));
#54069=CARTESIAN_POINT('Ctrl Pts',(10.7438381635478,-0.346426452420629,
3.47758519004106));
#54070=CARTESIAN_POINT('Ctrl Pts',(10.7597434422354,-0.140195104700642,
3.38903858287192));
#54071=CARTESIAN_POINT('Ctrl Pts',(10.775648720923,0.0559292266755373,3.40755347270721));
#54072=CARTESIAN_POINT('Ctrl Pts',(10.7915539996106,0.252053558051711,3.4260683625425));
#54073=CARTESIAN_POINT('Ctrl Pts',(10.8074592782982,0.438070873084069,3.55164474938222));
#54074=CARTESIAN_POINT('Ctrl Pts',(10.8233645569858,0.528569890453362,3.72662326908837));
#54075=CARTESIAN_POINT('Ctrl Pts',(10.8392698356734,0.619068907822657,3.90160178879453));
#54076=CARTESIAN_POINT('Ctrl Pts',(10.8551751143611,0.614049627528876,4.12598244136713));
#54077=CARTESIAN_POINT('Ctrl Pts',(10.8710803930487,0.515816690734684,4.29673912390739));
#54078=CARTESIAN_POINT('Ctrl Pts',(10.8869856717363,0.417583753940498,4.46749580644764));
#54079=CARTESIAN_POINT('Ctrl Pts',(10.9028909504239,0.226137160645921,4.58462851895556));
#54080=CARTESIAN_POINT('Ctrl Pts',(10.9187962291115,0.0293810870543861,
4.59435487532392));
#54081=CARTESIAN_POINT('Ctrl Pts',(10.9195823489885,0.0196563998352688,
4.59483560139116));
#54082=CARTESIAN_POINT('Ctrl Pts',(10.9203684688655,0.00991874240631306,
4.5950539509358));
#54083=CARTESIAN_POINT('Ctrl Pts',(10.9211545887425,0.000179316795020235,
4.59501533910171));
#54084=CARTESIAN_POINT('Origin',(4.,0.,4.));
#54085=CARTESIAN_POINT('',(11.3288454112576,-0.000294350894641693,4.59325842069974));
#54086=CARTESIAN_POINT('',(11.2211545887425,0.000456638431143918,4.59352536526061));
#54087=CARTESIAN_POINT('',(4.,-7.27562663373442E-17,4.5941));
#54088=CARTESIAN_POINT('Ctrl Pts',(11.3288454112576,-0.000294350894641693,
4.59325842069974));
#54089=CARTESIAN_POINT('Ctrl Pts',(11.3193914437904,0.117725031793324,4.59273125875086));
#54090=CARTESIAN_POINT('Ctrl Pts',(11.3099374763232,0.236024696118704,4.55868066117597));
#54091=CARTESIAN_POINT('Ctrl Pts',(11.300483508856,0.333060002447629,4.49314500997921));
#54092=CARTESIAN_POINT('Ctrl Pts',(11.2845782301684,0.496311419914153,4.38288835848583));
#54093=CARTESIAN_POINT('Ctrl Pts',(11.2686729514808,0.599375291650127,4.18351506848348));
#54094=CARTESIAN_POINT('Ctrl Pts',(11.2527676727932,0.594929048027223,3.98656891995295));
#54095=CARTESIAN_POINT('Ctrl Pts',(11.2368623941056,0.59048280440432,3.78962277142242));
#54096=CARTESIAN_POINT('Ctrl Pts',(11.220957115418,0.478526445422532,3.5951037643637));
#54097=CARTESIAN_POINT('Ctrl Pts',(11.2050518367303,0.310465594643358,3.49232679739763));
#54098=CARTESIAN_POINT('Ctrl Pts',(11.1891465580427,0.142404743864184,3.38954983043155));
#54099=CARTESIAN_POINT('Ctrl Pts',(11.1732412793551,-0.0817605987123653,
3.37851490355812));
#54100=CARTESIAN_POINT('Ctrl Pts',(11.1573360006675,-0.259103191428711,
3.46428878834836));
#54101=CARTESIAN_POINT('Ctrl Pts',(11.1414307219799,-0.436445784145052,
3.5500626731386));
#54102=CARTESIAN_POINT('Ctrl Pts',(11.1255254432923,-0.566965627001181,
3.73264536959251));
#54103=CARTESIAN_POINT('Ctrl Pts',(11.1096201646047,-0.590733529996744,
3.92820262793532));
#54104=CARTESIAN_POINT('Ctrl Pts',(11.0937148859171,-0.614501432992307,
4.12375988627813));
#54105=CARTESIAN_POINT('Ctrl Pts',(11.0778096072294,-0.531517396127296,
4.33229170650985));
#54106=CARTESIAN_POINT('Ctrl Pts',(11.0619043285418,-0.379884178365051,
4.45804909903384));
#54107=CARTESIAN_POINT('Ctrl Pts',(11.0508846894471,-0.274828280424841,
4.54517747360242));
#54108=CARTESIAN_POINT('Ctrl Pts',(11.0398650503523,-0.136819945681758,
4.59257312212411));
#54109=CARTESIAN_POINT('Ctrl Pts',(11.0288454112576,0.000503618959454472,
4.59367252935801));
#54110=CARTESIAN_POINT('Ctrl Pts',(10.9211545887425,0.000179316795020235,
4.59501533910171));
#54111=CARTESIAN_POINT('Ctrl Pts',(10.9362737475531,-0.187135527734918,
4.59427273168419));
#54112=CARTESIAN_POINT('Ctrl Pts',(10.9513929063637,-0.375104412928531,
4.49848156101044));
#54113=CARTESIAN_POINT('Ctrl Pts',(10.9665120651743,-0.484035620954107,
4.34616539940523));
#54114=CARTESIAN_POINT('Ctrl Pts',(10.982417343862,-0.598630701482551,4.1859295668894));
#54115=CARTESIAN_POINT('Ctrl Pts',(10.9983226225496,-0.625755308650954,
3.96313790162893));
#54116=CARTESIAN_POINT('Ctrl Pts',(11.0142279012372,-0.55295497039508,3.7800869107734));
#54117=CARTESIAN_POINT('Ctrl Pts',(11.0301331799248,-0.480154632139201,
3.59703591991786));
#54118=CARTESIAN_POINT('Ctrl Pts',(11.0460384586124,-0.307429348459053,
3.45372560346725));
#54119=CARTESIAN_POINT('Ctrl Pts',(11.0619437373,-0.114087262216405,3.41595799577618));
#54120=CARTESIAN_POINT('Ctrl Pts',(11.0778490159876,0.0792548240262376,
3.37819038808511));
#54121=CARTESIAN_POINT('Ctrl Pts',(11.0937542946752,0.293213712831377,3.4459654891536));
#54122=CARTESIAN_POINT('Ctrl Pts',(11.1096595733629,0.429548534313776,3.58816383989905));
#54123=CARTESIAN_POINT('Ctrl Pts',(11.1255648520505,0.565883355796175,3.7303621906445));
#54124=CARTESIAN_POINT('Ctrl Pts',(11.1414701307381,0.624594109955846,3.94698379106692));
#54125=CARTESIAN_POINT('Ctrl Pts',(11.1573754094257,0.578723302329844,4.13856516675647));
#54126=CARTESIAN_POINT('Ctrl Pts',(11.1732806881133,0.53285249470384,4.33014654244603));
#54127=CARTESIAN_POINT('Ctrl Pts',(11.1891859668009,0.382400125292158,4.49668769340272));
#54128=CARTESIAN_POINT('Ctrl Pts',(11.2050912454885,0.196447557013804,4.56171996888228));
#54129=CARTESIAN_POINT('Ctrl Pts',(11.2104456932399,0.133847376870746,4.58361282144047));
#54130=CARTESIAN_POINT('Ctrl Pts',(11.2158001409912,0.0672239414478651,
4.5940016224088));
#54131=CARTESIAN_POINT('Ctrl Pts',(11.2211545887425,0.000456638431143918,
4.59352536526061));
#54132=CARTESIAN_POINT('Origin',(4.,0.,4.));
#54133=CARTESIAN_POINT('',(11.6288454112576,-0.000389145320547679,4.59475273347735));
#54134=CARTESIAN_POINT('',(11.5211545887425,-0.0003715675665865,4.59335763259963));
#54135=CARTESIAN_POINT('',(4.,-7.27562663373442E-17,4.5941));
#54136=CARTESIAN_POINT('Ctrl Pts',(11.6288454112576,-0.000389145320547679,
4.59475273347735));
#54137=CARTESIAN_POINT('Ctrl Pts',(11.6148231159161,0.173538999407471,4.59343557735163));
#54138=CARTESIAN_POINT('Ctrl Pts',(11.6008008205746,0.348531733704351,4.51264940831536));
#54139=CARTESIAN_POINT('Ctrl Pts',(11.586778525233,0.459048433726307,4.37867598496766));
#54140=CARTESIAN_POINT('Ctrl Pts',(11.5708732465454,0.584405864209301,4.22671194604376));
#54141=CARTESIAN_POINT('Ctrl Pts',(11.5549679678578,0.626808276394098,4.00631705984067));
#54142=CARTESIAN_POINT('Ctrl Pts',(11.5390626891702,0.566786276503563,3.81868733396413));
#54143=CARTESIAN_POINT('Ctrl Pts',(11.5231574104826,0.506764276613028,3.6310576080876));
#54144=CARTESIAN_POINT('Ctrl Pts',(11.507252131795,0.344317864647159,3.47619304253762));
#54145=CARTESIAN_POINT('Ctrl Pts',(11.4913468531074,0.154035560439752,3.4252008940353));
#54146=CARTESIAN_POINT('Ctrl Pts',(11.4754415744198,-0.0362467437676612,
3.37420874553297));
#54147=CARTESIAN_POINT('Ctrl Pts',(11.4595362957322,-0.254364940216614,
3.4270890140783));
#54148=CARTESIAN_POINT('Ctrl Pts',(11.4436310170445,-0.400168380917644,
3.55956131753494));
#54149=CARTESIAN_POINT('Ctrl Pts',(11.4277257383569,-0.545971821618673,
3.69203362099157));
#54150=CARTESIAN_POINT('Ctrl Pts',(11.4118204596693,-0.619460506571779,
3.90409795935952));
#54151=CARTESIAN_POINT('Ctrl Pts',(11.3959151809817,-0.586891540696359,
4.09838336016249));
#54152=CARTESIAN_POINT('Ctrl Pts',(11.3800099022941,-0.554322574820941,
4.29266876096545));
#54153=CARTESIAN_POINT('Ctrl Pts',(11.3641046236065,-0.415695958117004,
4.46917522420345));
#54154=CARTESIAN_POINT('Ctrl Pts',(11.3481993449189,-0.234663168166497,
4.54685844933023));
#54155=CARTESIAN_POINT('Ctrl Pts',(11.3417480336984,-0.161234786808821,
4.57836740127901));
#54156=CARTESIAN_POINT('Ctrl Pts',(11.335296722478,-0.080829826651965,4.59361815176584));
#54157=CARTESIAN_POINT('Ctrl Pts',(11.3288454112576,-0.000294350894641693,
4.59325842069974));
#54158=CARTESIAN_POINT('Ctrl Pts',(11.2211545887425,0.000456638431143918,
4.59352536526061));
#54159=CARTESIAN_POINT('Ctrl Pts',(11.2317054196788,-0.131106980996848,
4.59258691018808));
#54160=CARTESIAN_POINT('Ctrl Pts',(11.2422562506151,-0.263229208150973,
4.54946171071576));
#54161=CARTESIAN_POINT('Ctrl Pts',(11.2528070815514,-0.366229002642205,
4.4690386804108));
#54162=CARTESIAN_POINT('Ctrl Pts',(11.268712360239,-0.521500226874852,4.34780171645731));
#54163=CARTESIAN_POINT('Ctrl Pts',(11.2846176389266,-0.610589908195122,
4.1418043885479));
#54164=CARTESIAN_POINT('Ctrl Pts',(11.3005229176142,-0.592591834014348,
3.94563195463032));
#54165=CARTESIAN_POINT('Ctrl Pts',(11.3164281963018,-0.574593759833574,
3.74945952071274));
#54166=CARTESIAN_POINT('Ctrl Pts',(11.3323334749894,-0.449507930151742,
3.56311198078699));
#54167=CARTESIAN_POINT('Ctrl Pts',(11.3482387536771,-0.274768466013715,
3.47215224147272));
#54168=CARTESIAN_POINT('Ctrl Pts',(11.3641440323647,-0.100029001875688,
3.38119250215845));
#54169=CARTESIAN_POINT('Ctrl Pts',(11.3800493110523,0.12436409671854,3.38562056345565));
#54170=CARTESIAN_POINT('Ctrl Pts',(11.3959545897399,0.295379012183608,3.48340324695247));
#54171=CARTESIAN_POINT('Ctrl Pts',(11.4118598684275,0.466393927648671,3.5811859304493));
#54172=CARTESIAN_POINT('Ctrl Pts',(11.4277651471151,0.584030659984583,3.77232323614575));
#54173=CARTESIAN_POINT('Ctrl Pts',(11.4436704258027,0.594275398502411,3.96905299961855));
#54174=CARTESIAN_POINT('Ctrl Pts',(11.4595757044903,0.60452013702024,4.16578276309136));
#54175=CARTESIAN_POINT('Ctrl Pts',(11.475480983178,0.507372881719984,4.36810498434052));
#54176=CARTESIAN_POINT('Ctrl Pts',(11.4913862618656,0.34743954227408,4.48312185891572));
#54177=CARTESIAN_POINT('Ctrl Pts',(11.5013090374912,0.247662438486696,4.55487707062799));
#54178=CARTESIAN_POINT('Ctrl Pts',(11.5112318131169,0.123448374926332,4.59265218509947));
#54179=CARTESIAN_POINT('Ctrl Pts',(11.5211545887425,-0.0003715675665865,
4.59335763259963));
#54180=CARTESIAN_POINT('Origin',(4.,0.,4.));
#54181=CARTESIAN_POINT('',(11.9288454112576,0.000492284285450728,4.5944814532616));
#54182=CARTESIAN_POINT('',(11.8211545887425,-0.000307672146732893,4.59488449882539));
#54183=CARTESIAN_POINT('',(4.,-7.27562663373442E-17,4.5941));
#54184=CARTESIAN_POINT('Ctrl Pts',(11.9288454112576,0.000492284285450728,
4.5944814532616));
#54185=CARTESIAN_POINT('Ctrl Pts',(11.9261600667293,0.0338400408399785,
4.59477876231094));
#54186=CARTESIAN_POINT('Ctrl Pts',(11.9234747222011,0.0671420792079604,
4.59221542322669));
#54187=CARTESIAN_POINT('Ctrl Pts',(11.9207893776729,0.0999293694653808,
4.5866302815369));
#54188=CARTESIAN_POINT('Ctrl Pts',(11.9048840989853,0.294128282668868,4.55354952256816));
#54189=CARTESIAN_POINT('Ctrl Pts',(11.8889788202977,0.470268877700486,4.41445832512751));
#54190=CARTESIAN_POINT('Ctrl Pts',(11.8730735416101,0.547474845215755,4.2332214826164));
#54191=CARTESIAN_POINT('Ctrl Pts',(11.8571682629225,0.624680812731027,4.05198464010529));
#54192=CARTESIAN_POINT('Ctrl Pts',(11.8412629842349,0.602952152729945,3.82860215252373));
#54193=CARTESIAN_POINT('Ctrl Pts',(11.8253577055472,0.492265746621211,3.66564180763548));
#54194=CARTESIAN_POINT('Ctrl Pts',(11.8094524268596,0.38157934051248,3.50268146274723));
#54195=CARTESIAN_POINT('Ctrl Pts',(11.793547148172,0.181935188296101,3.40014326055229));
#54196=CARTESIAN_POINT('Ctrl Pts',(11.7776418694844,-0.0149985615777061,
3.40510840546499));
#54197=CARTESIAN_POINT('Ctrl Pts',(11.7617365907968,-0.211932311451519,
3.41007355037768));
#54198=CARTESIAN_POINT('Ctrl Pts',(11.7458313121092,-0.406155658982761,
3.52254204239802));
#54199=CARTESIAN_POINT('Ctrl Pts',(11.7299260334216,-0.508489459897291,
3.69087310813977));
#54200=CARTESIAN_POINT('Ctrl Pts',(11.714020754734,-0.610823260811815,3.8592041738815));
#54201=CARTESIAN_POINT('Ctrl Pts',(11.6981154760463,-0.621267515109637,
4.08339781334463));
#54202=CARTESIAN_POINT('Ctrl Pts',(11.6822101973587,-0.53502666307716,4.26051379213839));
#54203=CARTESIAN_POINT('Ctrl Pts',(11.6663049186711,-0.448785811044678,
4.43762977093217));
#54204=CARTESIAN_POINT('Ctrl Pts',(11.6503996399835,-0.265859852681883,
4.56766808905658));
#54205=CARTESIAN_POINT('Ctrl Pts',(11.6344943612959,-0.070240649109886,
4.59092065229643));
#54206=CARTESIAN_POINT('Ctrl Pts',(11.6326113779498,-0.0470818155087989,
4.59367346098309));
#54207=CARTESIAN_POINT('Ctrl Pts',(11.6307283946037,-0.0237450789937817,
4.59492960773286));
#54208=CARTESIAN_POINT('Ctrl Pts',(11.6288454112576,-0.000389145320547679,
4.59475273347735));
#54209=CARTESIAN_POINT('Ctrl Pts',(11.5211545887425,-0.0003715675665865,
4.59335763259963));
#54210=CARTESIAN_POINT('Ctrl Pts',(11.5271370918045,-0.0750233800274846,
4.5937829512795));
#54211=CARTESIAN_POINT('Ctrl Pts',(11.5331195948664,-0.149531931096223,
4.58073359799715));
#54212=CARTESIAN_POINT('Ctrl Pts',(11.5391020979284,-0.218455391669058,
4.55353248138526));
#54213=CARTESIAN_POINT('Ctrl Pts',(11.555007376616,-0.40169756257477,4.48121470137836));
#54214=CARTESIAN_POINT('Ctrl Pts',(11.5709126553036,-0.545462480794654,
4.3088676134633));
#54215=CARTESIAN_POINT('Ctrl Pts',(11.5868179339912,-0.583739378074245,
4.1156257090067));
#54216=CARTESIAN_POINT('Ctrl Pts',(11.6027232126789,-0.622016275353834,
3.92238380455011));
#54217=CARTESIAN_POINT('Ctrl Pts',(11.6186284913665,-0.554805151693135,
3.70824708355197));
#54218=CARTESIAN_POINT('Ctrl Pts',(11.6345337700541,-0.412966511608993,
3.57153806891708));
#54219=CARTESIAN_POINT('Ctrl Pts',(11.6504390487417,-0.271127871524847,
3.43482905428217));
#54220=CARTESIAN_POINT('Ctrl Pts',(11.6663443274293,-0.0546617150172531,
3.37554774601052));
#54221=CARTESIAN_POINT('Ctrl Pts',(11.6822496061169,0.137039856773353,3.42091361287512));
#54222=CARTESIAN_POINT('Ctrl Pts',(11.6981548848045,0.328741428563947,3.46627947973972));
#54223=CARTESIAN_POINT('Ctrl Pts',(11.7140601634921,0.495678415637556,3.61629252174057));
#54224=CARTESIAN_POINT('Ctrl Pts',(11.7299654421798,0.56120041605148,3.80207309651931));
#54225=CARTESIAN_POINT('Ctrl Pts',(11.7458707208674,0.626722416465409,3.98785367129807));
#54226=CARTESIAN_POINT('Ctrl Pts',(11.761775999555,0.590829430219633,4.20940177885472));
#54227=CARTESIAN_POINT('Ctrl Pts',(11.7776812782426,0.470001998091193,4.36499190112672));
#54228=CARTESIAN_POINT('Ctrl Pts',(11.7921723817426,0.359917612963646,4.5067481450567));
#54229=CARTESIAN_POINT('Ctrl Pts',(11.8066634852425,0.179330777996457,4.59375393408315));
#54230=CARTESIAN_POINT('Ctrl Pts',(11.8211545887425,-0.000307672146732893,
4.59488449882539));
#54231=CARTESIAN_POINT('Origin',(4.,0.,4.));
#54232=CARTESIAN_POINT('',(12.2288454112576,0.000142795628640946,4.59314744373127));
#54233=CARTESIAN_POINT('',(12.1211545887425,0.00052868291625318,4.59430727435519));
#54234=CARTESIAN_POINT('',(4.,-7.27562663373442E-17,4.5941));
#54235=CARTESIAN_POINT('Ctrl Pts',(12.2288454112576,0.000142795628640946,
4.59314744373127));
#54236=CARTESIAN_POINT('Ctrl Pts',(12.221591738855,0.0907369315914116,4.59334157666405));
#54237=CARTESIAN_POINT('Ctrl Pts',(12.2143380664525,0.181251971066953,4.57388161006077));
#54238=CARTESIAN_POINT('Ctrl Pts',(12.2070843940499,0.261922584292681,4.53433840020651));
#54239=CARTESIAN_POINT('Ctrl Pts',(12.1911791153623,0.438810719578057,4.44763117963851));
#54240=CARTESIAN_POINT('Ctrl Pts',(12.1752738366747,0.56836661021043,4.26436322928705));
#54241=CARTESIAN_POINT('Ctrl Pts',(12.1593685579871,0.591103672269137,4.06868343852597));
#54242=CARTESIAN_POINT('Ctrl Pts',(12.1434632792995,0.613840734327844,3.87300364776488));
#54243=CARTESIAN_POINT('Ctrl Pts',(12.1275580006119,0.529758967812885,3.66491201659415));
#54244=CARTESIAN_POINT('Ctrl Pts',(12.1116527219243,0.377465162701742,3.53995541841648));
#54245=CARTESIAN_POINT('Ctrl Pts',(12.0957474432367,0.225171357590603,3.41499882023882));
#54246=CARTESIAN_POINT('Ctrl Pts',(12.0798421645491,0.00466551388328543,
3.37317725505421));
#54247=CARTESIAN_POINT('Ctrl Pts',(12.0639368858614,-0.182805413822737,
3.43369341627091));
#54248=CARTESIAN_POINT('Ctrl Pts',(12.0480316071738,-0.37027634152876,3.49420957748762));
#54249=CARTESIAN_POINT('Ctrl Pts',(12.0321263284862,-0.524712353233489,
3.65706346510565));
#54250=CARTESIAN_POINT('Ctrl Pts',(12.0162210497986,-0.575202966010955,
3.84747946371059));
#54251=CARTESIAN_POINT('Ctrl Pts',(12.000315771111,-0.625693578788423,4.03789546231555));
#54252=CARTESIAN_POINT('Ctrl Pts',(11.9844104924234,-0.572238792638624,
4.25587357190742));
#54253=CARTESIAN_POINT('Ctrl Pts',(11.9685052137358,-0.439382783876041,
4.40132746645495));
#54254=CARTESIAN_POINT('Ctrl Pts',(11.9552852795764,-0.328957325572706,
4.52222386487166));
#54255=CARTESIAN_POINT('Ctrl Pts',(11.942065345417,-0.163678510702966,4.59301780268865));
#54256=CARTESIAN_POINT('Ctrl Pts',(11.9288454112576,0.000492284285450728,
4.5944814532616));
#54257=CARTESIAN_POINT('Ctrl Pts',(11.8211545887425,-0.000307672146732893,
4.59488449882539));
#54258=CARTESIAN_POINT('Ctrl Pts',(11.8225687639301,-0.0178384446610953,
4.59499482973335));
#54259=CARTESIAN_POINT('Ctrl Pts',(11.8239829391178,-0.035360185088601,
4.59428731490513));
#54260=CARTESIAN_POINT('Ctrl Pts',(11.8253971143054,-0.0528064866265509,
4.59273302680715));
#54261=CARTESIAN_POINT('Ctrl Pts',(11.8413023929931,-0.249025661204777,
4.57525189322826));
#54262=CARTESIAN_POINT('Ctrl Pts',(11.8572076716807,-0.435702132350142,
4.45065748908313));
#54263=CARTESIAN_POINT('Ctrl Pts',(11.8731129503683,-0.527121962142897,
4.27615829360067));
#54264=CARTESIAN_POINT('Ctrl Pts',(11.8890182290559,-0.618541791935657,
4.10165909811819));
#54265=CARTESIAN_POINT('Ctrl Pts',(11.9049235077435,-0.614704980375792,
3.87725511129838));
#54266=CARTESIAN_POINT('Ctrl Pts',(11.9208287864311,-0.517373229009482,
3.70598315013913));
#54267=CARTESIAN_POINT('Ctrl Pts',(11.9367340651187,-0.420041477643178,
3.53471118897989));
#54268=CARTESIAN_POINT('Ctrl Pts',(11.9526393438063,-0.229214786470442,
3.41657125348121));
#54269=CARTESIAN_POINT('Ctrl Pts',(11.9685446224939,-0.0325126988662629,
3.4058082039356));
#54270=CARTESIAN_POINT('Ctrl Pts',(11.9844499011816,0.164189388737916,3.39504515438998));
#54271=CARTESIAN_POINT('Ctrl Pts',(12.0003551798692,0.366766872773537,3.49165899079743));
#54272=CARTESIAN_POINT('Ctrl Pts',(12.0162604585568,0.482204742918021,3.65128872687397));
#54273=CARTESIAN_POINT('Ctrl Pts',(12.0321657372444,0.597642613062508,3.81091846295053));
#54274=CARTESIAN_POINT('Ctrl Pts',(12.048071015932,0.625940869315854,4.03356409869619));
#54275=CARTESIAN_POINT('Ctrl Pts',(12.0639762946196,0.554106149607013,4.21699617753661));
#54276=CARTESIAN_POINT('Ctrl Pts',(12.0798815733072,0.482271429898174,4.40042825637702));
#54277=CARTESIAN_POINT('Ctrl Pts',(12.0957868519948,0.310303734227154,4.5446467783122));
#54278=CARTESIAN_POINT('Ctrl Pts',(12.1116921306825,0.117163353092859,4.583432699452));
#54279=CARTESIAN_POINT('Ctrl Pts',(12.1148462833691,0.0788619649798074,
4.59112427906975));
#54280=CARTESIAN_POINT('Ctrl Pts',(12.1180004360558,0.0397279339241207,
4.59466958677844));
#54281=CARTESIAN_POINT('Ctrl Pts',(12.1211545887425,0.00052868291625318,
4.59430727435519));
#54282=CARTESIAN_POINT('Origin',(4.,0.,4.));
#54283=CARTESIAN_POINT('',(12.5288454112576,-0.000545899910317726,4.59395595168017));
#54284=CARTESIAN_POINT('',(12.4211545887425,4.74932194801069E-5,4.59311952367199));
#54285=CARTESIAN_POINT('',(4.,-7.27562663373442E-17,4.5941));
#54286=CARTESIAN_POINT('Ctrl Pts',(12.5288454112576,-0.000545899910317726,
4.59395595168017));
#54287=CARTESIAN_POINT('Ctrl Pts',(12.5170234109807,0.14659828900878,4.5926299020853));
#54288=CARTESIAN_POINT('Ctrl Pts',(12.5052014107038,0.29463204299547,4.53735693360054));
#54289=CARTESIAN_POINT('Ctrl Pts',(12.493379410427,0.402483765871145,4.43832383497591));
#54290=CARTESIAN_POINT('Ctrl Pts',(12.4774741317394,0.547587104485886,4.30508504322883));
#54291=CARTESIAN_POINT('Ctrl Pts',(12.4615688530518,0.619957272242066,4.09263639239171));
#54292=CARTESIAN_POINT('Ctrl Pts',(12.4456635743641,0.586364949835353,3.89852531496775));
#54293=CARTESIAN_POINT('Ctrl Pts',(12.4297582956765,0.55277262742864,3.7044142375438));
#54294=CARTESIAN_POINT('Ctrl Pts',(12.4138530169889,0.41321781485904,3.52864073353302));
#54295=CARTESIAN_POINT('Ctrl Pts',(12.3979477383013,0.231778177981285,3.45191255961345));
#54296=CARTESIAN_POINT('Ctrl Pts',(12.3820424596137,0.0503385411035255,
3.37518438569388));
#54297=CARTESIAN_POINT('Ctrl Pts',(12.3661371809261,-0.172985920082391,
3.39750154186552));
#54298=CARTESIAN_POINT('Ctrl Pts',(12.3502319022385,-0.335654061078685,
3.50861693417539));
#54299=CARTESIAN_POINT('Ctrl Pts',(12.3343266235509,-0.498322202074975,
3.61973232648525));
#54300=CARTESIAN_POINT('Ctrl Pts',(12.3184213448632,-0.600334022881645,
3.81964595493332));
#54301=CARTESIAN_POINT('Ctrl Pts',(12.3025160661756,-0.594850011148503,
4.0165659389844));
#54302=CARTESIAN_POINT('Ctrl Pts',(12.286610787488,-0.58936599941536,4.21348592303547));
#54303=CARTESIAN_POINT('Ctrl Pts',(12.2707055088004,-0.476386155142398,
4.40741226268955));
#54304=CARTESIAN_POINT('Ctrl Pts',(12.2548002301128,-0.307786043036728,
4.50930218712431));
#54305=CARTESIAN_POINT('Ctrl Pts',(12.2461486238277,-0.216076754679914,
4.564724762732));
#54306=CARTESIAN_POINT('Ctrl Pts',(12.2374970175426,-0.107910718865932,
4.59291589733543));
#54307=CARTESIAN_POINT('Ctrl Pts',(12.2288454112576,0.000142795628640946,
4.59314744373127));
#54308=CARTESIAN_POINT('Ctrl Pts',(12.1211545887425,0.00052868291625318,
4.59430727435519));
#54309=CARTESIAN_POINT('Ctrl Pts',(12.1339057147434,-0.157940052872902,
4.59284257311225));
#54310=CARTESIAN_POINT('Ctrl Pts',(12.1466568407444,-0.317474678016714,
4.52751565545538));
#54311=CARTESIAN_POINT('Ctrl Pts',(12.1594079667453,-0.427372353356377,
4.41409399619463));
#54312=CARTESIAN_POINT('Ctrl Pts',(12.1753132454329,-0.564454612073754,
4.27261605145303));
#54313=CARTESIAN_POINT('Ctrl Pts',(12.1912185241205,-0.62430606291093,4.0563068416254));
#54314=CARTESIAN_POINT('Ctrl Pts',(12.2071238028081,-0.579445451749542,
3.8644864045766));
#54315=CARTESIAN_POINT('Ctrl Pts',(12.2230290814957,-0.534584840588155,
3.6726659675278));
#54316=CARTESIAN_POINT('Ctrl Pts',(12.2389343601834,-0.38501216742821,3.50533430325784));
#54317=CARTESIAN_POINT('Ctrl Pts',(12.254839638871,-0.199404875886796,3.43932303278057));
#54318=CARTESIAN_POINT('Ctrl Pts',(12.2707449175586,-0.0137975843453769,
3.37331176230329));
#54319=CARTESIAN_POINT('Ctrl Pts',(12.2866501962462,0.207844325577514,3.40862088561871));
#54320=CARTESIAN_POINT('Ctrl Pts',(12.3025554749338,0.363752265741203,3.52903794710619));
#54321=CARTESIAN_POINT('Ctrl Pts',(12.3184607536214,0.519660205904889,3.64945500859368));
#54322=CARTESIAN_POINT('Ctrl Pts',(12.334366032309,0.609834176309377,3.85498000825323));
#54323=CARTESIAN_POINT('Ctrl Pts',(12.3502713109967,0.592870104691008,4.05124456128685));
#54324=CARTESIAN_POINT('Ctrl Pts',(12.3661765896843,0.575906033072638,4.24750911432049));
#54325=CARTESIAN_POINT('Ctrl Pts',(12.3820818683719,0.451803919431404,4.4345132207282));
#54326=CARTESIAN_POINT('Ctrl Pts',(12.3979871470595,0.277546204023914,4.52639250633888));
#54327=CARTESIAN_POINT('Ctrl Pts',(12.4057096276205,0.192938958450368,4.57100260157974));
#54328=CARTESIAN_POINT('Ctrl Pts',(12.4134321081815,0.0965080911524262,
4.59318808505049));
#54329=CARTESIAN_POINT('Ctrl Pts',(12.4211545887425,4.74932194801069E-5,
4.59311952367199));
#54330=CARTESIAN_POINT('Origin',(4.,0.,4.));
#54331=CARTESIAN_POINT('',(12.8288454112576,0.000112157221815526,4.59505491513413));
#54332=CARTESIAN_POINT('',(12.7211545887425,-0.000546355209092884,4.59413239245978));
#54333=CARTESIAN_POINT('',(4.,-7.27562663373442E-17,4.5941));
#54334=CARTESIAN_POINT('Ctrl Pts',(12.8288454112576,0.000112157221815526,
4.59505491513413));
#54335=CARTESIAN_POINT('Ctrl Pts',(12.828360361794,0.00612048155630211,
4.59507046002904));
#54336=CARTESIAN_POINT('Ctrl Pts',(12.8278753123304,0.0121283652366354,
4.59498736156652));
#54337=CARTESIAN_POINT('Ctrl Pts',(12.8273902628668,0.0181332013859869,
4.59480429815638));
#54338=CARTESIAN_POINT('Ctrl Pts',(12.8114849841792,0.215038052543873,4.58880145767424));
#54339=CARTESIAN_POINT('Ctrl Pts',(12.7955797054916,0.408666038032992,4.47531104548453));
#54340=CARTESIAN_POINT('Ctrl Pts',(12.779674426804,0.510111378641258,4.30644305748136));
#54341=CARTESIAN_POINT('Ctrl Pts',(12.7637691481164,0.611556719249521,4.1375750694782));
#54342=CARTESIAN_POINT('Ctrl Pts',(12.7478638694288,0.620819414976937,3.9133295056616));
#54343=CARTESIAN_POINT('Ctrl Pts',(12.7319585907412,0.533646427817818,3.7366704418887));
#54344=CARTESIAN_POINT('Ctrl Pts',(12.7160533120536,0.446473440658691,3.56001137811579));
#54345=CARTESIAN_POINT('Ctrl Pts',(12.700148033366,0.26286477061301,3.43093881438659));
#54346=CARTESIAN_POINT('Ctrl Pts',(12.6842427546783,0.0671257511235207,
3.4087174113557));
#54347=CARTESIAN_POINT('Ctrl Pts',(12.6683374759907,-0.128613268365957,
3.38649600832481));
#54348=CARTESIAN_POINT('Ctrl Pts',(12.6524321973031,-0.336482637299241,
3.47112576599221));
#54349=CARTESIAN_POINT('Ctrl Pts',(12.6365269186155,-0.461037535689932,
3.62374828002683));
#54350=CARTESIAN_POINT('Ctrl Pts',(12.6206216399279,-0.585592434080627,
3.77637079406146));
#54351=CARTESIAN_POINT('Ctrl Pts',(12.6047163612403,-0.626832861928724,
3.9969860644633));
#54352=CARTESIAN_POINT('Ctrl Pts',(12.5888110825527,-0.565822959504995,
4.18429689252621));
#54353=CARTESIAN_POINT('Ctrl Pts',(12.5729058038651,-0.504813057081268,
4.37160772058911));
#54354=CARTESIAN_POINT('Ctrl Pts',(12.5570005251774,-0.341552824385721,
4.52561410631309));
#54355=CARTESIAN_POINT('Ctrl Pts',(12.5410952464898,-0.151004453301302,
4.57560283284656));
#54356=CARTESIAN_POINT('Ctrl Pts',(12.5370119680791,-0.102085973774189,
4.58843617527608));
#54357=CARTESIAN_POINT('Ctrl Pts',(12.5329286896683,-0.0513689988622793,
4.59441396466913));
#54358=CARTESIAN_POINT('Ctrl Pts',(12.5288454112576,-0.000545899910317726,
4.59395595168017));
#54359=CARTESIAN_POINT('Ctrl Pts',(12.4211545887425,4.74932194801069E-5,
4.59311952367199));
#54360=CARTESIAN_POINT('Ctrl Pts',(12.4293373868691,-0.102162877376194,
4.59304687552285));
#54361=CARTESIAN_POINT('Ctrl Pts',(12.4375201849957,-0.204406628577491,
4.5679880979308));
#54362=CARTESIAN_POINT('Ctrl Pts',(12.4457029831223,-0.292652646395614,
4.51814611323009));
#54363=CARTESIAN_POINT('Ctrl Pts',(12.4616082618099,-0.46418046423393,4.42126596969699));
#54364=CARTESIAN_POINT('Ctrl Pts',(12.4775135404976,-0.582822782736806,
4.23075121781716));
#54365=CARTESIAN_POINT('Ctrl Pts',(12.4934188191852,-0.594104068590283,
4.03407817163935));
#54366=CARTESIAN_POINT('Ctrl Pts',(12.5093240978728,-0.605385354443759,
3.83740512546155));
#54367=CARTESIAN_POINT('Ctrl Pts',(12.5252293765604,-0.509305607647849,
3.63457378498577));
#54368=CARTESIAN_POINT('Ctrl Pts',(12.541134655248,-0.34998058313236,3.51871572067214));
#54369=CARTESIAN_POINT('Ctrl Pts',(12.5570399339356,-0.19065555861687,3.4028576563585));
#54370=CARTESIAN_POINT('Ctrl Pts',(12.5729452126232,0.031914743618199,3.37397286820701));
#54371=CARTESIAN_POINT('Ctrl Pts',(12.5888504913108,0.215535456959467,3.44532402892222));
#54372=CARTESIAN_POINT('Ctrl Pts',(12.6047557699985,0.399156170300736,3.51667518963742));
#54373=CARTESIAN_POINT('Ctrl Pts',(12.6206610486861,0.543827294748204,3.68826229921932));
#54374=CARTESIAN_POINT('Ctrl Pts',(12.6365663273737,0.583121970486127,3.88129981619987));
#54375=CARTESIAN_POINT('Ctrl Pts',(12.6524716060613,0.622416646224052,4.07433733318042));
#54376=CARTESIAN_POINT('Ctrl Pts',(12.6683768847489,0.556334873252426,4.28882525755962));
#54377=CARTESIAN_POINT('Ctrl Pts',(12.6842821634365,0.415218606030559,4.42627980869829));
#54378=CARTESIAN_POINT('Ctrl Pts',(12.6965729718718,0.306170972122536,4.53249785050629));
#54379=CARTESIAN_POINT('Ctrl Pts',(12.7088637803072,0.152317016475741,4.59271595401221));
#54380=CARTESIAN_POINT('Ctrl Pts',(12.7211545887425,-0.000546355209092884,
4.59413239245978));
#54381=CARTESIAN_POINT('Origin',(4.,0.,4.));
#54382=CARTESIAN_POINT('',(13.1288454112576,0.000488576923893258,4.59361798633976));
#54383=CARTESIAN_POINT('',(13.0211545887425,0.000215375668158819,4.59498635240753));
#54384=CARTESIAN_POINT('',(4.,-7.27562663373442E-17,4.5941));
#54385=CARTESIAN_POINT('Ctrl Pts',(13.1288454112576,0.000488576923893258,
4.59361798633976));
#54386=CARTESIAN_POINT('Ctrl Pts',(13.1237920339197,0.0634769139372694,
4.59410397103046));
#54387=CARTESIAN_POINT('Ctrl Pts',(13.1187386565818,0.126326538027094,4.58487602541266));
#54388=CARTESIAN_POINT('Ctrl Pts',(13.1136852792439,0.185787091792062,4.56533540718874));
#54389=CARTESIAN_POINT('Ctrl Pts',(13.0977800005563,0.372936519850693,4.50383218710482));
#54390=CARTESIAN_POINT('Ctrl Pts',(13.0818747218686,0.526512210440984,4.34016674272733));
#54391=CARTESIAN_POINT('Ctrl Pts',(13.065969443181,0.575998703695535,4.14948732200047));
#54392=CARTESIAN_POINT('Ctrl Pts',(13.0500641644934,0.625485196950086,3.9588079012736));
#54393=CARTESIAN_POINT('Ctrl Pts',(13.0341588858058,0.570882492868891,3.74111450419737));
#54394=CARTESIAN_POINT('Ctrl Pts',(13.0182536071182,0.437261843116128,3.59636272886105));
#54395=CARTESIAN_POINT('Ctrl Pts',(13.0023483284306,0.303641193363369,3.45161095352474));
#54396=CARTESIAN_POINT('Ctrl Pts',(12.986443049743,0.0910025979390456,3.37980079992835));
#54397=CARTESIAN_POINT('Ctrl Pts',(12.9705377710554,-0.10301929613509,3.41390445256627));
#54398=CARTESIAN_POINT('Ctrl Pts',(12.9546324923678,-0.297041190209231,
3.4480081052042));
#54399=CARTESIAN_POINT('Ctrl Pts',(12.9387272136801,-0.472446382933184,
3.58802556407645));
#54400=CARTESIAN_POINT('Ctrl Pts',(12.9228219349925,-0.54869623058984,3.76966673571907));
#54401=CARTESIAN_POINT('Ctrl Pts',(12.9069166563049,-0.624946078246494,
3.95130790736168));
#54402=CARTESIAN_POINT('Ctrl Pts',(12.8910113776173,-0.602040580835857,
4.17457279177466));
#54403=CARTESIAN_POINT('Ctrl Pts',(12.8751060989297,-0.490496973717212,
4.33694759959386));
#54404=CARTESIAN_POINT('Ctrl Pts',(12.8596858697056,-0.382355015061345,
4.49437060399126));
#54405=CARTESIAN_POINT('Ctrl Pts',(12.8442656404816,-0.190898750836606,
4.59456072668396));
#54406=CARTESIAN_POINT('Ctrl Pts',(12.8288454112576,0.000112157221815526,
4.59505491513413));
#54407=CARTESIAN_POINT('Ctrl Pts',(12.7211545887425,-0.000546355209092884,
4.59413239245978));
#54408=CARTESIAN_POINT('Ctrl Pts',(12.7247690589948,-0.0455002825709059,
4.59454893744622));
#54409=CARTESIAN_POINT('Ctrl Pts',(12.7283835292471,-0.0903685417208244,
4.58988016539195));
#54410=CARTESIAN_POINT('Ctrl Pts',(12.7319979994994,-0.13398639330236,4.5798004937111));
#54411=CARTESIAN_POINT('Ctrl Pts',(12.747903278187,-0.325924363941296,4.53544544968711));
#54412=CARTESIAN_POINT('Ctrl Pts',(12.7638085568746,-0.493649543747071,
4.38631418374101));
#54413=CARTESIAN_POINT('Ctrl Pts',(12.7797138355622,-0.560149626020051,
4.20088146397168));
#54414=CARTESIAN_POINT('Ctrl Pts',(12.7956191142498,-0.626649708293032,
4.01544874420235));
#54415=CARTESIAN_POINT('Ctrl Pts',(12.8115243929374,-0.591924693033219,
3.79371457060979));
#54416=CARTESIAN_POINT('Ctrl Pts',(12.827429671625,-0.471918838153678,3.63748989490844));
#54417=CARTESIAN_POINT('Ctrl Pts',(12.8433349503126,-0.351912983274129,
3.48126521920708));
#54418=CARTESIAN_POINT('Ctrl Pts',(12.8592402290002,-0.146626288774854,
3.39055004139693));
#54419=CARTESIAN_POINT('Ctrl Pts',(12.8751455076879,0.0496822801939141,
3.40699693328572));
#54420=CARTESIAN_POINT('Ctrl Pts',(12.8910507863755,0.245990849162665,3.42344382517451));
#54421=CARTESIAN_POINT('Ctrl Pts',(12.9069560650631,0.433321292600904,3.54705278676224));
#54422=CARTESIAN_POINT('Ctrl Pts',(12.9228613437507,0.525659396179275,3.72106781235173));
#54423=CARTESIAN_POINT('Ctrl Pts',(12.9387666224383,0.617997499757654,3.89508283794124));
#54424=CARTESIAN_POINT('Ctrl Pts',(12.9546719011259,0.615343263476151,4.11950392753251));
#54425=CARTESIAN_POINT('Ctrl Pts',(12.9705771798135,0.518915400343756,4.29128641125856));
#54426=CARTESIAN_POINT('Ctrl Pts',(12.9864824585012,0.422487537211366,4.46306889498459));
#54427=CARTESIAN_POINT('Ctrl Pts',(13.0023877371888,0.232286047228094,4.58221277284539));
#54428=CARTESIAN_POINT('Ctrl Pts',(13.0182930158764,0.0356434078328121,
4.59401221668908));
#54429=CARTESIAN_POINT('Ctrl Pts',(13.0192468734984,0.0238505254767134,
4.59471984273368));
#54430=CARTESIAN_POINT('Ctrl Pts',(13.0202007311205,0.0120344772878951,
4.59504140054066));
#54431=CARTESIAN_POINT('Ctrl Pts',(13.0211545887425,0.000215375668158819,
4.59498635240753));
#54432=CARTESIAN_POINT('Origin',(4.,0.,4.));
#54433=CARTESIAN_POINT('',(13.4288454112576,-0.000323145728561625,4.59329116515504));
#54434=CARTESIAN_POINT('',(13.3211545887425,0.000436239896754628,4.59347700091179));
#54435=CARTESIAN_POINT('',(4.,-7.27562663373442E-17,4.5941));
#54436=CARTESIAN_POINT('Ctrl Pts',(13.4288454112576,-0.000323145728561625,
4.59329116515504));
#54437=CARTESIAN_POINT('Ctrl Pts',(13.4192237060453,0.11977362227264,4.59270025156928));
#54438=CARTESIAN_POINT('Ctrl Pts',(13.4096020008331,0.240190260834984,4.55734300206483));
#54439=CARTESIAN_POINT('Ctrl Pts',(13.3999802956209,0.338238798929947,4.48960747645051));
#54440=CARTESIAN_POINT('Ctrl Pts',(13.3840750169333,0.500319146323361,4.37763642888821));
#54441=CARTESIAN_POINT('Ctrl Pts',(13.3681697382457,0.601276083433826,4.17718801339723));
#54442=CARTESIAN_POINT('Ctrl Pts',(13.3522644595581,0.594754455875995,3.9802996620979));
#54443=CARTESIAN_POINT('Ctrl Pts',(13.3363591808704,0.588232828318166,3.78341131079859));
#54444=CARTESIAN_POINT('Ctrl Pts',(13.3204539021828,0.474232636092054,3.59008302369095));
#54445=CARTESIAN_POINT('Ctrl Pts',(13.3045486234952,0.305097944517489,3.48908297116948));
#54446=CARTESIAN_POINT('Ctrl Pts',(13.2886433448076,0.135963252942929,3.388082918648));
#54447=CARTESIAN_POINT('Ctrl Pts',(13.27273806612,-0.0883059379800925,3.3794111007127));
#54448=CARTESIAN_POINT('Ctrl Pts',(13.2568327874324,-0.264734703826722,
3.46704924928509));
#54449=CARTESIAN_POINT('Ctrl Pts',(13.2409275087448,-0.441163469673367,
3.55468739785749));
#54450=CARTESIAN_POINT('Ctrl Pts',(13.2250222300572,-0.569751810443623,
3.7386355129376));
#54451=CARTESIAN_POINT('Ctrl Pts',(13.2091169513696,-0.591457400179852,
3.9344324022836));
#54452=CARTESIAN_POINT('Ctrl Pts',(13.1932116726819,-0.613162989916079,
4.1302292916296));
#54453=CARTESIAN_POINT('Ctrl Pts',(13.1773063939943,-0.527985828618295,
4.33787495524147));
#54454=CARTESIAN_POINT('Ctrl Pts',(13.1614011153067,-0.375035665205916,
4.46202728915223));
#54455=CARTESIAN_POINT('Ctrl Pts',(13.150549213957,-0.270680367988337,4.54673431669939));
#54456=CARTESIAN_POINT('Ctrl Pts',(13.1396973126073,-0.134776053786733,
4.59257435599745));
#54457=CARTESIAN_POINT('Ctrl Pts',(13.1288454112576,0.000488576923893258,
4.59361798633976));
#54458=CARTESIAN_POINT('Ctrl Pts',(13.0211545887425,0.000215375668158819,
4.59498635240753));
#54459=CARTESIAN_POINT('Ctrl Pts',(13.0361060098081,-0.185045360160338,
4.59412349007018));
#54460=CARTESIAN_POINT('Ctrl Pts',(13.0510574308736,-0.371056311319581,
4.5007301079696));
#54461=CARTESIAN_POINT('Ctrl Pts',(13.0660088519392,-0.480360474535337,
4.35124746348123));
#54462=CARTESIAN_POINT('Ctrl Pts',(13.0819141306268,-0.596637928700896,
4.19222825660313));
#54463=CARTESIAN_POINT('Ctrl Pts',(13.0978194093145,-0.626109048224722,
3.96973483302036));
#54464=CARTESIAN_POINT('Ctrl Pts',(13.1137246880021,-0.555241941841719,
3.78592675992164));
#54465=CARTESIAN_POINT('Ctrl Pts',(13.1296299666897,-0.484374835458714,
3.60211868682292));
#54466=CARTESIAN_POINT('Ctrl Pts',(13.1455352453773,-0.313169503168878,
3.45699596420825));
#54467=CARTESIAN_POINT('Ctrl Pts',(13.1614405240649,-0.120236190459409,
3.4171928066662));
#54468=CARTESIAN_POINT('Ctrl Pts',(13.1773458027525,0.0726971222500488,
3.37738964912416));
#54469=CARTESIAN_POINT('Ctrl Pts',(13.1932510814401,0.287358415379145,3.44290605665475));
#54470=CARTESIAN_POINT('Ctrl Pts',(13.2091563601277,0.425184304693362,3.58365966669054));
#54471=CARTESIAN_POINT('Ctrl Pts',(13.2250616388154,0.563010194007583,3.72441327672633));
#54472=CARTESIAN_POINT('Ctrl Pts',(13.240966917503,0.624000679506934,3.94040408926733));
#54473=CARTESIAN_POINT('Ctrl Pts',(13.2568721961906,0.580151510544767,4.13245826101242));
#54474=CARTESIAN_POINT('Ctrl Pts',(13.2727774748782,0.536302341582597,4.32451243275751));
#54475=CARTESIAN_POINT('Ctrl Pts',(13.2886827535658,0.387613518158899,4.49262996370669));
#54476=CARTESIAN_POINT('Ctrl Pts',(13.3045880322534,0.202356657484476,4.55961839611428));
#54477=CARTESIAN_POINT('Ctrl Pts',(13.3101102177498,0.13803695776657,4.58287624384712));
#54478=CARTESIAN_POINT('Ctrl Pts',(13.3156324032461,0.0693092633201986,
4.59394375907155));
#54479=CARTESIAN_POINT('Ctrl Pts',(13.3211545887425,0.000436239896754628,
4.59347700091179));
#54480=CARTESIAN_POINT('Origin',(4.,0.,4.));
#54481=CARTESIAN_POINT('',(13.7288454112576,-0.000361622974213827,4.59480268714608));
#54482=CARTESIAN_POINT('',(13.6211545887425,-0.000396530615921017,4.59339874939382));
#54483=CARTESIAN_POINT('',(4.,-7.27562663373442E-17,4.5941));
#54484=CARTESIAN_POINT('Ctrl Pts',(13.7288454112576,-0.000361622974213827,
4.59480268714608));
#54485=CARTESIAN_POINT('Ctrl Pts',(13.714655378171,0.175608319374377,4.59354294412002));
#54486=CARTESIAN_POINT('Ctrl Pts',(13.7004653450845,0.352610168065205,4.51056419690263));
#54487=CARTESIAN_POINT('Ctrl Pts',(13.6862753119979,0.463013835099274,4.37381700684221));
#54488=CARTESIAN_POINT('Ctrl Pts',(13.6703700333103,0.586762742631886,4.22054025587244));
#54489=CARTESIAN_POINT('Ctrl Pts',(13.6544647546227,0.626840040937572,3.99971072753873));
#54490=CARTESIAN_POINT('Ctrl Pts',(13.6385594759351,0.564843930165024,3.81272399872504));
#54491=CARTESIAN_POINT('Ctrl Pts',(13.6226541972475,0.502847819392478,3.62573726991136));
#54492=CARTESIAN_POINT('Ctrl Pts',(13.6067489185599,0.338778299541704,3.4725933406177));
#54493=CARTESIAN_POINT('Ctrl Pts',(13.5908436398723,0.147969152919217,3.42360942419035));
#54494=CARTESIAN_POINT('Ctrl Pts',(13.5749383611846,-0.0428399937032757,
3.37462550776301));
#54495=CARTESIAN_POINT('Ctrl Pts',(13.559033082497,-0.260388767097474,3.42980160420198));
#54496=CARTESIAN_POINT('Ctrl Pts',(13.5431278038094,-0.404787974250376,
3.56380318433064));
#54497=CARTESIAN_POINT('Ctrl Pts',(13.5272225251218,-0.549187181403275,
3.6978047644593));
#54498=CARTESIAN_POINT('Ctrl Pts',(13.5113172464342,-0.620436822314871,
3.91063182827765));
#54499=CARTESIAN_POINT('Ctrl Pts',(13.4954119677466,-0.585822076202281,
4.10456319205082));
#54500=CARTESIAN_POINT('Ctrl Pts',(13.479506689059,-0.551207330089691,4.298494555824));
#54501=CARTESIAN_POINT('Ctrl Pts',(13.4636014103714,-0.410728196952908,
4.47353021955202));
#54502=CARTESIAN_POINT('Ctrl Pts',(13.4476961316837,-0.228886751546343,
4.54930121159921));
#54503=CARTESIAN_POINT('Ctrl Pts',(13.4414125582084,-0.15704808052867,4.57923546205676));
#54504=CARTESIAN_POINT('Ctrl Pts',(13.435128984733,-0.0787538239969463,
4.5936770685736));
#54505=CARTESIAN_POINT('Ctrl Pts',(13.4288454112576,-0.000323145728561625,
4.59329116515504));
#54506=CARTESIAN_POINT('Ctrl Pts',(13.3211545887425,0.000436239896754628,
4.59347700091179));
#54507=CARTESIAN_POINT('Ctrl Pts',(13.3315376819337,-0.129062311182503,
4.59259937855127));
#54508=CARTESIAN_POINT('Ctrl Pts',(13.341920775125,-0.259074650003773,4.55094414667863));
#54509=CARTESIAN_POINT('Ctrl Pts',(13.3523038683163,-0.361265427801182,
4.47287234722855));
#54510=CARTESIAN_POINT('Ctrl Pts',(13.3682091470039,-0.517805754487323,
4.35327853206923));
#54511=CARTESIAN_POINT('Ctrl Pts',(13.3841144256915,-0.609061509934468,
4.14823156788458));
#54512=CARTESIAN_POINT('Ctrl Pts',(13.4000197043791,-0.593131911953917,
3.95188034580653));
#54513=CARTESIAN_POINT('Ctrl Pts',(13.4159249830667,-0.577202313973367,
3.75552912372848));
#54514=CARTESIAN_POINT('Ctrl Pts',(13.4318302617543,-0.454087362565127,
3.56787364375704));
#54515=CARTESIAN_POINT('Ctrl Pts',(13.4477355404419,-0.280316234851803,
3.47507736324643));
#54516=CARTESIAN_POINT('Ctrl Pts',(13.4636408191295,-0.106545107138479,
3.38228108273583));
#54517=CARTESIAN_POINT('Ctrl Pts',(13.4795460978172,0.117882196879929,3.38434400168606));
#54518=CARTESIAN_POINT('Ctrl Pts',(13.4954513765048,0.2899181539344,3.48031891499009));
#54519=CARTESIAN_POINT('Ctrl Pts',(13.5113566551924,0.461954110988876,3.57629382829412));
#54520=CARTESIAN_POINT('Ctrl Pts',(13.52726193388,0.581598721079409,3.76618073595195));
#54521=CARTESIAN_POINT('Ctrl Pts',(13.5431672125676,0.593916240998451,3.96279160341967));
#54522=CARTESIAN_POINT('Ctrl Pts',(13.5590724912552,0.606233760917493,4.15940247088739));
#54523=CARTESIAN_POINT('Ctrl Pts',(13.5749777699428,0.511224190665043,4.362737298165));
#54524=CARTESIAN_POINT('Ctrl Pts',(13.5908830486304,0.352511905377589,4.47943333495374));
#54525=CARTESIAN_POINT('Ctrl Pts',(13.6009735620011,0.251822790258117,4.55346680161908));
#54526=CARTESIAN_POINT('Ctrl Pts',(13.6110640753718,0.125494626822297,4.59262991567553));
#54527=CARTESIAN_POINT('Ctrl Pts',(13.6211545887425,-0.000396530615921017,
4.59339874939382));
#54528=CARTESIAN_POINT('Origin',(4.,0.,4.));
#54529=CARTESIAN_POINT('',(14.0288454112576,0.000507412974116619,4.59441995931617));
#54530=CARTESIAN_POINT('',(13.9211545887425,-0.000275297881949146,4.59492513410986));
#54531=CARTESIAN_POINT('',(4.,-7.27562663373442E-17,4.5941));
#54532=CARTESIAN_POINT('Ctrl Pts',(14.0288454112576,0.000507412974116619,
4.59441995931617));
#54533=CARTESIAN_POINT('Ctrl Pts',(14.0259923289843,0.0359476882196221,
4.59474138052009));
#54534=CARTESIAN_POINT('Ctrl Pts',(14.0231392467111,0.0713355155074759,
4.59184535342408));
#54535=CARTESIAN_POINT('Ctrl Pts',(14.0202861644378,0.106106362061302,4.58554453803953));
#54536=CARTESIAN_POINT('Ctrl Pts',(14.0043808857502,0.299945849210873,4.55041893875697));
#54537=CARTESIAN_POINT('Ctrl Pts',(13.9884756070626,0.474610768799237,4.40947910659883));
#54538=CARTESIAN_POINT('Ctrl Pts',(13.972570328375,0.549902379214768,4.22743864981956));
#54539=CARTESIAN_POINT('Ctrl Pts',(13.9566650496873,0.625193989630293,4.04539819304031));
#54540=CARTESIAN_POINT('Ctrl Pts',(13.9407597709997,0.601112290873006,3.82225711163994));
#54541=CARTESIAN_POINT('Ctrl Pts',(13.9248544923121,0.488714580199595,3.66047234987686));
#54542=CARTESIAN_POINT('Ctrl Pts',(13.9089492136245,0.376316869526181,3.49868758811377));
#54543=CARTESIAN_POINT('Ctrl Pts',(13.8930439349369,0.175603146936639,3.39825914598798));
#54544=CARTESIAN_POINT('Ctrl Pts',(13.8771386562493,-0.0212673376532481,
3.40529951534663));
#54545=CARTESIAN_POINT('Ctrl Pts',(13.8612333775617,-0.218137822243141,
3.41233988470529));
#54546=CARTESIAN_POINT('Ctrl Pts',(13.8453280988741,-0.411165068833379,
3.52684906554841));
#54547=CARTESIAN_POINT('Ctrl Pts',(13.8294228201864,-0.511719132099071,
3.69624928651676));
#54548=CARTESIAN_POINT('Ctrl Pts',(13.8135175414988,-0.612273195364761,
3.8656495074851));
#54549=CARTESIAN_POINT('Ctrl Pts',(13.7976122628112,-0.62035407530591,4.08994076857866));
#54550=CARTESIAN_POINT('Ctrl Pts',(13.7817069841236,-0.532251373727382,
4.26613801168402));
#54551=CARTESIAN_POINT('Ctrl Pts',(13.765801705436,-0.44414867214885,4.44233525478938));
#54552=CARTESIAN_POINT('Ctrl Pts',(13.7498964267484,-0.259862389050636,
4.57043847990653));
#54553=CARTESIAN_POINT('Ctrl Pts',(13.7339911480608,-0.0640089891217576,
4.59162810566218));
#54554=CARTESIAN_POINT('Ctrl Pts',(13.7322759024597,-0.0428879079209441,
4.59391322201126));
#54555=CARTESIAN_POINT('Ctrl Pts',(13.7305606568586,-0.0216323041412813,
4.594954960835));
#54556=CARTESIAN_POINT('Ctrl Pts',(13.7288454112576,-0.000361622974213827,
4.59480268714608));
#54557=CARTESIAN_POINT('Ctrl Pts',(13.6211545887425,-0.000396530615921017,
4.59339874939382));
#54558=CARTESIAN_POINT('Ctrl Pts',(13.6269693540594,-0.0729426448807452,
4.59384179797573));
#54559=CARTESIAN_POINT('Ctrl Pts',(13.6327841193764,-0.145343639818557,
4.58153501668255));
#54560=CARTESIAN_POINT('Ctrl Pts',(13.6385988846933,-0.212609537044371,
4.5558040579697));
#54561=CARTESIAN_POINT('Ctrl Pts',(13.6545041633809,-0.396603693856438,
4.48542149789704));
#54562=CARTESIAN_POINT('Ctrl Pts',(13.6704094420685,-0.542177007158105,
4.31459913145184));
#54563=CARTESIAN_POINT('Ctrl Pts',(13.6863147207561,-0.582488370180261,
4.12177136240739));
#54564=CARTESIAN_POINT('Ctrl Pts',(13.7022199994437,-0.622799733202417,
3.92894359336294));
#54565=CARTESIAN_POINT('Ctrl Pts',(13.7181252781313,-0.557849145945042,
3.71411042171923));
#54566=CARTESIAN_POINT('Ctrl Pts',(13.734030556819,-0.417459170243993,3.57591415105311));
#54567=CARTESIAN_POINT('Ctrl Pts',(13.7499358355066,-0.277069194542941,
3.43771788038699));
#54568=CARTESIAN_POINT('Ctrl Pts',(13.7658411141942,-0.0612398303982075,
3.37615851069845));
#54569=CARTESIAN_POINT('Ctrl Pts',(13.7817463928818,0.130929209162332,3.41950150018632));
#54570=CARTESIAN_POINT('Ctrl Pts',(13.7976516715694,0.323098248722867,3.46284448967418));
#54571=CARTESIAN_POINT('Ctrl Pts',(13.813556950257,0.491606963699209,3.61108983833845));
#54572=CARTESIAN_POINT('Ctrl Pts',(13.8294622289446,0.559083281190044,3.79616955381596));
#54573=CARTESIAN_POINT('Ctrl Pts',(13.8453675076322,0.62655959868088,3.98124926929349));
#54574=CARTESIAN_POINT('Ctrl Pts',(13.8612727863198,0.593003518686204,4.20316335158427));
#54575=CARTESIAN_POINT('Ctrl Pts',(13.8771780650075,0.4738225734989,4.36001824251097));
#54576=CARTESIAN_POINT('Ctrl Pts',(13.8918369062525,0.363981395029584,4.50458099992985));
#54577=CARTESIAN_POINT('Ctrl Pts',(13.9064957474975,0.181409709145346,4.59388191268165));
#54578=CARTESIAN_POINT('Ctrl Pts',(13.9211545887425,-0.000275297881949146,
4.59492513410986));
#54579=CARTESIAN_POINT('Origin',(4.,0.,4.));
#54580=CARTESIAN_POINT('',(14.3288454112576,0.000109044058801022,4.5931342436645));
#54581=CARTESIAN_POINT('',(14.2211545887425,0.000537210645871958,4.59424369460725));
#54582=CARTESIAN_POINT('',(4.,-7.27562663373442E-17,4.5941));
#54583=CARTESIAN_POINT('Ctrl Pts',(14.3288454112576,0.000109044058801022,
4.5931342436645));
#54584=CARTESIAN_POINT('Ctrl Pts',(14.32142400111,0.0928032711674493,4.59328573107644));
#54585=CARTESIAN_POINT('Ctrl Pts',(14.3140025909624,0.185434358886594,4.57287353691408));
#54586=CARTESIAN_POINT('Ctrl Pts',(14.3065811808148,0.267539471941071,4.53154830171049));
#54587=CARTESIAN_POINT('Ctrl Pts',(14.2906759021272,0.443503969097433,4.44298165875801));
#54588=CARTESIAN_POINT('Ctrl Pts',(14.2747706234396,0.571121189235106,4.25835848700565));
#54589=CARTESIAN_POINT('Ctrl Pts',(14.258865344752,0.591794703906212,4.06244993615984));
#54590=CARTESIAN_POINT('Ctrl Pts',(14.2429600660644,0.612468218577319,3.86654138531401));
#54591=CARTESIAN_POINT('Ctrl Pts',(14.2270547873768,0.526198027781844,3.65934745537473));
#54592=CARTESIAN_POINT('Ctrl Pts',(14.2111495086891,0.372595753342289,3.53600283331781));
#54593=CARTESIAN_POINT('Ctrl Pts',(14.1952442300015,0.218993478902743,3.4126582112609));
#54594=CARTESIAN_POINT('Ctrl Pts',(14.1793389513139,-0.00194087918087354,
3.37316289708635));
#54595=CARTESIAN_POINT('Ctrl Pts',(14.1634336726263,-0.18876361063844,3.43565146815417));
#54596=CARTESIAN_POINT('Ctrl Pts',(14.1475283939387,-0.375586342096006,
3.49814003922198));
#54597=CARTESIAN_POINT('Ctrl Pts',(14.1316231152511,-0.528297446927522,
3.66261249553216));
#54598=CARTESIAN_POINT('Ctrl Pts',(14.1157178365635,-0.576778446468407,
3.85355004340287));
#54599=CARTESIAN_POINT('Ctrl Pts',(14.0998125578759,-0.625259446009293,
4.04448759127359));
#54600=CARTESIAN_POINT('Ctrl Pts',(14.0839072791882,-0.569510340259543,
4.26189023070484));
#54601=CARTESIAN_POINT('Ctrl Pts',(14.0680020005006,-0.435128760029281,
4.40593586721696));
#54602=CARTESIAN_POINT('Ctrl Pts',(14.0549498040863,-0.324852491748397,
4.52414265738481));
#54603=CARTESIAN_POINT('Ctrl Pts',(14.0418976076719,-0.161623710204441,
4.5929495310973));
#54604=CARTESIAN_POINT('Ctrl Pts',(14.0288454112576,0.000507412974116619,
4.59441995931617));
#54605=CARTESIAN_POINT('Ctrl Pts',(13.9211545887425,-0.000275297881949146,
4.59492513410986));
#54606=CARTESIAN_POINT('Ctrl Pts',(13.9224010261851,-0.015723926578741,
4.59501383895544));
#54607=CARTESIAN_POINT('Ctrl Pts',(13.9236474636277,-0.0311661445373128,
4.59446443570748));
#54608=CARTESIAN_POINT('Ctrl Pts',(13.9248939010703,-0.0465566941337027,
4.59325663951544));
#54609=CARTESIAN_POINT('Ctrl Pts',(13.9407991797579,-0.242949206199084,
4.5778444460306));
#54610=CARTESIAN_POINT('Ctrl Pts',(13.9567044584455,-0.430928419949921,
4.4552243594983));
#54611=CARTESIAN_POINT('Ctrl Pts',(13.9726097371331,-0.524182233176515,
4.28169833602613));
#54612=CARTESIAN_POINT('Ctrl Pts',(13.9885150158207,-0.617436046403107,
4.10817231255396));
#54613=CARTESIAN_POINT('Ctrl Pts',(14.0044202945084,-0.615964459105464,
3.88374035214192));
#54614=CARTESIAN_POINT('Ctrl Pts',(14.020325573196,-0.52044316191294,3.71145211607799));
#54615=CARTESIAN_POINT('Ctrl Pts',(14.0362308518836,-0.424921864720413,
3.53916388001405));
#54616=CARTESIAN_POINT('Ctrl Pts',(14.0521361305712,-0.235350857633014,
3.41901936829824));
#54617=CARTESIAN_POINT('Ctrl Pts',(14.0680414092588,-0.0387731270173405,
3.40618385781531));
#54618=CARTESIAN_POINT('Ctrl Pts',(14.0839466879464,0.157804603598333,3.39334834733239));
#54619=CARTESIAN_POINT('Ctrl Pts',(14.0998519666341,0.361389057742269,3.48782183808236));
#54620=CARTESIAN_POINT('Ctrl Pts',(14.1157572453217,0.478502867019537,3.64622609995664));
#54621=CARTESIAN_POINT('Ctrl Pts',(14.1316625240093,0.595616676296804,3.80463036183091));
#54622=CARTESIAN_POINT('Ctrl Pts',(14.1475678026969,0.626259840707404,4.02696539482948));
#54623=CARTESIAN_POINT('Ctrl Pts',(14.1634730813845,0.556362315559365,4.21114435801894));
#54624=CARTESIAN_POINT('Ctrl Pts',(14.1793783600721,0.486464790411328,4.3953233212084));
#54625=CARTESIAN_POINT('Ctrl Pts',(14.1952836387597,0.316026575704654,4.54134621458875));
#54626=CARTESIAN_POINT('Ctrl Pts',(14.2111889174473,0.123305688986428,4.58216550323889));
#54627=CARTESIAN_POINT('Ctrl Pts',(14.2145108078791,0.0830550475387342,
4.59069079896363));
#54628=CARTESIAN_POINT('Ctrl Pts',(14.2178326983108,0.0418324306113591,
4.59462708830176));
#54629=CARTESIAN_POINT('Ctrl Pts',(14.2211545887425,0.000537210645871958,
4.59424369460725));
#54630=CARTESIAN_POINT('Origin',(4.,0.,4.));
#54631=CARTESIAN_POINT('',(14.6288454112575,-0.000548182068839831,4.59401855345973));
#54632=CARTESIAN_POINT('',(14.5211545887425,1.28950532977596E-5,4.59311636453746));
#54633=CARTESIAN_POINT('',(4.,-7.27562663373442E-17,4.5941));
#54634=CARTESIAN_POINT('Ctrl Pts',(14.6288454112575,-0.000548182068839831,
4.59401855345973));
#54635=CARTESIAN_POINT('Ctrl Pts',(14.6168556732357,0.148643716013534,4.59265593252186));
#54636=CARTESIAN_POINT('Ctrl Pts',(14.6048659352138,0.29876355451001,4.53564313143304));
#54637=CARTESIAN_POINT('Ctrl Pts',(14.5928761971919,0.407080942069735,4.43405768361063));
#54638=CARTESIAN_POINT('Ctrl Pts',(14.5769709185042,0.55077200793829,4.29929703619113));
#54639=CARTESIAN_POINT('Ctrl Pts',(14.5610656398166,0.620899143473568,4.08609746938767));
#54640=CARTESIAN_POINT('Ctrl Pts',(14.545160361129,0.585262934872208,3.89235120454656));
#54641=CARTESIAN_POINT('Ctrl Pts',(14.5292550824414,0.549626726270847,3.69860493970543));
#54642=CARTESIAN_POINT('Ctrl Pts',(14.5133498037538,0.408227173532835,3.52431197682665));
#54643=CARTESIAN_POINT('Ctrl Pts',(14.4974445250662,0.225988969153725,3.44950027073699));
#54644=CARTESIAN_POINT('Ctrl Pts',(14.4815392463786,0.04375076477463,3.37468856464734));
#54645=CARTESIAN_POINT('Ctrl Pts',(14.465633967691,-0.179326091245555,3.39935811534679));
#54646=CARTESIAN_POINT('Ctrl Pts',(14.4497286890033,-0.340814144225853,
3.51218170883678));
#54647=CARTESIAN_POINT('Ctrl Pts',(14.4338234103157,-0.50230219720616,3.62500530232677));
#54648=CARTESIAN_POINT('Ctrl Pts',(14.4179181316281,-0.602201447146573,
3.82598293860731));
#54649=CARTESIAN_POINT('Ctrl Pts',(14.4020128529405,-0.594642384863179,
4.02283418976097));
#54650=CARTESIAN_POINT('Ctrl Pts',(14.3861075742529,-0.587083322579785,
4.21968544091462));
#54651=CARTESIAN_POINT('Ctrl Pts',(14.3702022955653,-0.47206594807259,4.4124103069414));
#54652=CARTESIAN_POINT('Ctrl Pts',(14.3542970168777,-0.302401373731467,
4.51251768287848));
#54653=CARTESIAN_POINT('Ctrl Pts',(14.3458131483376,-0.211902365642262,
4.565914912441));
#54654=CARTESIAN_POINT('Ctrl Pts',(14.3373292797976,-0.10585540495725,4.59296106912451));
#54655=CARTESIAN_POINT('Ctrl Pts',(14.3288454112576,0.000109044058801022,
4.5931342436645));
#54656=CARTESIAN_POINT('Ctrl Pts',(14.2211545887425,0.000537210645871958,
4.59424369460725));
#54657=CARTESIAN_POINT('Ctrl Pts',(14.2337379769984,-0.155889919212927,
4.59279139152499));
#54658=CARTESIAN_POINT('Ctrl Pts',(14.2463213652543,-0.313358837143528,
4.52935553548989));
#54659=CARTESIAN_POINT('Ctrl Pts',(14.2589047535102,-0.422984449084643,
4.4185751090669));
#54660=CARTESIAN_POINT('Ctrl Pts',(14.2748100321978,-0.561550141707708,
4.27854974232482));
#54661=CARTESIAN_POINT('Ctrl Pts',(14.2907153108854,-0.623677968224056,
4.06288332492072));
#54662=CARTESIAN_POINT('Ctrl Pts',(14.306620589573,-0.580841459108965,3.87060075163287));
#54663=CARTESIAN_POINT('Ctrl Pts',(14.3225258682606,-0.538004949993874,
3.67831817834502));
#54664=CARTESIAN_POINT('Ctrl Pts',(14.3384311469482,-0.390204105247342,
3.50941944917344));
#54665=CARTESIAN_POINT('Ctrl Pts',(14.3543364256359,-0.205302819838896,
3.44145571503774));
#54666=CARTESIAN_POINT('Ctrl Pts',(14.3702417043235,-0.0204015344304391,
3.37349198090203));
#54667=CARTESIAN_POINT('Ctrl Pts',(14.3861469830111,0.201600191639931,3.40646324180223));
#54668=CARTESIAN_POINT('Ctrl Pts',(14.4020522616987,0.358768557879186,3.52523048963197));
#54669=CARTESIAN_POINT('Ctrl Pts',(14.4179575403863,0.515936924118427,3.6439977374617));
#54670=CARTESIAN_POINT('Ctrl Pts',(14.4338628190739,0.608271930526566,3.84856097222098));
#54671=CARTESIAN_POINT('Ctrl Pts',(14.4497680977615,0.59337724853295,4.04499341086509));
#54672=CARTESIAN_POINT('Ctrl Pts',(14.4656733764491,0.578482566539332,4.2414258495092));
#54673=CARTESIAN_POINT('Ctrl Pts',(14.4815786551367,0.456358196143958,4.42972749203816));
#54674=CARTESIAN_POINT('Ctrl Pts',(14.4974839338244,0.283078481576349,4.52343819058819));
#54675=CARTESIAN_POINT('Ctrl Pts',(14.5053741521304,0.197118668938093,4.56992576768087));
#54676=CARTESIAN_POINT('Ctrl Pts',(14.5132643704364,0.0985699939877532,
4.59313537862966));
#54677=CARTESIAN_POINT('Ctrl Pts',(14.5211545887425,1.28950532977596E-5,
4.59311636453746));
#54678=CARTESIAN_POINT('Origin',(4.,0.,4.));
#54679=CARTESIAN_POINT('',(14.9288454112575,0.000149915246051877,4.59503491979621));
#54680=CARTESIAN_POINT('',(14.8211545887425,-0.000542004001680995,4.59419620878869));
#54681=CARTESIAN_POINT('',(4.,-7.27562663373442E-17,4.5941));
#54682=CARTESIAN_POINT('Ctrl Pts',(14.9288454112575,0.000149915246051877,
4.59503491979621));
#54683=CARTESIAN_POINT('Ctrl Pts',(14.9281926240489,0.00823674021970066,
4.59506221957623));
#54684=CARTESIAN_POINT('Ctrl Pts',(14.9275398368403,0.0163225255999611,
4.59491168338633));
#54685=CARTESIAN_POINT('Ctrl Pts',(14.9268870496317,0.0244008833477238,
4.59458015690877));
#54686=CARTESIAN_POINT('Ctrl Pts',(14.9109817709441,0.221231534471853,4.58650245417764));
#54687=CARTESIAN_POINT('Ctrl Pts',(14.8950764922565,0.413652681988333,4.47097768448731));
#54688=CARTESIAN_POINT('Ctrl Pts',(14.8791712135689,0.513312675625014,4.30104993462962));
#54689=CARTESIAN_POINT('Ctrl Pts',(14.8632659348813,0.612972669261697,4.13112218477192));
#54690=CARTESIAN_POINT('Ctrl Pts',(14.8473606561937,0.619871509018575,3.90679145474687));
#54691=CARTESIAN_POINT('Ctrl Pts',(14.831455377506,0.530841539545133,3.73106092513143));
#54692=CARTESIAN_POINT('Ctrl Pts',(14.8155500988184,0.441811570071688,3.55533039551599));
#54693=CARTESIAN_POINT('Ctrl Pts',(14.7996448201308,0.256852791367914,3.42820006631018));
#54694=CARTESIAN_POINT('Ctrl Pts',(14.7837395414432,0.0608904496539635,
3.40804280624462));
#54695=CARTESIAN_POINT('Ctrl Pts',(14.7678342627556,-0.135071892059981,
3.38788554617906));
#54696=CARTESIAN_POINT('Ctrl Pts',(14.751928984068,-0.342037796784102,3.47470135525375));
#54697=CARTESIAN_POINT('Ctrl Pts',(14.7360237053804,-0.464977277074429,
3.62862808681558));
#54698=CARTESIAN_POINT('Ctrl Pts',(14.7201184266927,-0.587916757364756,
3.78255481837741));
#54699=CARTESIAN_POINT('Ctrl Pts',(14.7042131480052,-0.62682981322129,4.00359247242638));
#54700=CARTESIAN_POINT('Ctrl Pts',(14.6883078693175,-0.56384921567034,4.19024990955517));
#54701=CARTESIAN_POINT('Ctrl Pts',(14.6724025906299,-0.500868618119389,
4.37690734668397));
#54702=CARTESIAN_POINT('Ctrl Pts',(14.6564973119423,-0.335994367160947,
4.52918456689258));
#54703=CARTESIAN_POINT('Ctrl Pts',(14.6405920332547,-0.144929743580805,
4.57716231297912));
#54704=CARTESIAN_POINT('Ctrl Pts',(14.636676492589,-0.097893704910838,4.5889734116427));
#54705=CARTESIAN_POINT('Ctrl Pts',(14.6327609519233,-0.0492704262804658,
4.59446355048005));
#54706=CARTESIAN_POINT('Ctrl Pts',(14.6288454112575,-0.000548182068839831,
4.59401855345973));
#54707=CARTESIAN_POINT('Ctrl Pts',(14.5211545887425,1.28950532977596E-5,
4.59311636453746));
#54708=CARTESIAN_POINT('Ctrl Pts',(14.5291696491241,-0.100103612291989,
4.59309704959697));
#54709=CARTESIAN_POINT('Ctrl Pts',(14.5371847095056,-0.200228812305367,
4.56910822985942));
#54710=CARTESIAN_POINT('Ctrl Pts',(14.5451997698872,-0.287175610734119,
4.52120162576233));
#54711=CARTESIAN_POINT('Ctrl Pts',(14.5611050485748,-0.459714929737158,
4.42613460781534));
#54712=CARTESIAN_POINT('Ctrl Pts',(14.5770103272624,-0.580358509003398,
4.23688081735026));
#54713=CARTESIAN_POINT('Ctrl Pts',(14.59291560595,-0.593711920942704,4.04033758828107));
#54714=CARTESIAN_POINT('Ctrl Pts',(14.6088208846377,-0.607065332882009,
3.84379435921188));
#54715=CARTESIAN_POINT('Ctrl Pts',(14.6247261633253,-0.513128577494387,
3.63996169153858));
#54716=CARTESIAN_POINT('Ctrl Pts',(14.6406314420129,-0.35503343871745,3.52243092280774));
#54717=CARTESIAN_POINT('Ctrl Pts',(14.6565367207005,-0.196938299940509,
3.40490015407689));
#54718=CARTESIAN_POINT('Ctrl Pts',(14.6724419993881,0.025315222225754,3.37367128428849));
#54719=CARTESIAN_POINT('Ctrl Pts',(14.6883472780757,0.209677713173688,3.44308328926485));
#54720=CARTESIAN_POINT('Ctrl Pts',(14.7042525567633,0.394040204121622,3.51249529424121));
#54721=CARTESIAN_POINT('Ctrl Pts',(14.720157835451,0.540511663851219,3.68254817398232));
#54722=CARTESIAN_POINT('Ctrl Pts',(14.7360631141386,0.581838594751101,3.87516084045512));
#54723=CARTESIAN_POINT('Ctrl Pts',(14.7519683928262,0.623165525650983,4.06777350692792));
#54724=CARTESIAN_POINT('Ctrl Pts',(14.7678736715138,0.559347927721136,4.2829459601324));
#54725=CARTESIAN_POINT('Ctrl Pts',(14.7837789502014,0.419688142031033,4.42188011275284));
#54726=CARTESIAN_POINT('Ctrl Pts',(14.7962374963817,0.310293146587505,4.53070672248707));
#54727=CARTESIAN_POINT('Ctrl Pts',(14.8086960425621,0.154364940471616,4.59275708529138));
#54728=CARTESIAN_POINT('Ctrl Pts',(14.8211545887425,-0.000542004001680995,
4.59419620878869));
#54729=CARTESIAN_POINT('Origin',(4.,0.,4.));
#54730=CARTESIAN_POINT('',(15.2288454112576,0.000471544078774977,4.59356550157774));
#54731=CARTESIAN_POINT('',(15.1211545887425,0.000250233060073018,4.59495282954609));
#54732=CARTESIAN_POINT('',(4.,-7.27562663373442E-17,4.5941));
#54733=CARTESIAN_POINT('Ctrl Pts',(15.2288454112576,0.000471544078774977,
4.59356550157774));
#54734=CARTESIAN_POINT('Ctrl Pts',(15.2236242961746,0.0655651715058866,
4.59404721416646));
#54735=CARTESIAN_POINT('Ctrl Pts',(15.2184031810917,0.130516835945995,4.58418155789741));
#54736=CARTESIAN_POINT('Ctrl Pts',(15.2131820660088,0.191734887706884,4.56334598510492));
#54737=CARTESIAN_POINT('Ctrl Pts',(15.1972767873211,0.378225734681762,4.49987379829874));
#54738=CARTESIAN_POINT('Ctrl Pts',(15.1813715086335,0.530068013118856,4.33459889729257));
#54739=CARTESIAN_POINT('Ctrl Pts',(15.1654662299459,0.577542172676889,4.143408524424));
#54740=CARTESIAN_POINT('Ctrl Pts',(15.1495609512583,0.625016332234921,3.95221815155542));
#54741=CARTESIAN_POINT('Ctrl Pts',(15.1336556725707,0.568122372913892,3.73511230682445));
#54742=CARTESIAN_POINT('Ctrl Pts',(15.1177503938831,0.432983593849097,3.59177680914072));
#54743=CARTESIAN_POINT('Ctrl Pts',(15.1018451151955,0.297844814784303,3.44844131145699));
#54744=CARTESIAN_POINT('Ctrl Pts',(15.0859398365078,0.0844612159757424,
3.37887616082051));
#54745=CARTESIAN_POINT('Ctrl Pts',(15.0700345578202,-0.109190481519281,
3.41502273134472));
#54746=CARTESIAN_POINT('Ctrl Pts',(15.0541292791326,-0.302842179014298,
3.45116930186893));
#54747=CARTESIAN_POINT('Ctrl Pts',(15.038224000445,-0.47676197519578,3.59302759355383));
#54748=CARTESIAN_POINT('Ctrl Pts',(15.0223187217574,-0.551093257596978,
3.77546228038711));
#54749=CARTESIAN_POINT('Ctrl Pts',(15.0064134430698,-0.625424539998176,
3.95789696722038));
#54750=CARTESIAN_POINT('Ctrl Pts',(14.9905081643822,-0.600167308619091,
4.18090804920204));
#54751=CARTESIAN_POINT('Ctrl Pts',(14.9746028856946,-0.486918615563658,
4.34209827230691));
#54752=CARTESIAN_POINT('Ctrl Pts',(14.9593503942156,-0.378317895025423,
4.49667289829699));
#54753=CARTESIAN_POINT('Ctrl Pts',(14.9440979027365,-0.188800216398263,
4.59439705548643));
#54754=CARTESIAN_POINT('Ctrl Pts',(14.9288454112575,0.000149915246051877,
4.59503491979621));
#54755=CARTESIAN_POINT('Ctrl Pts',(14.8211545887425,-0.000542004001680995,
4.59419620878869));
#54756=CARTESIAN_POINT('Ctrl Pts',(14.8246013212497,-0.0433979515083632,
4.5945943510493));
#54757=CARTESIAN_POINT('Ctrl Pts',(14.828048053757,-0.0861757330942537,
4.59035339483295));
#54758=CARTESIAN_POINT('Ctrl Pts',(14.8314947862642,-0.127868389248254,
4.58118038604969));
#54759=CARTESIAN_POINT('Ctrl Pts',(14.8474000649518,-0.320263161387096,
4.5388506546897));
#54760=CARTESIAN_POINT('Ctrl Pts',(14.8633053436395,-0.489550732214419,
4.39149533993331));
#54761=CARTESIAN_POINT('Ctrl Pts',(14.8792106223271,-0.558001411172811,
4.20677376822741));
#54762=CARTESIAN_POINT('Ctrl Pts',(14.8951159010147,-0.6264520901312,4.0220521965215));
#54763=CARTESIAN_POINT('Ctrl Pts',(14.9110211797023,-0.594065877220663,
3.79996436786608));
#54764=CARTESIAN_POINT('Ctrl Pts',(14.9269264583899,-0.475713151262041,
3.64248361741852));
#54765=CARTESIAN_POINT('Ctrl Pts',(14.9428317370775,-0.357360425303418,
3.48500286697096));
#54766=CARTESIAN_POINT('Ctrl Pts',(14.9587370157651,-0.153041186296697,
3.39212919473125));
#54767=CARTESIAN_POINT('Ctrl Pts',(14.9746422944528,0.0434298152403689,
3.40650626183085));
#54768=CARTESIAN_POINT('Ctrl Pts',(14.9905475731404,0.239900816777435,3.42088332893044));
#54769=CARTESIAN_POINT('Ctrl Pts',(15.006452851828,0.428523580844854,3.54251113536931));
#54770=CARTESIAN_POINT('Ctrl Pts',(15.0223581305156,0.522690514153935,3.71554333807889));
#54771=CARTESIAN_POINT('Ctrl Pts',(15.0382634092032,0.616857447463019,3.88857554078846));
#54772=CARTESIAN_POINT('Ctrl Pts',(15.0541686878908,0.616568550013756,4.11301213976874));
#54773=CARTESIAN_POINT('Ctrl Pts',(15.0700739665784,0.521956471292605,4.28580134389743));
#54774=CARTESIAN_POINT('Ctrl Pts',(15.085979245266,0.427344392571456,4.45859054802613));
#54775=CARTESIAN_POINT('Ctrl Pts',(15.1018845239536,0.238409132578427,4.57973235730324));
#54776=CARTESIAN_POINT('Ctrl Pts',(15.1177898026413,0.0419017695106382,
4.59360357799603));
#54777=CARTESIAN_POINT('Ctrl Pts',(15.1189113980083,0.0280446248267054,
4.59458173733358));
#54778=CARTESIAN_POINT('Ctrl Pts',(15.1200329933754,0.0141498265549413,
4.59502647517791));
#54779=CARTESIAN_POINT('Ctrl Pts',(15.1211545887425,0.000250233060073018,
4.59495282954609));
#54780=CARTESIAN_POINT('Origin',(4.,0.,4.));
#54781=CARTESIAN_POINT('',(15.5288454112575,-0.000350670266729247,4.59332700645389));
#54782=CARTESIAN_POINT('',(15.4211545887425,0.000414092275955974,4.59343115273787));
#54783=CARTESIAN_POINT('',(4.,-7.27562663373442E-17,4.5941));
#54784=CARTESIAN_POINT('Ctrl Pts',(15.5288454112575,-0.000350670266729247,
4.59332700645389));
#54785=CARTESIAN_POINT('Ctrl Pts',(15.5190559683003,0.121821298278883,4.59267222728074));
#54786=CARTESIAN_POINT('Ctrl Pts',(15.509266525343,0.244354036528086,4.55597946496206));
#54787=CARTESIAN_POINT('Ctrl Pts',(15.4994770823858,0.343380025451582,4.48601555964668));
#54788=CARTESIAN_POINT('Ctrl Pts',(15.4835718036982,0.504271299656008,4.37234255322809));
#54789=CARTESIAN_POINT('Ctrl Pts',(15.4676665250105,0.603110088323456,4.17084127710728));
#54790=CARTESIAN_POINT('Ctrl Pts',(15.4517612463229,0.594513801222153,3.97403259246294));
#54791=CARTESIAN_POINT('Ctrl Pts',(15.4358559676353,0.58591751412085,3.7772239078186));
#54792=CARTESIAN_POINT('Ctrl Pts',(15.4199506889477,0.469886151250777,3.58510781465072));
#54793=CARTESIAN_POINT('Ctrl Pts',(15.4040454102601,0.299696405559752,3.48589589518039));
#54794=CARTESIAN_POINT('Ctrl Pts',(15.3881401315725,0.129506659868722,3.38668397571006));
#54795=CARTESIAN_POINT('Ctrl Pts',(15.3722348528849,-0.0948414686432761,
3.38037622993726));
#54796=CARTESIAN_POINT('Ctrl Pts',(15.3563295741973,-0.270336810750117,
3.46986890786216));
#54797=CARTESIAN_POINT('Ctrl Pts',(15.3404242955096,-0.445832152856957,
3.55936158578705));
#54798=CARTESIAN_POINT('Ctrl Pts',(15.324519016822,-0.572474708558633,3.74465468740961));
#54799=CARTESIAN_POINT('Ctrl Pts',(15.3086137381344,-0.592115574081638,
3.94066945956945));
#54800=CARTESIAN_POINT('Ctrl Pts',(15.2927084594468,-0.611756439604643,
4.13668423172929));
#54801=CARTESIAN_POINT('Ctrl Pts',(15.2768031807592,-0.524395614948954,
4.3434206744264));
#54802=CARTESIAN_POINT('Ctrl Pts',(15.2608979020716,-0.370145494864779,
4.46595415947185));
#54803=CARTESIAN_POINT('Ctrl Pts',(15.2502137384669,-0.266529987624151,
4.54826443060822));
#54804=CARTESIAN_POINT('Ctrl Pts',(15.2395295748622,-0.13273198696893,4.59257975504152));
#54805=CARTESIAN_POINT('Ctrl Pts',(15.2288454112576,0.000471544078774977,
4.59356550157774));
#54806=CARTESIAN_POINT('Ctrl Pts',(15.1211545887425,0.000250233060073018,
4.59495282954609));
#54807=CARTESIAN_POINT('Ctrl Pts',(15.135938272063,-0.18295950063263,4.59398211075496));
#54808=CARTESIAN_POINT('Ctrl Pts',(15.1507219553836,-0.367002343096231,
4.50294888365168));
#54809=CARTESIAN_POINT('Ctrl Pts',(15.1655056387041,-0.476631971954554,
4.35629051265579));
#54810=CARTESIAN_POINT('Ctrl Pts',(15.1814109173917,-0.594578884209397,
4.19850559451431));
#54811=CARTESIAN_POINT('Ctrl Pts',(15.1973161960793,-0.626393242576541,
3.97633512612291));
#54812=CARTESIAN_POINT('Ctrl Pts',(15.2132214747669,-0.557467239648298,
3.79179038730953));
#54813=CARTESIAN_POINT('Ctrl Pts',(15.2291267534545,-0.488541236720055,
3.60724564849615));
#54814=CARTESIAN_POINT('Ctrl Pts',(15.2450320321422,-0.318874872496425,
3.46032663926078));
#54815=CARTESIAN_POINT('Ctrl Pts',(15.2609373108298,-0.126371763436977,
3.41849235301362));
#54816=CARTESIAN_POINT('Ctrl Pts',(15.2768425895174,0.0661313456224706,
3.37665806676646));
#54817=CARTESIAN_POINT('Ctrl Pts',(15.292747868205,0.281471199517752,3.4399085035075));
#54818=CARTESIAN_POINT('Ctrl Pts',(15.3086531468926,0.420772847618048,3.57920173859056));
#54819=CARTESIAN_POINT('Ctrl Pts',(15.3245584255802,0.560074495718348,3.71849497367363));
#54820=CARTESIAN_POINT('Ctrl Pts',(15.3404637042678,0.623337938023671,3.9338310070987));
#54821=CARTESIAN_POINT('Ctrl Pts',(15.3563689829554,0.581515278282945,4.12633664243329));
#54822=CARTESIAN_POINT('Ctrl Pts',(15.3722742616431,0.53969261854222,4.31884227776789));
#54823=CARTESIAN_POINT('Ctrl Pts',(15.3881795403307,0.392783856755445,4.48851751501199));
#54824=CARTESIAN_POINT('Ctrl Pts',(15.4040848190183,0.208243281137944,4.55745466359042));
#54825=CARTESIAN_POINT('Ctrl Pts',(15.4097747422597,0.142226097106806,4.58211610408423));
#54826=CARTESIAN_POINT('Ctrl Pts',(15.4154646655011,0.0713929250243718,
4.593885435962));
#54827=CARTESIAN_POINT('Ctrl Pts',(15.4211545887425,0.000414092275955974,
4.59343115273787));
#54828=CARTESIAN_POINT('Origin',(4.,0.,4.));
#54829=CARTESIAN_POINT('',(15.8288454112575,-0.000332254705457391,4.59484959654372));
#54830=CARTESIAN_POINT('',(15.7211545887425,-0.000419917270904514,4.59344262983929));
#54831=CARTESIAN_POINT('',(4.,-7.27562663373442E-17,4.5941));
#54832=CARTESIAN_POINT('Ctrl Pts',(15.8288454112575,-0.000332254705457391,
4.59484959654372));
#54833=CARTESIAN_POINT('Ctrl Pts',(15.814487640426,0.177680873019276,4.5936575613883));
#54834=CARTESIAN_POINT('Ctrl Pts',(15.8001298695944,0.356683508224643,4.50844978272675));
#54835=CARTESIAN_POINT('Ctrl Pts',(15.7857720987628,0.466927807092597,4.36891650689757));
#54836=CARTESIAN_POINT('Ctrl Pts',(15.7698668200752,0.589054446233417,4.21434406913608));
#54837=CARTESIAN_POINT('Ctrl Pts',(15.7539615413876,0.626802179063893,3.99310442736787));
#54838=CARTESIAN_POINT('Ctrl Pts',(15.7380562627,0.562838843643149,3.80678146521555));
#54839=CARTESIAN_POINT('Ctrl Pts',(15.7221509840123,0.498875508222402,3.62045850306322));
#54840=CARTESIAN_POINT('Ctrl Pts',(15.7062457053247,0.333201104550436,3.46905222052678));
#54841=CARTESIAN_POINT('Ctrl Pts',(15.6903404266371,0.141886309687413,3.42208197707538));
#54842=CARTESIAN_POINT('Ctrl Pts',(15.6744351479495,-0.0494284851756215,
3.37511173362399));
#54843=CARTESIAN_POINT('Ctrl Pts',(15.6585298692619,-0.266383671229707,
3.43257752925765));
#54844=CARTESIAN_POINT('Ctrl Pts',(15.6426245905743,-0.409362605655794,
3.5680935017987));
#54845=CARTESIAN_POINT('Ctrl Pts',(15.6267193118867,-0.552341540081869,
3.70360947433975));
#54846=CARTESIAN_POINT('Ctrl Pts',(15.6108140331991,-0.621344222879956,
3.9171756237882));
#54847=CARTESIAN_POINT('Ctrl Pts',(15.5949087545115,-0.584687541371933,
4.11073140955597));
#54848=CARTESIAN_POINT('Ctrl Pts',(15.5790034758238,-0.548030859863907,
4.30428719532377));
#54849=CARTESIAN_POINT('Ctrl Pts',(15.5630981971362,-0.405714814049763,
4.47783261741089));
#54850=CARTESIAN_POINT('Ctrl Pts',(15.5471929184486,-0.223084911271984,
4.55168296009627));
#54851=CARTESIAN_POINT('Ctrl Pts',(15.5410770827183,-0.152860773312716,
4.58007960584922));
#54852=CARTESIAN_POINT('Ctrl Pts',(15.5349612469879,-0.0766761255292402,
4.5937360717991));
#54853=CARTESIAN_POINT('Ctrl Pts',(15.5288454112575,-0.000350670266729247,
4.59332700645389));
#54854=CARTESIAN_POINT('Ctrl Pts',(15.4211545887425,0.000414092275955974,
4.59343115273787));
#54855=CARTESIAN_POINT('Ctrl Pts',(15.4313699441887,-0.12701715326484,4.59261555920332));
#54856=CARTESIAN_POINT('Ctrl Pts',(15.4415852996349,-0.254917899718674,
4.55240018390688));
#54857=CARTESIAN_POINT('Ctrl Pts',(15.4518006550811,-0.356261725310785,
4.47665348962993));
#54858=CARTESIAN_POINT('Ctrl Pts',(15.4677059337687,-0.514053766693778,
4.35871610717824));
#54859=CARTESIAN_POINT('Ctrl Pts',(15.4836112124564,-0.607465460011524,
4.15464228236211));
#54860=CARTESIAN_POINT('Ctrl Pts',(15.499516491144,-0.593606107615349,3.95813408188558));
#54861=CARTESIAN_POINT('Ctrl Pts',(15.5154217698316,-0.579746755219174,
3.76162588140906));
#54862=CARTESIAN_POINT('Ctrl Pts',(15.5313270485192,-0.458616357109098,
3.57268330527213));
#54863=CARTESIAN_POINT('Ctrl Pts',(15.5472323272068,-0.285832867492734,
3.47806079093568));
#54864=CARTESIAN_POINT('Ctrl Pts',(15.5631376058944,-0.113049377876356,
3.38343827659922));
#54865=CARTESIAN_POINT('Ctrl Pts',(15.579042884582,0.111387203246309,3.38313582406324));
#54866=CARTESIAN_POINT('Ctrl Pts',(15.5949481632696,0.284425092952457,3.47729230673655));
#54867=CARTESIAN_POINT('Ctrl Pts',(15.6108534419572,0.457462982658595,3.57144878940986));
#54868=CARTESIAN_POINT('Ctrl Pts',(15.6267587206449,0.579102180948212,3.76006420729246));
#54869=CARTESIAN_POINT('Ctrl Pts',(15.6426639993325,0.593491114096805,3.95653434015292));
#54870=CARTESIAN_POINT('Ctrl Pts',(15.6585692780201,0.607880047245398,4.15300447301339));
#54871=CARTESIAN_POINT('Ctrl Pts',(15.6744745567077,0.515018715252963,4.35732932085173));
#54872=CARTESIAN_POINT('Ctrl Pts',(15.6903798353953,0.357545113131455,4.47569155781202));
#54873=CARTESIAN_POINT('Ctrl Pts',(15.700638086511,0.255981111243369,4.55203033647815));
#54874=CARTESIAN_POINT('Ctrl Pts',(15.7108963376268,0.127540214881222,4.59261107697802));
#54875=CARTESIAN_POINT('Ctrl Pts',(15.7211545887425,-0.000419917270904514,
4.59344262983929));
#54876=CARTESIAN_POINT('Origin',(4.,0.,4.));
#54877=CARTESIAN_POINT('',(16.1288454112575,0.000520203518568921,4.59435747030618));
#54878=CARTESIAN_POINT('',(16.0211545887425,-0.00024144267326323,4.59496181546483));
#54879=CARTESIAN_POINT('',(4.,-7.27562663373442E-17,4.5941));
#54880=CARTESIAN_POINT('Ctrl Pts',(16.1288454112575,0.000520203518568921,
4.59435747030618));
#54881=CARTESIAN_POINT('Ctrl Pts',(16.1258245912393,0.0380542554257849,
4.59470210862833));
#54882=CARTESIAN_POINT('Ctrl Pts',(16.122803771221,0.0755288363057283,4.59145263304759));
#54883=CARTESIAN_POINT('Ctrl Pts',(16.1197829512027,0.112271568866026,4.58439375503351));
#54884=CARTESIAN_POINT('Ctrl Pts',(16.1038776725151,0.305730099191281,4.54722721702202));
#54885=CARTESIAN_POINT('Ctrl Pts',(16.0879723938275,0.478899942385972,4.40445440507416));
#54886=CARTESIAN_POINT('Ctrl Pts',(16.0720671151398,0.55226883266698,4.22163055421683));
#54887=CARTESIAN_POINT('Ctrl Pts',(16.0561618364522,0.625637722947984,4.03880670335952));
#54888=CARTESIAN_POINT('Ctrl Pts',(16.0402565577646,0.599205660315318,3.81593181359275));
#54889=CARTESIAN_POINT('Ctrl Pts',(16.024351279077,0.485109129681553,3.65534060523843));
#54890=CARTESIAN_POINT('Ctrl Pts',(16.0084460003894,0.371012599047788,3.4947493968841));
#54891=CARTESIAN_POINT('Ctrl Pts',(15.9925407217018,0.169251600412921,3.39644186994223));
#54892=CARTESIAN_POINT('Ctrl Pts',(15.9766354430142,-0.0275337514538456,
3.40555668173602));
#54893=CARTESIAN_POINT('Ctrl Pts',(15.9607301643265,-0.224319103320618,
3.41467149352982));
#54894=CARTESIAN_POINT('Ctrl Pts',(15.9448248856389,-0.416128808419276,
3.53120864405929));
#54895=CARTESIAN_POINT('Ctrl Pts',(15.9289196069513,-0.514891964967956,
3.70165920408156));
#54896=CARTESIAN_POINT('Ctrl Pts',(15.9130143282637,-0.613655121516638,
3.87210976410384));
#54897=CARTESIAN_POINT('Ctrl Pts',(15.8971090495761,-0.619371729515322,
4.09647373361892));
#54898=CARTESIAN_POINT('Ctrl Pts',(15.8812037708885,-0.52941696442075,4.27173266988224));
#54899=CARTESIAN_POINT('Ctrl Pts',(15.8652984922009,-0.439462199326184,
4.44699160614554));
#54900=CARTESIAN_POINT('Ctrl Pts',(15.8493932135132,-0.25383606113837,4.57314550915708));
#54901=CARTESIAN_POINT('Ctrl Pts',(15.8334879348256,-0.0577702193188812,
4.59226984378546));
#54902=CARTESIAN_POINT('Ctrl Pts',(15.8319404269696,-0.0386939468137543,
4.59413055045147));
#54903=CARTESIAN_POINT('Ctrl Pts',(15.8303929191136,-0.0195188482833839,
4.59497807636063));
#54904=CARTESIAN_POINT('Ctrl Pts',(15.8288454112575,-0.000332254705457391,
4.59484959654372));
#54905=CARTESIAN_POINT('Ctrl Pts',(15.7211545887425,-0.000419917270904514,
4.59344262983929));
#54906=CARTESIAN_POINT('Ctrl Pts',(15.7268016163144,-0.0708602278282204,
4.59390038836772));
#54907=CARTESIAN_POINT('Ctrl Pts',(15.7324486438863,-0.141154849878182,
4.58231274148771));
#54908=CARTESIAN_POINT('Ctrl Pts',(15.7380956714582,-0.206740066761224,
4.55801389847688));
#54909=CARTESIAN_POINT('Ctrl Pts',(15.7540009501458,-0.391465772281827,
4.48957437609924));
#54910=CARTESIAN_POINT('Ctrl Pts',(15.7699062288334,-0.538831311072463,
4.32029570526172));
#54911=CARTESIAN_POINT('Ctrl Pts',(15.785811507521,-0.58117266224226,4.12790349002296));
#54912=CARTESIAN_POINT('Ctrl Pts',(15.8017167862086,-0.62351401341206,3.93551127478418));
#54913=CARTESIAN_POINT('Ctrl Pts',(15.8176220648962,-0.560831176961022,
3.72000551514415));
#54914=CARTESIAN_POINT('Ctrl Pts',(15.8335273435838,-0.421905459495345,
3.58033733863277));
#54915=CARTESIAN_POINT('Ctrl Pts',(15.8494326222715,-0.282979742029676,
3.44066916212139));
#54916=CARTESIAN_POINT('Ctrl Pts',(15.8653379009591,-0.0678111435493865,
3.37683856873865));
#54917=CARTESIAN_POINT('Ctrl Pts',(15.8812431796467,0.124804018556085,3.41815386651619));
#54918=CARTESIAN_POINT('Ctrl Pts',(15.8971484583343,0.317419180661557,3.45946916429373));
#54919=CARTESIAN_POINT('Ctrl Pts',(15.9130537370219,0.487480906392202,3.60593035323155));
#54920=CARTESIAN_POINT('Ctrl Pts',(15.9289590157095,0.556904046010802,3.79028865163133));
#54921=CARTESIAN_POINT('Ctrl Pts',(15.9448642943971,0.6263271856294,3.9746469500311));
#54922=CARTESIAN_POINT('Ctrl Pts',(15.9607695730847,0.595111739135951,4.19690235789283));
#54923=CARTESIAN_POINT('Ctrl Pts',(15.9766748517723,0.477590518943614,4.35500459477727));
#54924=CARTESIAN_POINT('Ctrl Pts',(15.9915014307624,0.368039615220995,4.50238430120742));
#54925=CARTESIAN_POINT('Ctrl Pts',(16.0063280097524,0.18349252241573,4.59401752470064));
#54926=CARTESIAN_POINT('Ctrl Pts',(16.0211545887425,-0.00024144267326323,
4.59496181546483));
#54927=CARTESIAN_POINT('Origin',(4.,0.,4.));
#54928=CARTESIAN_POINT('',(16.4288454112575,7.48704377684928E-5,4.59312461313858));
#54929=CARTESIAN_POINT('',(16.3211545887425,0.000543344619121817,4.59417988242975));
#54930=CARTESIAN_POINT('',(4.,-7.27562663373442E-17,4.5941));
#54931=CARTESIAN_POINT('Ctrl Pts',(16.4288454112575,7.48704377684928E-5,
4.59312461313858));
#54932=CARTESIAN_POINT('Ctrl Pts',(16.4212562633649,0.0948679978941589,
4.5932308806522));
#54933=CARTESIAN_POINT('Ctrl Pts',(16.4136671154723,0.189615837117123,4.57184094704105));
#54934=CARTESIAN_POINT('Ctrl Pts',(16.4060779675797,0.273126642574496,4.52869916135151));
#54935=CARTESIAN_POINT('Ctrl Pts',(16.3901726888921,0.448147956300534,4.43828293357696));
#54936=CARTESIAN_POINT('Ctrl Pts',(16.3742674102045,0.573812330828296,4.25232504748949));
#54937=CARTESIAN_POINT('Ctrl Pts',(16.3583621315169,0.592420001795879,4.05620949715111));
#54938=CARTESIAN_POINT('Ctrl Pts',(16.3424568528292,0.611027672763462,3.86009394681272));
#54939=CARTESIAN_POINT('Ctrl Pts',(16.3265515741416,0.522578640170867,3.6538207322234));
#54940=CARTESIAN_POINT('Ctrl Pts',(16.310646295454,0.367684957814641,3.53210178682255));
#54941=CARTESIAN_POINT('Ctrl Pts',(16.2947410167664,0.212791275458425,3.4103828414217));
#54942=CARTESIAN_POINT('Ctrl Pts',(16.2788357380788,-0.00854705666138705,
3.3732181652093));
#54943=CARTESIAN_POINT('Ctrl Pts',(16.2629304593912,-0.19470084048803,3.43767220519428));
#54944=CARTESIAN_POINT('Ctrl Pts',(16.2470251807036,-0.380854624314662,
3.50212624517926));
#54945=CARTESIAN_POINT('Ctrl Pts',(16.231119902016,-0.531823859848111,3.66819900136163));
#54946=CARTESIAN_POINT('Ctrl Pts',(16.2152146233283,-0.578289861113055,
3.85963689006134));
#54947=CARTESIAN_POINT('Ctrl Pts',(16.1993093446407,-0.624755862378002,
4.05107477876107));
#54948=CARTESIAN_POINT('Ctrl Pts',(16.1834040659531,-0.566718629374431,
4.26787779997815));
#54949=CARTESIAN_POINT('Ctrl Pts',(16.1674987872655,-0.430826404144746,
4.41049917854914));
#54950=CARTESIAN_POINT('Ctrl Pts',(16.1546143285962,-0.320743594918802,
4.52603310245269));
#54951=CARTESIAN_POINT('Ctrl Pts',(16.1417298699269,-0.159570744489656,
4.592887512417));
#54952=CARTESIAN_POINT('Ctrl Pts',(16.1288454112575,0.000520203518568921,
4.59435747030618));
#54953=CARTESIAN_POINT('Ctrl Pts',(16.0211545887425,-0.00024144267326323,
4.59496181546483));
#54954=CARTESIAN_POINT('Ctrl Pts',(16.0222332884401,-0.0136089074611732,
4.59503051682625));
#54955=CARTESIAN_POINT('Ctrl Pts',(16.0233119881376,-0.0269720681925484,
4.59461918253551));
#54956=CARTESIAN_POINT('Ctrl Pts',(16.0243906878352,-0.0403017303441999,
4.59371435609144));
#54957=CARTESIAN_POINT('Ctrl Pts',(16.0402959665228,-0.236845765548457,
4.58037281461397));
#54958=CARTESIAN_POINT('Ctrl Pts',(16.0562012452104,-0.426106842065734,
4.45974066575184));
#54959=CARTESIAN_POINT('Ctrl Pts',(16.072106523898,-0.521184280535122,4.2872070887372));
#54960=CARTESIAN_POINT('Ctrl Pts',(16.0880118025856,-0.616261719004504,
4.11467351172257));
#54961=CARTESIAN_POINT('Ctrl Pts',(16.1039170812732,-0.61715551942601,3.89023850655542));
#54962=CARTESIAN_POINT('Ctrl Pts',(16.1198223599609,-0.523455286459661,
3.71695313254649));
#54963=CARTESIAN_POINT('Ctrl Pts',(16.1357276386485,-0.429755053493313,
3.54366775853756));
#54964=CARTESIAN_POINT('Ctrl Pts',(16.1516329173361,-0.241460787139106,
3.42153201568684));
#54965=CARTESIAN_POINT('Ctrl Pts',(16.1675381960237,-0.045029248433429,
3.40662546997421));
#54966=CARTESIAN_POINT('Ctrl Pts',(16.1834434747113,0.151402290272254,3.39171892426158));
#54967=CARTESIAN_POINT('Ctrl Pts',(16.1993487533989,0.355971101329402,3.48404157568705));
#54968=CARTESIAN_POINT('Ctrl Pts',(16.2152540320865,0.474747841293266,3.64120276856532));
#54969=CARTESIAN_POINT('Ctrl Pts',(16.2311593107741,0.593524581257127,3.79836396144359));
#54970=CARTESIAN_POINT('Ctrl Pts',(16.2470645894618,0.626509250127697,4.02036369577466));
#54971=CARTESIAN_POINT('Ctrl Pts',(16.2629698681494,0.558556683425868,4.20526908558792));
#54972=CARTESIAN_POINT('Ctrl Pts',(16.278875146837,0.490604116724039,4.39017447540119));
#54973=CARTESIAN_POINT('Ctrl Pts',(16.2947804255246,0.32171431444981,4.53798552069667));
#54974=CARTESIAN_POINT('Ctrl Pts',(16.3106857042122,0.129434328669215,4.58083364284428));
#54975=CARTESIAN_POINT('Ctrl Pts',(16.314175332389,0.0872479785030607,4.5902345478711));
#54976=CARTESIAN_POINT('Ctrl Pts',(16.3176649605657,0.0439357035691123,
4.5945828907904));
#54977=CARTESIAN_POINT('Ctrl Pts',(16.3211545887425,0.000543344619121817,
4.59417988242975));
#54978=CARTESIAN_POINT('Origin',(4.,0.,4.));
#54979=CARTESIAN_POINT('',(16.7288454112575,-0.000548108868865471,4.59408180714414));
#54980=CARTESIAN_POINT('',(16.6211545887425,-2.1752937549985E-5,4.5931168278739));
#54981=CARTESIAN_POINT('',(4.,-7.27562663373442E-17,4.5941));
#54982=CARTESIAN_POINT('Ctrl Pts',(16.7288454112575,-0.000548108868865471,
4.59408180714414));
#54983=CARTESIAN_POINT('Ctrl Pts',(16.7166879354906,0.15068989439403,4.59268722311157));
#54984=CARTESIAN_POINT('Ctrl Pts',(16.7045304597237,0.302891836883802,4.53390177381835));
#54985=CARTESIAN_POINT('Ctrl Pts',(16.6923729839567,0.411632901649024,4.42974331917764));
#54986=CARTESIAN_POINT('Ctrl Pts',(16.6764677052691,0.553895734249677,4.29347578465895));
#54987=CARTESIAN_POINT('Ctrl Pts',(16.6605624265815,0.621772048174623,4.07954898308531));
#54988=CARTESIAN_POINT('Ctrl Pts',(16.6446571478939,0.58409591167956,3.88618905124272));
#54989=CARTESIAN_POINT('Ctrl Pts',(16.6287518692063,0.546419775184499,3.69282911940014));
#54990=CARTESIAN_POINT('Ctrl Pts',(16.6128465905187,0.403191188269443,3.52003605728863));
#54991=CARTESIAN_POINT('Ctrl Pts',(16.596941311831,0.220174658543969,3.44714912875817));
#54992=CARTESIAN_POINT('Ctrl Pts',(16.5810360331434,0.0371581288184754,
3.37426220022769));
#54993=CARTESIAN_POINT('Ctrl Pts',(16.5651307544558,-0.185646343717467,
3.40128140527831));
#54994=CARTESIAN_POINT('Ctrl Pts',(16.5492254757682,-0.34593637135519,3.51580066803907));
#54995=CARTESIAN_POINT('Ctrl Pts',(16.5333201970806,-0.506226398992903,
3.63031993079982));
#54996=CARTESIAN_POINT('Ctrl Pts',(16.517414918393,-0.604001981732426,3.83233925127069));
#54997=CARTESIAN_POINT('Ctrl Pts',(16.5015096397054,-0.594368708523554,
4.02909990422408));
#54998=CARTESIAN_POINT('Ctrl Pts',(16.4856043610178,-0.584735435314682,
4.22586055717748));
#54999=CARTESIAN_POINT('Ctrl Pts',(16.4696990823301,-0.467693306157413,
4.4173625426134));
#55000=CARTESIAN_POINT('Ctrl Pts',(16.4537938036425,-0.296983115116624,
4.51567625060054));
#55001=CARTESIAN_POINT('Ctrl Pts',(16.4454776728475,-0.20772669247752,4.56707991793767));
#55002=CARTESIAN_POINT('Ctrl Pts',(16.4371615420525,-0.103798720846626,
4.59300816600183));
#55003=CARTESIAN_POINT('Ctrl Pts',(16.4288454112575,7.48704377684928E-5,
4.59312461313858));
#55004=CARTESIAN_POINT('Ctrl Pts',(16.3211545887425,0.000543344619121817,
4.59417988242975));
#55005=CARTESIAN_POINT('Ctrl Pts',(16.3335702392533,-0.153841115924154,
4.59274603025257));
#55006=CARTESIAN_POINT('Ctrl Pts',(16.3459858897642,-0.309239316255332,
4.53116741914846));
#55007=CARTESIAN_POINT('Ctrl Pts',(16.3584015402751,-0.418549561707542,
4.42300972860235));
#55008=CARTESIAN_POINT('Ctrl Pts',(16.3743068189627,-0.558583297016706,
4.28445249321304));
#55009=CARTESIAN_POINT('Ctrl Pts',(16.3902120976503,-0.622980598348072,
4.06945282343469));
#55010=CARTESIAN_POINT('Ctrl Pts',(16.4061173763379,-0.582172949355422,
3.87672947174358));
#55011=CARTESIAN_POINT('Ctrl Pts',(16.4220226550255,-0.541365300362771,
3.68400612005246));
#55012=CARTESIAN_POINT('Ctrl Pts',(16.4379279337131,-0.395352701046104,
3.5135590864486));
#55013=CARTESIAN_POINT('Ctrl Pts',(16.4538332124007,-0.211177959727979,
3.44365043774355));
#55014=CARTESIAN_POINT('Ctrl Pts',(16.4697384910883,-0.0270032184098532,
3.37374178903851));
#55015=CARTESIAN_POINT('Ctrl Pts',(16.485643769776,0.195333664909731,3.40437152523229));
#55016=CARTESIAN_POINT('Ctrl Pts',(16.5015490484636,0.353744999708243,3.52147576730199));
#55017=CARTESIAN_POINT('Ctrl Pts',(16.5174543271512,0.512156334506764,3.63858000937169));
#55018=CARTESIAN_POINT('Ctrl Pts',(16.5333596058388,0.606642120784206,3.84215875731731));
#55019=CARTESIAN_POINT('Ctrl Pts',(16.5492648845264,0.59381848284593,4.03873726278877));
#55020=CARTESIAN_POINT('Ctrl Pts',(16.565170163214,0.580994844907655,4.23531576826023));
#55021=CARTESIAN_POINT('Ctrl Pts',(16.5810754419016,0.460861782753675,4.42489403125753));
#55022=CARTESIAN_POINT('Ctrl Pts',(16.5969807205892,0.288579316114369,4.52042573380721));
#55023=CARTESIAN_POINT('Ctrl Pts',(16.6050386766403,0.201297315476928,4.56882414767653));
#55024=CARTESIAN_POINT('Ctrl Pts',(16.6130966326914,0.100630370301649,4.59308406930439));
#55025=CARTESIAN_POINT('Ctrl Pts',(16.6211545887425,-2.1752937549985E-5,
4.5931168278739));
#55026=CARTESIAN_POINT('Origin',(4.,0.,4.));
#55027=CARTESIAN_POINT('',(17.0288454112575,0.000186802344652959,4.59500977980842));
#55028=CARTESIAN_POINT('',(16.9211545887425,-0.000535257393875686,4.59425998651214));
#55029=CARTESIAN_POINT('',(4.,-7.27562663373442E-17,4.5941));
#55030=CARTESIAN_POINT('Ctrl Pts',(17.0288454112575,0.000186802344652959,
4.59500977980842));
#55031=CARTESIAN_POINT('Ctrl Pts',(17.0280248863039,0.0103527338555297,
4.59505157132578));
#55032=CARTESIAN_POINT('Ctrl Pts',(17.0272043613502,0.0205166685362397,
4.5948136789481));
#55033=CARTESIAN_POINT('Ctrl Pts',(17.0263838363966,0.0306658549750798,
4.59428997251885));
#55034=CARTESIAN_POINT('Ctrl Pts',(17.010478557709,0.227400443050786,4.58413830477164));
#55035=CARTESIAN_POINT('Ctrl Pts',(16.9945732790214,0.418593379366704,4.46659200952389));
#55036=CARTESIAN_POINT('Ctrl Pts',(16.9786680003338,0.516456956272638,4.29562337257973));
#55037=CARTESIAN_POINT('Ctrl Pts',(16.9627627216462,0.614320533178566,4.12465473563558));
#55038=CARTESIAN_POINT('Ctrl Pts',(16.9468574429585,0.618854750674521,3.90026375699502));
#55039=CARTESIAN_POINT('Ctrl Pts',(16.9309521642709,0.527977687913284,3.72548128085037));
#55040=CARTESIAN_POINT('Ctrl Pts',(16.9150468855833,0.437100625152047,3.55069880470573));
#55041=CARTESIAN_POINT('Ctrl Pts',(16.8991416068957,0.25081228213362,3.42552483105699));
#55042=CARTESIAN_POINT('Ctrl Pts',(16.8832363282081,0.054648384762208,3.40743395292956));
#55043=CARTESIAN_POINT('Ctrl Pts',(16.8673310495205,-0.141515512609204,
3.38934307480212));
#55044=CARTESIAN_POINT('Ctrl Pts',(16.8514257708328,-0.347554964333599,
3.47833529219599));
#55045=CARTESIAN_POINT('Ctrl Pts',(16.8355204921452,-0.468865370989487,
3.63354914383413));
#55046=CARTESIAN_POINT('Ctrl Pts',(16.8196152134576,-0.590175777645383,
3.78876299547228));
#55047=CARTESIAN_POINT('Ctrl Pts',(16.80370993477,-0.62675713923276,4.01019848135471));
#55048=CARTESIAN_POINT('Ctrl Pts',(16.7878046560824,-0.561812842140477,
4.19618179452704));
#55049=CARTESIAN_POINT('Ctrl Pts',(16.7718993773948,-0.496868545048197,
4.38216510769936));
#55050=CARTESIAN_POINT('Ctrl Pts',(16.7559940987072,-0.330398589276266,
4.53269624816158));
#55051=CARTESIAN_POINT('Ctrl Pts',(16.7400888200196,-0.138838935752124,
4.57865768466082));
#55052=CARTESIAN_POINT('Ctrl Pts',(16.7363410170989,-0.0937012275068688,
4.58948769960953));
#55053=CARTESIAN_POINT('Ctrl Pts',(16.7325932141782,-0.0471704703862807,
4.59451171761327));
#55054=CARTESIAN_POINT('Ctrl Pts',(16.7288454112575,-0.000548108868865471,
4.59408180714414));
#55055=CARTESIAN_POINT('Ctrl Pts',(16.6211545887425,-2.1752937549985E-5,
4.5931168278739));
#55056=CARTESIAN_POINT('Ctrl Pts',(16.629001911379,-0.0980428491191961,
4.59314873014073));
#55057=CARTESIAN_POINT('Ctrl Pts',(16.6368492340155,-0.196049888122182,
4.57020350190738));
#55058=CARTESIAN_POINT('Ctrl Pts',(16.6446965566521,-0.281666676968544,
4.52419924569128));
#55059=CARTESIAN_POINT('Ctrl Pts',(16.6606018353397,-0.455198332287519,
4.43095591292362));
#55060=CARTESIAN_POINT('Ctrl Pts',(16.6765071140273,-0.577829771800838,
4.24298410528626));
#55061=CARTESIAN_POINT('Ctrl Pts',(16.6924123927149,-0.593253826592341,
4.0465925244149));
#55062=CARTESIAN_POINT('Ctrl Pts',(16.7083176714025,-0.608677881383846,
3.85020094354353));
#55063=CARTESIAN_POINT('Ctrl Pts',(16.7242229500901,-0.516894551453523,
3.64538958943816));
#55064=CARTESIAN_POINT('Ctrl Pts',(16.7401282287778,-0.360046858872914,
3.52619917105016));
#55065=CARTESIAN_POINT('Ctrl Pts',(16.7560335074654,-0.203199166292313,
3.40700875266216));
#55066=CARTESIAN_POINT('Ctrl Pts',(16.771938786153,0.0187128889385656,3.37343926999153));
#55067=CARTESIAN_POINT('Ctrl Pts',(16.7878440648406,0.203796679382533,3.44090440927292));
#55068=CARTESIAN_POINT('Ctrl Pts',(16.8037493435282,0.388880469826499,3.50836954855431));
#55069=CARTESIAN_POINT('Ctrl Pts',(16.8196546222158,0.537135995483554,3.67686930978772));
#55070=CARTESIAN_POINT('Ctrl Pts',(16.8355599009034,0.58049059114602,3.86903573125179));
#55071=CARTESIAN_POINT('Ctrl Pts',(16.851465179591,0.623845186808487,4.06120215271587));
#55072=CARTESIAN_POINT('Ctrl Pts',(16.8673704582787,0.562298852476364,4.2770352344106));
#55073=CARTESIAN_POINT('Ctrl Pts',(16.8832757369663,0.424111061064287,4.41743355636644));
#55074=CARTESIAN_POINT('Ctrl Pts',(16.8959020208917,0.314411738992559,4.5288876912157));
#55075=CARTESIAN_POINT('Ctrl Pts',(16.9085283048171,0.156414067554279,4.59280392009262));
#55076=CARTESIAN_POINT('Ctrl Pts',(16.9211545887425,-0.000535257393875686,
4.59425998651214));
#55077=CARTESIAN_POINT('Origin',(4.,0.,4.));
#55078=CARTESIAN_POINT('',(17.3288454112575,0.000452601584348983,4.59351524744837));
#55079=CARTESIAN_POINT('',(17.2211545887425,0.000283723793354941,4.5949151055343));
#55080=CARTESIAN_POINT('',(4.,-7.27562663373442E-17,4.5941));
#55081=CARTESIAN_POINT('Ctrl Pts',(17.3288454112575,0.000452601584348983,
4.59351524744837));
#55082=CARTESIAN_POINT('Ctrl Pts',(17.3234565584296,0.0676518012035294,
4.59398979695312));
#55083=CARTESIAN_POINT('Ctrl Pts',(17.3180677056016,0.134706745978521,4.58346365752876));
#55084=CARTESIAN_POINT('Ctrl Pts',(17.3126788527736,0.197661386620268,4.56129398922237));
#55085=CARTESIAN_POINT('Ctrl Pts',(17.296773574086,0.383472937993069,4.49585988588324));
#55086=CARTESIAN_POINT('Ctrl Pts',(17.2808682953984,0.533564938357213,4.32899388620009));
#55087=CARTESIAN_POINT('Ctrl Pts',(17.2649630167108,0.579021491014364,4.13731379770915));
#55088=CARTESIAN_POINT('Ctrl Pts',(17.2490577380232,0.624478043671518,3.94563370921821));
#55089=CARTESIAN_POINT('Ctrl Pts',(17.2331524593355,0.565299148621668,3.72913953191949));
#55090=CARTESIAN_POINT('Ctrl Pts',(17.2172471806479,0.428657250819126,3.58723623291525));
#55091=CARTESIAN_POINT('Ctrl Pts',(17.2013419019603,0.292015353016592,3.44533293391101));
#55092=CARTESIAN_POINT('Ctrl Pts',(17.1854366232727,0.0779104524613767,
3.37802051320125));
#55093=CARTESIAN_POINT('Ctrl Pts',(17.1695313445851,-0.115349538542919,
3.41620598662221));
#55094=CARTESIAN_POINT('Ctrl Pts',(17.1536260658975,-0.308609529547215,
3.45439146004317));
#55095=CARTESIAN_POINT('Ctrl Pts',(17.1377207872099,-0.48102461100059,3.59807482759486));
#55096=CARTESIAN_POINT('Ctrl Pts',(17.1218155085223,-0.553429071780215,
3.78128276563952));
#55097=CARTESIAN_POINT('Ctrl Pts',(17.1059102298347,-0.625833532559839,
3.96449070368418));
#55098=CARTESIAN_POINT('Ctrl Pts',(17.090004951147,-0.598227372665711,4.18722321222181));
#55099=CARTESIAN_POINT('Ctrl Pts',(17.0740996724594,-0.483286172800906,
4.34721094636728));
#55100=CARTESIAN_POINT('Ctrl Pts',(17.0590149187255,-0.374274584390508,
4.4989451987145));
#55101=CARTESIAN_POINT('Ctrl Pts',(17.0439301649915,-0.186706445247169,
4.59424147319602));
#55102=CARTESIAN_POINT('Ctrl Pts',(17.0288454112575,0.000186802344652959,
4.59500977980842));
#55103=CARTESIAN_POINT('Ctrl Pts',(16.9211545887425,-0.000535257393875686,
4.59425998651214));
#55104=CARTESIAN_POINT('Ctrl Pts',(16.9244335835047,-0.0412943609811605,
4.59463812105998));
#55105=CARTESIAN_POINT('Ctrl Pts',(16.9277125782669,-0.0819827620002526,
4.59080381827239));
#55106=CARTESIAN_POINT('Ctrl Pts',(16.9309915730291,-0.121736182180322,
4.58249572362891));
#55107=CARTESIAN_POINT('Ctrl Pts',(16.9468968517167,-0.31456638552074,4.54219600671859));
#55108=CARTESIAN_POINT('Ctrl Pts',(16.9628021304043,-0.485397543709551,
4.39663301068103));
#55109=CARTESIAN_POINT('Ctrl Pts',(16.978707409092,-0.555791216176751,4.21264310503418));
#55110=CARTESIAN_POINT('Ctrl Pts',(16.9946126877796,-0.626184888643955,
4.02865319938731));
#55111=CARTESIAN_POINT('Ctrl Pts',(17.0105179664672,-0.596141075389537,
3.80623638413113));
#55112=CARTESIAN_POINT('Ctrl Pts',(17.0264232451548,-0.479454624411006,
3.64751705115182));
#55113=CARTESIAN_POINT('Ctrl Pts',(17.0423285238424,-0.362768173432475,
3.48879771817251));
#55114=CARTESIAN_POINT('Ctrl Pts',(17.05823380253,-0.159439084729831,3.39377586747005));
#55115=CARTESIAN_POINT('Ctrl Pts',(17.0741390812176,0.0371725263090214,
3.40608151284405));
#55116=CARTESIAN_POINT('Ctrl Pts',(17.0900443599052,0.233784137347885,3.41838715821804));
#55117=CARTESIAN_POINT('Ctrl Pts',(17.1059496385929,0.423678270722955,3.5380202996685));
#55118=CARTESIAN_POINT('Ctrl Pts',(17.1218549172805,0.519663574146654,3.71005045990219));
#55119=CARTESIAN_POINT('Ctrl Pts',(17.1377601959681,0.615648877570348,3.88208062013586));
#55120=CARTESIAN_POINT('Ctrl Pts',(17.1536654746557,0.617725351042682,4.10650779915277));
#55121=CARTESIAN_POINT('Ctrl Pts',(17.1695707533433,0.524939565793509,4.28028453107927));
#55122=CARTESIAN_POINT('Ctrl Pts',(17.1854760320309,0.432153780544336,4.45406126300578));
#55123=CARTESIAN_POINT('Ctrl Pts',(17.2013813107185,0.244505736573655,4.5771875478419));
#55124=CARTESIAN_POINT('Ctrl Pts',(17.2172865894061,0.0481554769387473,
4.59312900463441));
#55125=CARTESIAN_POINT('Ctrl Pts',(17.2185759225182,0.0322386925622284,
4.59442127046022));
#55126=CARTESIAN_POINT('Ctrl Pts',(17.2198652556304,0.0162647237884017,
4.5950091984451));
#55127=CARTESIAN_POINT('Ctrl Pts',(17.2211545887425,0.000283723793354941,
4.5949151055343));
#55128=CARTESIAN_POINT('Origin',(4.,0.,4.));
#55129=CARTESIAN_POINT('',(17.6288454112575,-0.000376811216598938,4.5933658344624));
#55130=CARTESIAN_POINT('',(17.5211545887425,0.000390292690419375,4.59338796628294));
#55131=CARTESIAN_POINT('',(4.,-7.27562663373442E-17,4.5941));
#55132=CARTESIAN_POINT('Ctrl Pts',(17.6288454112575,-0.000376811216598938,
4.5933658344624));
#55133=CARTESIAN_POINT('Ctrl Pts',(17.6188882305552,0.123868145157646,4.5926473455414));
#55134=CARTESIAN_POINT('Ctrl Pts',(17.608931049853,0.248515939035854,4.55458993700248));
#55135=CARTESIAN_POINT('Ctrl Pts',(17.5989738691507,0.348483110949462,4.48236965854082));
#55136=CARTESIAN_POINT('Ctrl Pts',(17.5830685904631,0.508167440925656,4.36700731952407));
#55137=CARTESIAN_POINT('Ctrl Pts',(17.5671633117754,0.604877102606476,4.16447556457896));
#55138=CARTESIAN_POINT('Ctrl Pts',(17.5512580330878,0.594207110796467,3.96776840716434));
#55139=CARTESIAN_POINT('Ctrl Pts',(17.5353527544002,0.583537118986457,3.77106124974973));
#55140=CARTESIAN_POINT('Ctrl Pts',(17.5194474757126,0.465487473685617,3.58017868986561));
#55141=CARTESIAN_POINT('Ctrl Pts',(17.503542197025,0.294261577747463,3.48276592343564));
#55142=CARTESIAN_POINT('Ctrl Pts',(17.4876369183374,0.123035681809298,3.38535315700567));
#55143=CARTESIAN_POINT('Ctrl Pts',(17.4717316396498,-0.101366464766187,
3.38141018402985));
#55144=CARTESIAN_POINT('Ctrl Pts',(17.4558263609621,-0.275908889943427,
3.47274745088526));
#55145=CARTESIAN_POINT('Ctrl Pts',(17.4399210822745,-0.450451315120656,
3.56408471774066));
#55146=CARTESIAN_POINT('Ctrl Pts',(17.4240158035869,-0.575134018899647,
3.75070222442727));
#55147=CARTESIAN_POINT('Ctrl Pts',(17.4081105248993,-0.592707978595278,
3.94691310701022));
#55148=CARTESIAN_POINT('Ctrl Pts',(17.3922052462117,-0.610281938290908,
4.14312398959316));
#55149=CARTESIAN_POINT('Ctrl Pts',(17.3762999675241,-0.520747153903178,
4.34892824807245));
#55150=CARTESIAN_POINT('Ctrl Pts',(17.3603946888365,-0.365214210518585,
4.46982927381454));
#55151=CARTESIAN_POINT('Ctrl Pts',(17.3498782629768,-0.262377240481122,
4.54976793433994));
#55152=CARTESIAN_POINT('Ctrl Pts',(17.3393618371172,-0.130687628661636,
4.59258915708319));
#55153=CARTESIAN_POINT('Ctrl Pts',(17.3288454112575,0.000452601584348983,
4.59351524744837));
#55154=CARTESIAN_POINT('Ctrl Pts',(17.2211545887425,0.000283723793354941,
4.5949151055343));
#55155=CARTESIAN_POINT('Ctrl Pts',(17.235770534318,-0.18087770297476,4.59384846352355));
#55156=CARTESIAN_POINT('Ctrl Pts',(17.2503864798935,-0.362942684182573,
4.50513801271133));
#55157=CARTESIAN_POINT('Ctrl Pts',(17.265002425469,-0.47285052735612,4.36129398677095));
#55158=CARTESIAN_POINT('Ctrl Pts',(17.2809077041566,-0.592453796716944,
4.20476088336606));
#55159=CARTESIAN_POINT('Ctrl Pts',(17.2968129828442,-0.626607860139456,
3.98293804780737));
#55160=CARTESIAN_POINT('Ctrl Pts',(17.3127182615318,-0.559630616639302,
3.79767714163318));
#55161=CARTESIAN_POINT('Ctrl Pts',(17.3286235402194,-0.492653373139145,
3.61241623545897));
#55162=CARTESIAN_POINT('Ctrl Pts',(17.3445288189071,-0.324544822716309,
3.46371725866926));
#55163=CARTESIAN_POINT('Ctrl Pts',(17.3604340975947,-0.132493299638714,
3.41985649047097));
#55164=CARTESIAN_POINT('Ctrl Pts',(17.3763393762823,0.0595582234388708,
3.37599572227269));
#55165=CARTESIAN_POINT('Ctrl Pts',(17.3922446549699,0.275552719171213,3.43697316266583));
#55166=CARTESIAN_POINT('Ctrl Pts',(17.4081499336575,0.416314653091553,3.5747905507646));
#55167=CARTESIAN_POINT('Ctrl Pts',(17.4240552123451,0.557076587011893,3.71260793886338));
#55168=CARTESIAN_POINT('Ctrl Pts',(17.4399604910327,0.622605959120231,3.92726527466781));
#55169=CARTESIAN_POINT('Ctrl Pts',(17.4558657697203,0.582814454063527,4.12020099097945));
#55170=CARTESIAN_POINT('Ctrl Pts',(17.4717710484079,0.543022949006823,4.31313670729109));
#55171=CARTESIAN_POINT('Ctrl Pts',(17.4876763270955,0.397910566785078,4.48435080410994));
#55172=CARTESIAN_POINT('Ctrl Pts',(17.5035816057832,0.214106774115907,4.55522901164789));
#55173=CARTESIAN_POINT('Ctrl Pts',(17.5094392667696,0.146414762764002,4.58133232736073));
#55174=CARTESIAN_POINT('Ctrl Pts',(17.515296927756,0.073474912906076,4.59382676872096));
#55175=CARTESIAN_POINT('Ctrl Pts',(17.5211545887425,0.000390292690419375,
4.59338796628294));
#55176=CARTESIAN_POINT('Origin',(4.,0.,4.));
#55177=CARTESIAN_POINT('',(17.9288454112575,-0.000301159635511528,4.59489313984584));
#55178=CARTESIAN_POINT('',(17.8211545887425,-0.000441626631060947,4.59348913571676));
#55179=CARTESIAN_POINT('',(4.,-7.27562663373442E-17,4.5941));
#55180=CARTESIAN_POINT('Ctrl Pts',(17.9288454112575,-0.000301159635511528,
4.59489313984584));
#55181=CARTESIAN_POINT('Ctrl Pts',(17.9143199026809,0.179756887528332,4.59377956832623));
#55182=CARTESIAN_POINT('Ctrl Pts',(17.8997943941043,0.360751589755073,4.50630604003092));
#55183=CARTESIAN_POINT('Ctrl Pts',(17.8852688855277,0.470789914960854,4.36397502945801));
#55184=CARTESIAN_POINT('Ctrl Pts',(17.8693636068401,0.591280720462369,4.20812407407766));
#55185=CARTESIAN_POINT('Ctrl Pts',(17.8534583281524,0.626694694978596,3.98649889312445));
#55186=CARTESIAN_POINT('Ctrl Pts',(17.8375530494648,0.560771239653389,3.80086039350393));
#55187=CARTESIAN_POINT('Ctrl Pts',(17.8216477707772,0.494847784328189,3.61522189388343));
#55188=CARTESIAN_POINT('Ctrl Pts',(17.8057424920896,0.327586899161578,3.46557007559562));
#55189=CARTESIAN_POINT('Ctrl Pts',(17.789837213402,0.135787706397568,3.42061872235194));
#55190=CARTESIAN_POINT('Ctrl Pts',(17.7739319347144,-0.0560114863664412,
3.37566736910827));
#55191=CARTESIAN_POINT('Ctrl Pts',(17.7580266560268,-0.272348986727849,
3.43541648090873));
#55192=CARTESIAN_POINT('Ctrl Pts',(17.7421213773392,-0.41389176700556,3.57243179339102));
#55193=CARTESIAN_POINT('Ctrl Pts',(17.7262160986515,-0.555434547283271,
3.7094471058733));
#55194=CARTESIAN_POINT('Ctrl Pts',(17.710310819964,-0.622182607477285,3.92372861903742));
#55195=CARTESIAN_POINT('Ctrl Pts',(17.6944055412763,-0.583488062224059,
4.11688732754162));
#55196=CARTESIAN_POINT('Ctrl Pts',(17.6785002625887,-0.544793516970831,
4.31004603604583));
#55197=CARTESIAN_POINT('Ctrl Pts',(17.6625949839011,-0.400656366270352,
4.48208193989012));
#55198=CARTESIAN_POINT('Ctrl Pts',(17.6466897052135,-0.217258291784321,
4.55400343026805));
#55199=CARTESIAN_POINT('Ctrl Pts',(17.6407416072282,-0.148672903323923,
4.58089991415997));
#55200=CARTESIAN_POINT('Ctrl Pts',(17.6347935092429,-0.0745967331795002,
4.59379503652584));
#55201=CARTESIAN_POINT('Ctrl Pts',(17.6288454112575,-0.000376811216598938,
4.5933658344624));
#55202=CARTESIAN_POINT('Ctrl Pts',(17.5211545887425,0.000390292690419375,
4.59338796628294));
#55203=CARTESIAN_POINT('Ctrl Pts',(17.5312022064437,-0.12497140465997,4.59263529057266));
#55204=CARTESIAN_POINT('Ctrl Pts',(17.5412498241448,-0.250759050797478,
4.55382993891589));
#55205=CARTESIAN_POINT('Ctrl Pts',(17.551297441846,-0.351218450958555,4.48038168762358));
#55206=CARTESIAN_POINT('Ctrl Pts',(17.5672027205336,-0.510244680247213,
4.36411383780432));
#55207=CARTESIAN_POINT('Ctrl Pts',(17.5831079992212,-0.605801935707933,
4.16103581990878));
#55208=CARTESIAN_POINT('Ctrl Pts',(17.5990132779088,-0.594014368327242,
3.96439246823218));
#55209=CARTESIAN_POINT('Ctrl Pts',(17.6149185565964,-0.58222680094655,3.76774911655557));
#55210=CARTESIAN_POINT('Ctrl Pts',(17.6308238352841,-0.463094410724447,
3.5775404310979));
#55211=CARTESIAN_POINT('Ctrl Pts',(17.6467291139717,-0.291317751175132,
3.48110219315546));
#55212=CARTESIAN_POINT('Ctrl Pts',(17.6626343926593,-0.119541091625818,
3.38466395521302));
#55213=CARTESIAN_POINT('Ctrl Pts',(17.6785396713469,0.104879837250709,3.38199616478582));
#55214=CARTESIAN_POINT('Ctrl Pts',(17.6944449500345,0.278900439380867,3.47432375837312));
#55215=CARTESIAN_POINT('Ctrl Pts',(17.7103502287221,0.452921041511034,3.56665135196042));
#55216=CARTESIAN_POINT('Ctrl Pts',(17.7262555074097,0.576541316894826,3.75397432956222));
#55217=CARTESIAN_POINT('Ctrl Pts',(17.7421607860974,0.593000065018554,3.95028190484542));
#55218=CARTESIAN_POINT('Ctrl Pts',(17.758066064785,0.60945881314228,4.1465894801286));
#55219=CARTESIAN_POINT('Ctrl Pts',(17.7739713434726,0.518756034005955,4.35188165309317));
#55220=CARTESIAN_POINT('Ctrl Pts',(17.7898766221602,0.362538606470845,4.47189694310939));
#55221=CARTESIAN_POINT('Ctrl Pts',(17.8003026110209,0.260137309937395,4.55056755941266));
#55222=CARTESIAN_POINT('Ctrl Pts',(17.8107285998817,0.129585238016204,4.59259583028147));
#55223=CARTESIAN_POINT('Ctrl Pts',(17.8211545887425,-0.000441626631060947,
4.59348913571676));
#55224=CARTESIAN_POINT('Origin',(4.,0.,4.));
#55225=CARTESIAN_POINT('',(18.2288454112575,0.000530626821107938,4.59429426521737));
#55226=CARTESIAN_POINT('',(18.1211545887425,-0.000206261771334874,4.59499421029555));
#55227=CARTESIAN_POINT('',(4.,-7.27562663373442E-17,4.5941));
#55228=CARTESIAN_POINT('Ctrl Pts',(18.2288454112575,0.000530626821107938,
4.59429426521737));
#55229=CARTESIAN_POINT('Ctrl Pts',(18.2256568534942,0.0401596894680921,
4.59466101186164));
#55230=CARTESIAN_POINT('Ctrl Pts',(18.2224682957309,0.0797220295111884,
4.5910372210354));
#55231=CARTESIAN_POINT('Ctrl Pts',(18.2192797379675,0.118424305077702,4.58317806034235));
#55232=CARTESIAN_POINT('Ctrl Pts',(18.2033744592799,0.311480390123117,4.54397471188459));
#55233=CARTESIAN_POINT('Ctrl Pts',(18.1874691805923,0.483135922039688,4.39938477867344));
#55234=CARTESIAN_POINT('Ctrl Pts',(18.1715639019047,0.554573942717995,4.21579784094385));
#55235=CARTESIAN_POINT('Ctrl Pts',(18.1556586232171,0.626011963396302,4.03221090321426));
#55236=CARTESIAN_POINT('Ctrl Pts',(18.1397533445295,0.597232472836345,3.80962696096622));
#55237=CARTESIAN_POINT('Ctrl Pts',(18.1238480658419,0.481449795543417,3.65024714373002));
#55238=CARTESIAN_POINT('Ctrl Pts',(18.1079427871543,0.365667118250483,3.49086732649381));
#55239=CARTESIAN_POINT('Ctrl Pts',(18.0920375084667,0.16288125422457,3.39469163426944));
#55240=CARTESIAN_POINT('Ctrl Pts',(18.076132229779,-0.0337971069360236,
3.40587987606835));
#55241=CARTESIAN_POINT('Ctrl Pts',(18.0602269510914,-0.230475468096606,
3.41706811786726));
#55242=CARTESIAN_POINT('Ctrl Pts',(18.0443216724038,-0.421046326391869,
3.53562029368944));
#55243=CARTESIAN_POINT('Ctrl Pts',(18.0284163937162,-0.518007606080761,
3.70710225992629));
#55244=CARTESIAN_POINT('Ctrl Pts',(18.0125111150286,-0.614968885769652,
3.87858422616314));
#55245=CARTESIAN_POINT('Ctrl Pts',(17.996605836341,-0.618320586852172,4.10299598281466));
#55246=CARTESIAN_POINT('Ctrl Pts',(17.9807005576534,-0.526523749990007,
4.27729714530494));
#55247=CARTESIAN_POINT('Ctrl Pts',(17.9647952789658,-0.434726913127837,
4.45159830779523));
#55248=CARTESIAN_POINT('Ctrl Pts',(17.9488900002781,-0.247781538320971,
4.57578887612429));
#55249=CARTESIAN_POINT('Ctrl Pts',(17.9329847215905,-0.0515250326741526,
4.59284579538505));
#55250=CARTESIAN_POINT('Ctrl Pts',(17.9316049514795,-0.0344999389365885,
4.59432546938787));
#55251=CARTESIAN_POINT('Ctrl Pts',(17.9302251813685,-0.0174047750035579,
4.59499891739512));
#55252=CARTESIAN_POINT('Ctrl Pts',(17.9288454112575,-0.000301159635511528,
4.59489313984584));
#55253=CARTESIAN_POINT('Ctrl Pts',(17.8211545887425,-0.000441626631060947,
4.59348913571676));
#55254=CARTESIAN_POINT('Ctrl Pts',(17.8266338785693,-0.0687761401428734,
4.59395860479535));
#55255=CARTESIAN_POINT('Ctrl Pts',(17.8321131683962,-0.136965594625977,
4.58306684864343));
#55256=CARTESIAN_POINT('Ctrl Pts',(17.837592458223,-0.200847632772524,4.56016175744822));
#55257=CARTESIAN_POINT('Ctrl Pts',(17.8534977369106,-0.386284368546891,
4.49367287470298));
#55258=CARTESIAN_POINT('Ctrl Pts',(17.8694030155983,-0.535425764161732,
4.32595670214462));
#55259=CARTESIAN_POINT('Ctrl Pts',(17.8853082942859,-0.579792400402821,
4.13402141072584));
#55260=CARTESIAN_POINT('Ctrl Pts',(17.9012135729735,-0.624159036643913,
3.94208611930704));
#55261=CARTESIAN_POINT('Ctrl Pts',(17.9171188516611,-0.563750913511241,
3.72593170902781));
#55262=CARTESIAN_POINT('Ctrl Pts',(17.9330241303487,-0.426304885490399,
3.58480714034942));
#55263=CARTESIAN_POINT('Ctrl Pts',(17.9489294090363,-0.288858857469565,
3.44368257167104));
#55264=CARTESIAN_POINT('Ctrl Pts',(17.9648346877239,-0.0743749245605683,
3.37758784459349));
#55265=CARTESIAN_POINT('Ctrl Pts',(17.9807399664116,0.118664965311668,3.41687086155347));
#55266=CARTESIAN_POINT('Ctrl Pts',(17.9966452450992,0.311704855183904,3.45615387851346));
#55267=CARTESIAN_POINT('Ctrl Pts',(18.0125505237868,0.483300702019379,3.60081463951098));
#55268=CARTESIAN_POINT('Ctrl Pts',(18.0284558024744,0.554662952572844,3.78443104318807));
#55269=CARTESIAN_POINT('Ctrl Pts',(18.044361081162,0.62602520312631,3.96804744686516));
#55270=CARTESIAN_POINT('Ctrl Pts',(18.0602663598496,0.597153857397765,4.19061949322182));
#55271=CARTESIAN_POINT('Ctrl Pts',(18.0761716385372,0.481305415899848,4.34995151481781));
#55272=CARTESIAN_POINT('Ctrl Pts',(18.0911659552723,0.372092100044007,4.50015792394613));
#55273=CARTESIAN_POINT('Ctrl Pts',(18.1061602720074,0.185579460002099,4.59416090236354));
#55274=CARTESIAN_POINT('Ctrl Pts',(18.1211545887425,-0.000206261771334874,
4.59499421029555));
#55275=CARTESIAN_POINT('Origin',(4.,0.,4.));
#55276=CARTESIAN_POINT('',(18.5288454112575,4.04073003155148E-5,4.59311858068669));
#55277=CARTESIAN_POINT('',(18.4211545887425,0.000547083855738422,4.59411609730493));
#55278=CARTESIAN_POINT('',(4.,-7.27562663373442E-17,4.5941));
#55279=CARTESIAN_POINT('Ctrl Pts',(18.5288454112575,4.04073003155148E-5,
4.59311858068669));
#55280=CARTESIAN_POINT('Ctrl Pts',(18.5210885256199,0.0969311390001333,
4.59317716754242));
#55281=CARTESIAN_POINT('Ctrl Pts',(18.5133316399822,0.193796352446061,4.57078374547556));
#55282=CARTESIAN_POINT('Ctrl Pts',(18.5055747543446,0.27868347559656,4.52579129559858));
#55283=CARTESIAN_POINT('Ctrl Pts',(18.489669475657,0.452742165355285,4.43353552600749));
#55284=CARTESIAN_POINT('Ctrl Pts',(18.4737641969693,0.576439736070726,4.24626358090446));
#55285=CARTESIAN_POINT('Ctrl Pts',(18.4578589182817,0.592979496483005,4.04996281465819));
#55286=CARTESIAN_POINT('Ctrl Pts',(18.4419536395941,0.609519256895283,3.85366204841193));
#55287=CARTESIAN_POINT('Ctrl Pts',(18.4260483609065,0.518901207004412,3.64833246102244));
#55288=CARTESIAN_POINT('Ctrl Pts',(18.4101430822189,0.362733321586741,3.52825271224048));
#55289=CARTESIAN_POINT('Ctrl Pts',(18.3942378035313,0.206565436169079,3.40817296345854));
#55290=CARTESIAN_POINT('Ctrl Pts',(18.3783325248437,-0.015152284775374,
3.37334305328413));
#55291=CARTESIAN_POINT('Ctrl Pts',(18.3624272461561,-0.200616443892158,
3.43975540293737));
#55292=CARTESIAN_POINT('Ctrl Pts',(18.3465219674685,-0.386080603008964,
3.50616775259061));
#55293=CARTESIAN_POINT('Ctrl Pts',(18.3306166887808,-0.535291200298091,
3.67382236207151));
#55294=CARTESIAN_POINT('Ctrl Pts',(18.3147114100932,-0.579737042064157,
3.86573932758804));
#55295=CARTESIAN_POINT('Ctrl Pts',(18.2988061314056,-0.624182883830224,
4.05765629310458));
#55296=CARTESIAN_POINT('Ctrl Pts',(18.282900852718,-0.563863970073232,4.27383561465674));
#55297=CARTESIAN_POINT('Ctrl Pts',(18.2669955740304,-0.426476194107598,
4.41501689358062));
#55298=CARTESIAN_POINT('Ctrl Pts',(18.2542788531061,-0.316630774880643,
4.52789532589669));
#55299=CARTESIAN_POINT('Ctrl Pts',(18.2415621321818,-0.157519428275204,
4.5928315930404));
#55300=CARTESIAN_POINT('Ctrl Pts',(18.2288454112575,0.000530626821107938,
4.59429426521737));
#55301=CARTESIAN_POINT('Ctrl Pts',(18.1211545887425,-0.000206261771334874,
4.59499421029555));
#55302=CARTESIAN_POINT('Ctrl Pts',(18.122065550695,-0.0114934532352288,
4.59504483693191));
#55303=CARTESIAN_POINT('Ctrl Pts',(18.1229765126475,-0.0227779616248223,
4.59475157188293));
#55304=CARTESIAN_POINT('Ctrl Pts',(18.1238874746001,-0.0340422900297544,
4.59410612569417));
#55305=CARTESIAN_POINT('Ctrl Pts',(18.1397927532877,-0.230716017194119,
4.58283671813918));
#55306=CARTESIAN_POINT('Ctrl Pts',(18.1556980319753,-0.421237934255556,
4.46420590619388));
#55307=CARTESIAN_POINT('Ctrl Pts',(18.1716033106629,-0.518128437217054,
4.29268393984778));
#55308=CARTESIAN_POINT('Ctrl Pts',(18.1875085893505,-0.615018940178556,
4.12116197350168));
#55309=CARTESIAN_POINT('Ctrl Pts',(18.2034138680381,-0.618278029040109,
3.89674885275477));
#55310=CARTESIAN_POINT('Ctrl Pts',(18.2193191467258,-0.526409268077163,
3.72248558851787));
#55311=CARTESIAN_POINT('Ctrl Pts',(18.2352244254134,-0.434540507114227,
3.54822232428098));
#55312=CARTESIAN_POINT('Ctrl Pts',(18.251129704101,-0.24754389632682,3.42410891655409));
#55313=CARTESIAN_POINT('Ctrl Pts',(18.2670349827886,-0.0512803682143169,
3.40713299136011));
#55314=CARTESIAN_POINT('Ctrl Pts',(18.2829402614762,0.144983159898198,3.39015706616613));
#55315=CARTESIAN_POINT('Ctrl Pts',(18.2988455401638,0.35051360533581,3.48031862350507));
#55316=CARTESIAN_POINT('Ctrl Pts',(18.3147508188514,0.470940082829639,3.63621929066782));
#55317=CARTESIAN_POINT('Ctrl Pts',(18.330656097539,0.591366560323475,3.79211995783059));
#55318=CARTESIAN_POINT('Ctrl Pts',(18.3465613762266,0.62668906987352,4.01375973481717));
#55319=CARTESIAN_POINT('Ctrl Pts',(18.3624666549143,0.560689009466533,4.199371012841));
#55320=CARTESIAN_POINT('Ctrl Pts',(18.3783719336019,0.49468894905955,4.38498229086483));
#55321=CARTESIAN_POINT('Ctrl Pts',(18.3942772122895,0.327366318695548,4.53456506992591));
#55322=CARTESIAN_POINT('Ctrl Pts',(18.4101824909771,0.135548591400956,4.57943726620491));
#55323=CARTESIAN_POINT('Ctrl Pts',(18.4138398568989,0.0914407431336166,
4.58975547846199));
#55324=CARTESIAN_POINT('Ctrl Pts',(18.4174972228207,0.0460377050408626,
4.59453706917327));
#55325=CARTESIAN_POINT('Ctrl Pts',(18.4211545887425,0.000547083855738422,
4.59411609730493));
#55326=CARTESIAN_POINT('Origin',(4.,0.,4.));
#55327=CARTESIAN_POINT('',(18.8288454112575,-0.000545657836941327,4.59414547262434));
#55328=CARTESIAN_POINT('',(18.7211545887425,-5.63168744233308E-5,4.59312091231189));
#55329=CARTESIAN_POINT('',(4.,-7.27562663373442E-17,4.5941));
#55330=CARTESIAN_POINT('Ctrl Pts',(18.8288454112575,-0.000545657836941327,
4.59414547262434));
#55331=CARTESIAN_POINT('Ctrl Pts',(18.8165201977456,0.15273698101805,4.59272393327212));
#55332=CARTESIAN_POINT('Ctrl Pts',(18.8041949842336,0.307016766534516,4.53213273669464));
#55333=CARTESIAN_POINT('Ctrl Pts',(18.7918697707216,0.416139138999065,4.42538122089617));
#55334=CARTESIAN_POINT('Ctrl Pts',(18.775964492034,0.556957936451544,4.28762193522949));
#55335=CARTESIAN_POINT('Ctrl Pts',(18.7600592133464,0.622575889387102,4.0729916608594));
#55336=CARTESIAN_POINT('Ctrl Pts',(18.7441539346588,0.582864009884755,3.88003953951897));
#55337=CARTESIAN_POINT('Ctrl Pts',(18.7282486559712,0.543152130382401,3.6870874181785));
#55338=CARTESIAN_POINT('Ctrl Pts',(18.7123433772835,0.3981104184421,3.51581344986768));
#55339=CARTESIAN_POINT('Ctrl Pts',(18.6964380985959,0.214335891977863,3.44485939483061));
#55340=CARTESIAN_POINT('Ctrl Pts',(18.6805328199083,0.0305613655136472,
3.37390533979354));
#55341=CARTESIAN_POINT('Ctrl Pts',(18.6646275412207,-0.191945975474496,
3.40327119803019));
#55342=CARTESIAN_POINT('Ctrl Pts',(18.6487222625331,-0.351020173514001,
3.51947340980541));
#55343=CARTESIAN_POINT('Ctrl Pts',(18.6328169838455,-0.510094371553506,
3.63567562158063));
#55344=CARTESIAN_POINT('Ctrl Pts',(18.6169117051579,-0.605735426644373,
3.83871418689441));
#55345=CARTESIAN_POINT('Ctrl Pts',(18.6010064264702,-0.594029012528289,
4.03536238640794));
#55346=CARTESIAN_POINT('Ctrl Pts',(18.5851011477826,-0.582322598412206,
4.23201058592146));
#55347=CARTESIAN_POINT('Ctrl Pts',(18.569195869095,-0.463268715089173,4.42226841963472));
#55348=CARTESIAN_POINT('Ctrl Pts',(18.5532905904074,-0.29153186902666,4.51877753945177));
#55349=CARTESIAN_POINT('Ctrl Pts',(18.5451421973574,-0.203549800283198,
4.56821988225003));
#55350=CARTESIAN_POINT('Ctrl Pts',(18.5369938043075,-0.101740616897797,
4.59305703682098));
#55351=CARTESIAN_POINT('Ctrl Pts',(18.5288454112575,4.04073003155148E-5,
4.59311858068669));
#55352=CARTESIAN_POINT('Ctrl Pts',(18.4211545887425,0.000547083855738422,
4.59411609730493));
#55353=CARTESIAN_POINT('Ctrl Pts',(18.4334025015083,-0.151793472668411,
4.59270633223614));
#55354=CARTESIAN_POINT('Ctrl Pts',(18.4456504142741,-0.305116246576315,
4.53295143150856));
#55355=CARTESIAN_POINT('Ctrl Pts',(18.4578983270399,-0.414068183831284,
4.42739736222451));
#55356=CARTESIAN_POINT('Ctrl Pts',(18.4738036057275,-0.555554407543751,
4.29032364846819));
#55357=CARTESIAN_POINT('Ctrl Pts',(18.4897088844152,-0.622214030743504,
4.07601460745865));
#55358=CARTESIAN_POINT('Ctrl Pts',(18.5056141631028,-0.583439774593308,
3.88287188415962));
#55359=CARTESIAN_POINT('Ctrl Pts',(18.5215194417904,-0.54466551844311,3.68972916086059));
#55360=CARTESIAN_POINT('Ctrl Pts',(18.537424720478,-0.400457382942952,3.51775275527208));
#55361=CARTESIAN_POINT('Ctrl Pts',(18.5533299991656,-0.217029642971419,
3.44590695711865));
#55362=CARTESIAN_POINT('Ctrl Pts',(18.5692352778532,-0.0336019029998957,
3.37406115896522));
#55363=CARTESIAN_POINT('Ctrl Pts',(18.5851405565408,0.189045441442997,3.40234596824686));
#55364=CARTESIAN_POINT('Ctrl Pts',(18.6010458352284,0.348682149221421,3.51777419717301));
#55365=CARTESIAN_POINT('Ctrl Pts',(18.6169511139161,0.508318856999844,3.63320242609916));
#55366=CARTESIAN_POINT('Ctrl Pts',(18.6328563926037,0.604944928113798,3.83577407466982));
#55367=CARTESIAN_POINT('Ctrl Pts',(18.6487616712913,0.594193758619731,4.03247681196108));
#55368=CARTESIAN_POINT('Ctrl Pts',(18.6646669499789,0.583442589125664,4.22917954925235));
#55369=CARTESIAN_POINT('Ctrl Pts',(18.6805722286665,0.465314179023576,4.42001337526422));
#55370=CARTESIAN_POINT('Ctrl Pts',(18.6964775073541,0.294048096631404,4.51735547060535));
#55371=CARTESIAN_POINT('Ctrl Pts',(18.7047032011502,0.205474838715737,4.56769764225005));
#55372=CARTESIAN_POINT('Ctrl Pts',(18.7129288949463,0.102689258835563,4.59303430424318));
#55373=CARTESIAN_POINT('Ctrl Pts',(18.7211545887425,-5.63168744233308E-5,
4.59312091231189));
#55374=CARTESIAN_POINT('Origin',(4.,0.,4.));
#55375=CARTESIAN_POINT('',(19.1288454112575,0.000222628893785728,4.59497983522242));
#55376=CARTESIAN_POINT('',(19.0211545887425,-0.000526118841417405,4.59432346427954));
#55377=CARTESIAN_POINT('',(4.,-7.27562663373442E-17,4.5941));
#55378=CARTESIAN_POINT('Ctrl Pts',(19.1288454112575,0.000222628893785728,
4.59497983522242));
#55379=CARTESIAN_POINT('Ctrl Pts',(19.1278571485589,0.012468395078646,4.59503853204781));
#55380=CARTESIAN_POINT('Ctrl Pts',(19.1268688858602,0.0247107891953784,
4.59469333777414));
#55381=CARTESIAN_POINT('Ctrl Pts',(19.1258806231615,0.0369274203756033,
4.59393377720877));
#55382=CARTESIAN_POINT('Ctrl Pts',(19.1099753444739,0.233544093050454,4.58170927203582));
#55383=CARTESIAN_POINT('Ctrl Pts',(19.0940700657862,0.423487581379576,4.46215450773496));
#55384=CARTESIAN_POINT('Ctrl Pts',(19.0781647870986,0.519543871337238,4.29016397409385));
#55385=CARTESIAN_POINT('Ctrl Pts',(19.062259508411,0.615600161294901,4.11817344045274));
#55386=CARTESIAN_POINT('Ctrl Pts',(19.0463542297234,0.617769252881104,3.89374713747137));
#55387=CARTESIAN_POINT('Ctrl Pts',(19.0304489510358,0.525055191022736,3.71993212880311));
#55388=CARTESIAN_POINT('Ctrl Pts',(19.0145436723482,0.432341129164367,3.54611712013485));
#55389=CARTESIAN_POINT('Ctrl Pts',(18.9986383936606,0.244743913861428,3.42291340577968));
#55390=CARTESIAN_POINT('Ctrl Pts',(18.982733114973,0.0484002497885746,3.40689091904056));
#55391=CARTESIAN_POINT('Ctrl Pts',(18.9668278362853,-0.147943414284278,
3.39086843230144));
#55392=CARTESIAN_POINT('Ctrl Pts',(18.9509225575977,-0.353033527127044,
3.48202717317836));
#55393=CARTESIAN_POINT('Ctrl Pts',(18.9350172789101,-0.472701385564812,
3.63851090447403));
#55394=CARTESIAN_POINT('Ctrl Pts',(18.9191120002225,-0.592369244002587,
3.79499463576972));
#55395=CARTESIAN_POINT('Ctrl Pts',(18.9032067215349,-0.626614848035354,
4.01680335748416));
#55396=CARTESIAN_POINT('Ctrl Pts',(18.8873014428473,-0.559714065105754,
4.20209188855652));
#55397=CARTESIAN_POINT('Ctrl Pts',(18.8713961641597,-0.492813282176159,
4.38738041962887));
#55398=CARTESIAN_POINT('Ctrl Pts',(18.8554908854721,-0.324766112284209,
4.53614876005914));
#55399=CARTESIAN_POINT('Ctrl Pts',(18.8395856067844,-0.132732706353525,
4.58008878179264));
#55400=CARTESIAN_POINT('Ctrl Pts',(18.8360055416088,-0.0895085590353085,
4.5899790920924));
#55401=CARTESIAN_POINT('Ctrl Pts',(18.8324254764332,-0.0450691735440342,
4.59455838259347));
#55402=CARTESIAN_POINT('Ctrl Pts',(18.8288454112575,-0.000545657836941327,
4.59414547262434));
#55403=CARTESIAN_POINT('Ctrl Pts',(18.7211545887425,-5.63168744233308E-5,
4.59312091231189));
#55404=CARTESIAN_POINT('Ctrl Pts',(18.728834173634,-0.0959805501911411,
4.59320177041728));
#55405=CARTESIAN_POINT('Ctrl Pts',(18.7365137585255,-0.191869914813978,
4.57127401300463));
#55406=CARTESIAN_POINT('Ctrl Pts',(18.744193343417,-0.276126457005151,4.5271386400555));
#55407=CARTESIAN_POINT('Ctrl Pts',(18.7600986221046,-0.450631173567243,
4.43572934949413));
#55408=CARTESIAN_POINT('Ctrl Pts',(18.7760039007922,-0.575236852009173,
4.249060403701));
#55409=CARTESIAN_POINT('Ctrl Pts',(18.7919091794798,-0.592729836422094,
4.05284228527226));
#55410=CARTESIAN_POINT('Ctrl Pts',(18.8078144581674,-0.610222820835014,
3.85662416684351));
#55411=CARTESIAN_POINT('Ctrl Pts',(18.823719736855,-0.520603111218926,3.65085687577915));
#55412=CARTESIAN_POINT('Ctrl Pts',(18.8396250155426,-0.365020286731977,
3.53002004684018));
#55413=CARTESIAN_POINT('Ctrl Pts',(18.8555302942302,-0.209437462245028,
3.40918321790122));
#55414=CARTESIAN_POINT('Ctrl Pts',(18.8714355729179,0.0121084771127808,
3.37327685108765));
#55415=CARTESIAN_POINT('Ctrl Pts',(18.8873408516055,0.197893008823487,3.43878763096633));
#55416=CARTESIAN_POINT('Ctrl Pts',(18.9032461302931,0.383677540534204,3.50429841084501));
#55417=CARTESIAN_POINT('Ctrl Pts',(18.9191514089807,0.533700664597814,3.67122633741595));
#55418=CARTESIAN_POINT('Ctrl Pts',(18.9350566876683,0.579078109400399,3.86292516893752));
#55419=CARTESIAN_POINT('Ctrl Pts',(18.9509619663559,0.624455554202981,4.05462400045908));
#55420=CARTESIAN_POINT('Ctrl Pts',(18.9668672450435,0.56518731974455,4.27109373693126));
#55421=CARTESIAN_POINT('Ctrl Pts',(18.9827725237311,0.428486871854059,4.41294063344238));
#55422=CARTESIAN_POINT('Ctrl Pts',(18.9955665454016,0.318526617336051,4.52704063153052));
#55423=CARTESIAN_POINT('Ctrl Pts',(19.008360567072,0.158464569423419,4.5928566151945));
#55424=CARTESIAN_POINT('Ctrl Pts',(19.0211545887425,-0.000526118841417405,
4.59432346427954));
#55425=CARTESIAN_POINT('Origin',(4.,0.,4.));
#55426=CARTESIAN_POINT('',(19.4288454112575,0.000431836873498515,4.59346738712276));
#55427=CARTESIAN_POINT('',(19.3211545887425,0.000315695961457875,4.59487351203822));
#55428=CARTESIAN_POINT('',(4.,-7.27562663373442E-17,4.5941));
#55429=CARTESIAN_POINT('Ctrl Pts',(19.4288454112575,0.000431836873498515,
4.59346738712276));
#55430=CARTESIAN_POINT('Ctrl Pts',(19.4232888206845,0.0697367837969298,
4.59393182999066));
#55431=CARTESIAN_POINT('Ctrl Pts',(19.4177322301115,0.13889623855249,4.58272225272434));
#55432=CARTESIAN_POINT('Ctrl Pts',(19.4121756395385,0.203565929825556,4.55917964700716));
#55433=CARTESIAN_POINT('Ctrl Pts',(19.3962703608509,0.38867754617092,4.49179089484985));
#55434=CARTESIAN_POINT('Ctrl Pts',(19.3803650821633,0.537002597765565,4.32335233206236));
#55435=CARTESIAN_POINT('Ctrl Pts',(19.3644598034757,0.580436494614329,4.13120381907284));
#55436=CARTESIAN_POINT('Ctrl Pts',(19.3485545247881,0.623870391463095,3.93905530608331));
#55437=CARTESIAN_POINT('Ctrl Pts',(19.3326492461004,0.562413133565966,3.72319684289176));
#55438=CARTESIAN_POINT('Ctrl Pts',(19.3167439674128,0.424283294458304,3.58274150440131));
#55439=CARTESIAN_POINT('Ctrl Pts',(19.3008386887252,0.286153455350651,3.44228616591086));
#55440=CARTESIAN_POINT('Ctrl Pts',(19.2849334100376,0.071351035032473,3.37723395212151));
#55441=CARTESIAN_POINT('Ctrl Pts',(19.26902813135,-0.12149578302492,3.4174540870367));
#55442=CARTESIAN_POINT('Ctrl Pts',(19.2531228526624,-0.314342601082313,
3.45767422195189));
#55443=CARTESIAN_POINT('Ctrl Pts',(19.2372175739748,-0.485233816878921,
3.60316670557164));
#55444=CARTESIAN_POINT('Ctrl Pts',(19.2213122952871,-0.555703413721375,
3.78712754492824));
#55445=CARTESIAN_POINT('Ctrl Pts',(19.2054070165995,-0.626173010563829,
3.97108838428485));
#55446=CARTESIAN_POINT('Ctrl Pts',(19.1895017379119,-0.59622098845213,4.19351757937831));
#55447=CARTESIAN_POINT('Ctrl Pts',(19.1735964592243,-0.479600048885993,
4.35228505390253));
#55448=CARTESIAN_POINT('Ctrl Pts',(19.1586794432354,-0.370225264934164,
4.50118762911129));
#55449=CARTESIAN_POINT('Ctrl Pts',(19.1437624272465,-0.184617181632464,
4.59409385471947));
#55450=CARTESIAN_POINT('Ctrl Pts',(19.1288454112575,0.000222628893785728,
4.59497983522242));
#55451=CARTESIAN_POINT('Ctrl Pts',(19.0211545887425,-0.000526118841417405,
4.59432346427954));
#55452=CARTESIAN_POINT('Ctrl Pts',(19.0242658457596,-0.0391895592568775,
4.59468017342281));
#55453=CARTESIAN_POINT('Ctrl Pts',(19.0273771027768,-0.0777896429211806,
4.59123148246997));
#55454=CARTESIAN_POINT('Ctrl Pts',(19.030488359794,-0.115590453236054,4.58374636034569));
#55455=CARTESIAN_POINT('Ctrl Pts',(19.0463936384816,-0.308834669113126,
4.5454811341878));
#55456=CARTESIAN_POINT('Ctrl Pts',(19.0622989171692,-0.481190439544719,
4.40172662532195));
#55457=CARTESIAN_POINT('Ctrl Pts',(19.0782041958568,-0.553519286527586,
4.21848882245705));
#55458=CARTESIAN_POINT('Ctrl Pts',(19.0941094745444,-0.625848133510457,
4.03525101959215));
#55459=CARTESIAN_POINT('Ctrl Pts',(19.1100147532321,-0.598150057044591,
3.81252992272818));
#55460=CARTESIAN_POINT('Ctrl Pts',(19.1259200319197,-0.483142842019737,
3.65258963701249));
#55461=CARTESIAN_POINT('Ctrl Pts',(19.1418253106073,-0.36813562699489,3.49264935129682));
#55462=CARTESIAN_POINT('Ctrl Pts',(19.1577305892949,-0.165819273411065,
3.39548987672941));
#55463=CARTESIAN_POINT('Ctrl Pts',(19.1736358679825,0.0309111084379188,
3.40572273351557));
#55464=CARTESIAN_POINT('Ctrl Pts',(19.1895411466701,0.227641490286902,3.41595559030173));
#55465=CARTESIAN_POINT('Ctrl Pts',(19.2054464253577,0.418785900401045,3.53358077844144));
#55466=CARTESIAN_POINT('Ctrl Pts',(19.2213517040453,0.516578912360374,3.70458978792342));
#55467=CARTESIAN_POINT('Ctrl Pts',(19.237256982733,0.614371924319703,3.87559879740541));
#55468=CARTESIAN_POINT('Ctrl Pts',(19.2531622614206,0.618813538124218,4.09999162822965));
#55469=CARTESIAN_POINT('Ctrl Pts',(19.2690675401082,0.527864352527146,4.27473658562515));
#55470=CARTESIAN_POINT('Ctrl Pts',(19.2849728187958,0.436915166930073,4.44948154302064));
#55471=CARTESIAN_POINT('Ctrl Pts',(19.3008780974834,0.250575181931413,4.5745786269874));
#55472=CARTESIAN_POINT('Ctrl Pts',(19.316783376171,0.0544038354309166,4.59258854924263));
#55473=CARTESIAN_POINT('Ctrl Pts',(19.3182404470282,0.0364327229714708,
4.59423842494573));
#55474=CARTESIAN_POINT('Ctrl Pts',(19.3196975178853,0.0183791031991185,
4.59498959766064));
#55475=CARTESIAN_POINT('Ctrl Pts',(19.3211545887425,0.000315695961457875,
4.59487351203822));
#55476=CARTESIAN_POINT('Origin',(4.,0.,4.));
#55477=CARTESIAN_POINT('',(19.7288454112575,-0.000401422265437046,4.59340756962635));
#55478=CARTESIAN_POINT('',(19.6211545887425,0.000364945106097663,4.59334757974602));
#55479=CARTESIAN_POINT('',(4.,-7.27562663373442E-17,4.5941));
#55480=CARTESIAN_POINT('Ctrl Pts',(19.7288454112575,-0.000401422265437046,
4.59340756962635));
#55481=CARTESIAN_POINT('Ctrl Pts',(19.7187204928102,0.125914276337785,4.59262579220321));
#55482=CARTESIAN_POINT('Ctrl Pts',(19.7085955743629,0.252675872983383,4.55317429478549));
#55483=CARTESIAN_POINT('Ctrl Pts',(19.6984706559155,0.353547469597214,4.47867015725961));
#55484=CARTESIAN_POINT('Ctrl Pts',(19.6825653772279,0.512007102052776,4.36163128164859));
#55485=CARTESIAN_POINT('Ctrl Pts',(19.6666600985403,0.606576931433326,4.15809158444534));
#55486=CARTESIAN_POINT('Ctrl Pts',(19.6507548198527,0.593834428727047,3.9615078130365));
#55487=CARTESIAN_POINT('Ctrl Pts',(19.6348495411651,0.581091926020768,3.76492404162769));
#55488=CARTESIAN_POINT('Ctrl Pts',(19.6189442624775,0.46103709122769,3.57529619601327));
#55489=CARTESIAN_POINT('Ctrl Pts',(19.6030389837899,0.288794059426421,3.47969339775167));
#55490=CARTESIAN_POINT('Ctrl Pts',(19.5871337051022,0.116551027625133,3.38409059949006));
#55491=CARTESIAN_POINT('Ctrl Pts',(19.5712284264146,-0.107880201184358,
3.38251284858128));
#55492=CARTESIAN_POINT('Ctrl Pts',(19.555323147727,-0.281450319664219,3.47568456171554));
#55493=CARTESIAN_POINT('Ctrl Pts',(19.5394178690394,-0.45502043814407,3.5688562748498));
#55494=CARTESIAN_POINT('Ctrl Pts',(19.5235125903518,-0.577729446294298,
3.75677745202708));
#55495=CARTESIAN_POINT('Ctrl Pts',(19.5076073116642,-0.593234549413986,
3.95316264945144));
#55496=CARTESIAN_POINT('Ctrl Pts',(19.4917020329766,-0.608739652533674,
4.1495478468758));
#55497=CARTESIAN_POINT('Ctrl Pts',(19.475796754289,-0.517040850622822,4.35439706454724));
#55498=CARTESIAN_POINT('Ctrl Pts',(19.4598914756013,-0.360242359119356,
4.47365220261941));
#55499=CARTESIAN_POINT('Ctrl Pts',(19.4495427874867,-0.258222223711561,
4.55124494740629));
#55500=CARTESIAN_POINT('Ctrl Pts',(19.4391940993721,-0.128642866595325,
4.59260240088276));
#55501=CARTESIAN_POINT('Ctrl Pts',(19.4288454112575,0.000431836873498515,
4.59346738712276));
#55502=CARTESIAN_POINT('Ctrl Pts',(19.3211545887425,0.000315695961457875,
4.59487351203822));
#55503=CARTESIAN_POINT('Ctrl Pts',(19.3356027965729,-0.178799726336078,
4.59372241551416));
#55504=CARTESIAN_POINT('Ctrl Pts',(19.3500510044034,-0.35887750705714,4.50729762043595));
#55505=CARTESIAN_POINT('Ctrl Pts',(19.3644992122339,-0.469016560662847,
4.36625733020606));
#55506=CARTESIAN_POINT('Ctrl Pts',(19.3804044909215,-0.590262902253753,
4.21099342837053));
#55507=CARTESIAN_POINT('Ctrl Pts',(19.3963097696091,-0.626752877433238,
3.98954286415574));
#55508=CARTESIAN_POINT('Ctrl Pts',(19.4122150482967,-0.561731832709929,
3.80358636875254));
#55509=CARTESIAN_POINT('Ctrl Pts',(19.4281203269843,-0.49671078798662,3.61762987334934));
#55510=CARTESIAN_POINT('Ctrl Pts',(19.4440256056719,-0.330178723360516,
3.46716744675772));
#55511=CARTESIAN_POINT('Ctrl Pts',(19.4599308843595,-0.138600118749324,
3.42128506802099));
#55512=CARTESIAN_POINT('Ctrl Pts',(19.4758361630471,0.0529784858618673,
3.37540268928427));
#55513=CARTESIAN_POINT('Ctrl Pts',(19.4917414417347,0.269603630458146,3.43410035840244));
#55514=CARTESIAN_POINT('Ctrl Pts',(19.5076467204224,0.411810215621333,3.57042659223364));
#55515=CARTESIAN_POINT('Ctrl Pts',(19.52355199911,0.554016800784528,3.70675282606484));
#55516=CARTESIAN_POINT('Ctrl Pts',(19.5394572777976,0.621804826514621,3.92070762460909));
#55517=CARTESIAN_POINT('Ctrl Pts',(19.5553625564852,0.584048894878601,4.11405198996909));
#55518=CARTESIAN_POINT('Ctrl Pts',(19.5712678351728,0.546292963242583,4.30739635532907));
#55519=CARTESIAN_POINT('Ctrl Pts',(19.5871731138604,0.402993074240464,4.4801302875048));
#55520=CARTESIAN_POINT('Ctrl Pts',(19.6030783925481,0.219946482677819,4.55294168410437));
#55521=CARTESIAN_POINT('Ctrl Pts',(19.6091037912795,0.150602919307179,4.5805248346624));
#55522=CARTESIAN_POINT('Ctrl Pts',(19.615129190011,0.0755552166468998,4.59376787586841));
#55523=CARTESIAN_POINT('Ctrl Pts',(19.6211545887425,0.000364945106097663,
4.59334757974602));
#55524=CARTESIAN_POINT('Origin',(4.,0.,4.));
#55525=CARTESIAN_POINT('',(20.0288454112575,-0.000266600559035268,4.5949350414008));
#55526=CARTESIAN_POINT('',(19.9211545887425,-0.000461335262921832,4.59353843444423));
#55527=CARTESIAN_POINT('',(4.,-7.27562663373442E-17,4.5941));
#55528=CARTESIAN_POINT('Ctrl Pts',(20.0288454112575,-0.000266600559035268,
4.5949350414008));
#55529=CARTESIAN_POINT('Ctrl Pts',(20.0141521649359,0.181839152323842,4.59391190659116));
#55530=CARTESIAN_POINT('Ctrl Pts',(19.9994589186142,0.364814066967773,4.50413264800542));
#55531=CARTESIAN_POINT('Ctrl Pts',(19.9847656722925,0.474598868642052,4.35899217880197));
#55532=CARTESIAN_POINT('Ctrl Pts',(19.9688603936049,0.593439717564554,4.20187920587587));
#55533=CARTESIAN_POINT('Ctrl Pts',(19.9529551149173,0.626517665065843,3.97989492921597));
#55534=CARTESIAN_POINT('Ctrl Pts',(19.9370498362297,0.558641803885684,3.79496194153783));
#55535=CARTESIAN_POINT('Ctrl Pts',(19.9211445575421,0.490765942705524,3.61002895385969));
#55536=CARTESIAN_POINT('Ctrl Pts',(19.9052392788545,0.321936272843916,3.46214725516331));
#55537=CARTESIAN_POINT('Ctrl Pts',(19.8893340001669,0.129673778938228,3.41921955761011));
#55538=CARTESIAN_POINT('Ctrl Pts',(19.8734287214793,-0.0625887149674591,
3.37629186005692));
#55539=CARTESIAN_POINT('Ctrl Pts',(19.8575234427916,-0.278284032917226,
3.43831816364691));
#55540=CARTESIAN_POINT('Ctrl Pts',(19.841618164104,-0.418374827314372,3.57681771754473));
#55541=CARTESIAN_POINT('Ctrl Pts',(19.8257128854164,-0.558465621711518,
3.71531727144255));
#55542=CARTESIAN_POINT('Ctrl Pts',(19.8098076067288,-0.622951892556044,
3.9302900756482));
#55543=CARTESIAN_POINT('Ctrl Pts',(19.7939023280412,-0.58222383973146,4.12303018792675));
#55544=CARTESIAN_POINT('Ctrl Pts',(19.7779970493536,-0.541495786906873,
4.3157703002053));
#55545=CARTESIAN_POINT('Ctrl Pts',(19.762091770666,-0.395553410413165,4.48627772055676));
#55546=CARTESIAN_POINT('Ctrl Pts',(19.7461864919784,-0.211407504401025,
4.55626240372308));
#55547=CARTESIAN_POINT('Ctrl Pts',(19.7404061317381,-0.144484459893097,
4.58169651826758));
#55548=CARTESIAN_POINT('Ctrl Pts',(19.7346257714978,-0.0725156072563085,
4.59385388977766));
#55549=CARTESIAN_POINT('Ctrl Pts',(19.7288454112575,-0.000401422265437046,
4.59340756962635));
#55550=CARTESIAN_POINT('Ctrl Pts',(19.6211545887425,0.000364945106097663,
4.59334757974602));
#55551=CARTESIAN_POINT('Ctrl Pts',(19.6310344686986,-0.122924963130536,
4.59265841784648));
#55552=CARTESIAN_POINT('Ctrl Pts',(19.6409143486547,-0.246598186964828,
4.55523353708024));
#55553=CARTESIAN_POINT('Ctrl Pts',(19.6507942286109,-0.346136160298313,
4.48405653351353));
#55554=CARTESIAN_POINT('Ctrl Pts',(19.6666995072985,-0.506378917588675,
4.36947112529969));
#55555=CARTESIAN_POINT('Ctrl Pts',(19.6826047859861,-0.60407113804621,4.16741144784858));
#55556=CARTESIAN_POINT('Ctrl Pts',(19.6985100646737,-0.5943566574826,3.97065479758251));
#55557=CARTESIAN_POINT('Ctrl Pts',(19.7144153433613,-0.584642176918989,
3.77389814731645));
#55558=CARTESIAN_POINT('Ctrl Pts',(19.7303206220489,-0.467520995334232,
3.58244452423543));
#55559=CARTESIAN_POINT('Ctrl Pts',(19.7462259007365,-0.296770260159971,
3.48420125495101));
#55560=CARTESIAN_POINT('Ctrl Pts',(19.7621311794242,-0.12601952498572,3.38595798566659));
#55561=CARTESIAN_POINT('Ctrl Pts',(19.7780364581118,0.098360763778029,3.38092507017875));
#55562=CARTESIAN_POINT('Ctrl Pts',(19.7939417367994,0.27334477570878,3.47141355644931));
#55563=CARTESIAN_POINT('Ctrl Pts',(19.809847015487,0.448328787639532,3.56190204271987));
#55564=CARTESIAN_POINT('Ctrl Pts',(19.8257522941746,0.573916522737285,3.74791193074883));
#55565=CARTESIAN_POINT('Ctrl Pts',(19.8416575728622,0.592443207149574,3.9440350735258));
#55566=CARTESIAN_POINT('Ctrl Pts',(19.8575628515498,0.610969891561863,4.14015821630277));
#55567=CARTESIAN_POINT('Ctrl Pts',(19.8734681302375,0.522435525288687,4.34639461382776));
#55568=CARTESIAN_POINT('Ctrl Pts',(19.8893734089251,0.367491719635661,4.46804975837363));
#55569=CARTESIAN_POINT('Ctrl Pts',(19.8999671355309,0.264291244586565,4.54907828775811));
#55570=CARTESIAN_POINT('Ctrl Pts',(19.9105608621367,0.131629953687138,4.59258455010229));
#55571=CARTESIAN_POINT('Ctrl Pts',(19.9211545887425,-0.000461335262921832,
4.59353843444423));
#55572=CARTESIAN_POINT('Origin',(4.,0.,4.));
#55573=CARTESIAN_POINT('',(20.3288454112575,0.000547175593784699,4.59423670486774));
#55574=CARTESIAN_POINT('',(20.2211545887425,-0.000159442692484791,4.59503650419094));
#55575=CARTESIAN_POINT('',(4.,-7.27562663373442E-17,4.5941));
#55576=CARTESIAN_POINT('Ctrl Pts',(20.3288454112575,0.000547175593784699,
4.59423670486774));
#55577=CARTESIAN_POINT('Ctrl Pts',(20.3254891157492,0.0422991098545892,
4.59465405164581));
#55578=CARTESIAN_POINT('Ctrl Pts',(20.3221328202408,0.0839734681026259,
4.59066114403672));
#55579=CARTESIAN_POINT('Ctrl Pts',(20.3187765247324,0.124636177719752,4.58197547152207));
#55580=CARTESIAN_POINT('Ctrl Pts',(20.3028712460448,0.317334266145104,4.54081460186972));
#55581=CARTESIAN_POINT('Ctrl Pts',(20.2869659673572,0.48731321493246,4.39426577643889));
#55582=CARTESIAN_POINT('Ctrl Pts',(20.2710606886696,0.556778600406793,4.20989870881916));
#55583=CARTESIAN_POINT('Ctrl Pts',(20.255155409982,0.626243985881127,4.02553164119943));
#55584=CARTESIAN_POINT('Ctrl Pts',(20.2392501312944,0.595195808042437,3.80334633139079));
#55585=CARTESIAN_POINT('Ctrl Pts',(20.2233448526068,0.477757630702126,3.64521515909767));
#55586=CARTESIAN_POINT('Ctrl Pts',(20.2074395739191,0.360319453361808,3.48708398680455));
#55587=CARTESIAN_POINT('Ctrl Pts',(20.1915342952315,0.156491276519859,3.39300695202695));
#55588=CARTESIAN_POINT('Ctrl Pts',(20.1756290165439,-0.04006765138094,3.40625706061923));
#55589=CARTESIAN_POINT('Ctrl Pts',(20.1597237378563,-0.236626579281727,
3.4195071692115));
#55590=CARTESIAN_POINT('Ctrl Pts',(20.1438184591687,-0.425916258241364,
3.54008442117362));
#55591=CARTESIAN_POINT('Ctrl Pts',(20.1279131804811,-0.521059912873915,
3.71258420787224));
#55592=CARTESIAN_POINT('Ctrl Pts',(20.1120079017935,-0.616203567506467,
3.88508399457085));
#55593=CARTESIAN_POINT('Ctrl Pts',(20.0961026231058,-0.617201197811932,
4.10950631600596));
#55594=CARTESIAN_POINT('Ctrl Pts',(20.0801973444182,-0.523575121773085,
4.28282745216878));
#55595=CARTESIAN_POINT('Ctrl Pts',(20.0642920657306,-0.429949045734243,
4.45614858833159));
#55596=CARTESIAN_POINT('Ctrl Pts',(20.048386787043,-0.241699263351099,4.57836853922213));
#55597=CARTESIAN_POINT('Ctrl Pts',(20.0324815083554,-0.0452724969876719,
4.59335768007126));
#55598=CARTESIAN_POINT('Ctrl Pts',(20.0312694759895,-0.030304158296608,
4.59449989984645));
#55599=CARTESIAN_POINT('Ctrl Pts',(20.0300574436235,-0.0152883365109376,
4.5950194388496));
#55600=CARTESIAN_POINT('Ctrl Pts',(20.0288454112575,-0.000266600559035268,
4.5949350414008));
#55601=CARTESIAN_POINT('Ctrl Pts',(19.9211545887425,-0.000461335262921832,
4.59353843444423));
#55602=CARTESIAN_POINT('Ctrl Pts',(19.9264661408243,-0.0666901315043342,
4.5940166992278));
#55603=CARTESIAN_POINT('Ctrl Pts',(19.9317776929061,-0.132775635823809,
4.58379778651276));
#55604=CARTESIAN_POINT('Ctrl Pts',(19.9370892449879,-0.194932679790098,
4.56224768701753));
#55605=CARTESIAN_POINT('Ctrl Pts',(19.9529945236755,-0.381060028529917,
4.49771657954882));
#55606=CARTESIAN_POINT('Ctrl Pts',(19.9688998023631,-0.531961480976676,
4.33158047304464));
#55607=CARTESIAN_POINT('Ctrl Pts',(19.9848050810507,-0.578348134104426,
4.14012389605102));
#55608=CARTESIAN_POINT('Ctrl Pts',(20.0007103597384,-0.624734787232175,
3.94866731905739));
#55609=CARTESIAN_POINT('Ctrl Pts',(20.016615638426,-0.566606641040915,3.73189027157431));
#55610=CARTESIAN_POINT('Ctrl Pts',(20.0325209171136,-0.430656211588969,
3.58932409618151));
#55611=CARTESIAN_POINT('Ctrl Pts',(20.0484261958012,-0.294705782137024,
3.44675792078871));
#55612=CARTESIAN_POINT('Ctrl Pts',(20.0643314744888,-0.080933069424392,
3.37840261748619));
#55613=CARTESIAN_POINT('Ctrl Pts',(20.0802367531764,0.112511319004002,3.41565067076361));
#55614=CARTESIAN_POINT('Ctrl Pts',(20.096142031864,0.305955707432406,3.45289872404102));
#55615=CARTESIAN_POINT('Ctrl Pts',(20.1120473105516,0.479071771576571,3.59575013389837));
#55616=CARTESIAN_POINT('Ctrl Pts',(20.1279525892393,0.552362916535151,3.77860107435498));
#55617=CARTESIAN_POINT('Ctrl Pts',(20.1438578679269,0.625654061493722,3.96145201481158));
#55618=CARTESIAN_POINT('Ctrl Pts',(20.1597631466145,0.599120287266732,4.18430248586742));
#55619=CARTESIAN_POINT('Ctrl Pts',(20.1756684253021,0.484961816589866,4.3448525870839));
#55620=CARTESIAN_POINT('Ctrl Pts',(20.1908304797822,0.376137759761604,4.49790047950022));
#55621=CARTESIAN_POINT('Ctrl Pts',(20.2059925342623,0.187686755696174,4.59433432972249));
#55622=CARTESIAN_POINT('Ctrl Pts',(20.2211545887425,-0.000159442692484791,
4.59503650419094));
#55623=CARTESIAN_POINT('Origin',(4.,0.,4.));
#55624=CARTESIAN_POINT('',(20.6288454112575,1.84392275237588E-6,4.59415158619139));
#55625=CARTESIAN_POINT('',(20.5211545887425,0.00014515264107467,4.59408556636595));
#55626=CARTESIAN_POINT('',(4.,-7.27562663373442E-17,4.5941));
#55627=CARTESIAN_POINT('Ctrl Pts',(20.6288454112575,1.84392275237588E-6,
4.59415158619139));
#55628=CARTESIAN_POINT('Ctrl Pts',(20.6209207878748,0.0985777406598016,
4.59414764832452));
#55629=CARTESIAN_POINT('Ctrl Pts',(20.6129961644921,0.197149291092008,4.56908802213256));
#55630=CARTESIAN_POINT('Ctrl Pts',(20.6050715411094,0.283761277174982,4.52200793915563));
#55631=CARTESIAN_POINT('Ctrl Pts',(20.5971189017656,0.370679463050262,4.47476141372331));
#55632=CARTESIAN_POINT('Ctrl Pts',(20.5891662624218,0.445553373684486,4.40533845822152));
#55633=CARTESIAN_POINT('Ctrl Pts',(20.581213623078,0.499196468040806,4.3222224876916));
#55634=CARTESIAN_POINT('Ctrl Pts',(20.5732609837342,0.552839562397126,4.23910651716169));
#55635=CARTESIAN_POINT('Ctrl Pts',(20.5653083443904,0.585251840475543,4.14229753160364));
#55636=CARTESIAN_POINT('Ctrl Pts',(20.5573557050466,0.592531230276538,4.04364021904617));
#55637=CARTESIAN_POINT('Ctrl Pts',(20.5494030657028,0.599810620077534,3.9449829064887));
#55638=CARTESIAN_POINT('Ctrl Pts',(20.541450426359,0.581957121601108,3.84447726693182));
#55639=CARTESIAN_POINT('Ctrl Pts',(20.5334977870152,0.541038843355354,3.75439549632807));
#55640=CARTESIAN_POINT('Ctrl Pts',(20.5255451476714,0.5001205651096,3.66431372572433));
#55641=CARTESIAN_POINT('Ctrl Pts',(20.5175925083276,0.436137507094518,3.58465582407373));
#55642=CARTESIAN_POINT('Ctrl Pts',(20.5096398689838,0.357128912623608,3.5251911792601));
#55643=CARTESIAN_POINT('Ctrl Pts',(20.50168722964,0.278120318152698,3.46572653444646));
#55644=CARTESIAN_POINT('Ctrl Pts',(20.4937345902962,0.184086187225959,3.42645514646979));
#55645=CARTESIAN_POINT('Ctrl Pts',(20.4857819509524,0.0861162623359374,
3.4121221101222));
#55646=CARTESIAN_POINT('Ctrl Pts',(20.4778293116085,-0.0118536625540841,
3.39778907377461));
#55647=CARTESIAN_POINT('Ctrl Pts',(20.4698766722647,-0.113759381407388,
3.4083943890561));
#55648=CARTESIAN_POINT('Ctrl Pts',(20.4619240329209,-0.206384677702653,
3.44274365129583));
#55649=CARTESIAN_POINT('Ctrl Pts',(20.4539713935771,-0.299009973997917,
3.47709291353557));
#55650=CARTESIAN_POINT('Ctrl Pts',(20.4460187542333,-0.382354847735142,
3.53518612273354));
#55651=CARTESIAN_POINT('Ctrl Pts',(20.4380661148895,-0.447563842371028,
3.60976099223211));
#55652=CARTESIAN_POINT('Ctrl Pts',(20.4301134755457,-0.512772837006921,
3.68433586173069));
#55653=CARTESIAN_POINT('Ctrl Pts',(20.4221608362019,-0.559845952541473,
3.77539239152987));
#55654=CARTESIAN_POINT('Ctrl Pts',(20.4142081968581,-0.580888308445953,
3.87190852591559));
#55655=CARTESIAN_POINT('Ctrl Pts',(20.3983029181705,-0.622973020254908,
4.06494079468701));
#55656=CARTESIAN_POINT('Ctrl Pts',(20.3823976394829,-0.5609346935436,4.27981148180459));
#55657=CARTESIAN_POINT('Ctrl Pts',(20.3664923607953,-0.422206916156273,
4.41936036842645));
#55658=CARTESIAN_POINT('Ctrl Pts',(20.353943377616,-0.312753156865475,4.52946196836027));
#55659=CARTESIAN_POINT('Ctrl Pts',(20.3413943944368,-0.155560747392339,
4.59267627084609));
#55660=CARTESIAN_POINT('Ctrl Pts',(20.3288454112575,0.000547175593784699,
4.59423670486774));
#55661=CARTESIAN_POINT('Ctrl Pts',(20.2211545887425,-0.000159442692484791,
4.59503650419094));
#55662=CARTESIAN_POINT('Ctrl Pts',(20.22189781295,-0.00936741923094289,
4.59507092387091));
#55663=CARTESIAN_POINT('Ctrl Pts',(20.2226410371574,-0.0185739425223631,
4.59487531632137));
#55664=CARTESIAN_POINT('Ctrl Pts',(20.2233842613649,-0.0277695625699301,
4.59444507412072));
#55665=CARTESIAN_POINT('Ctrl Pts',(20.2392895400526,-0.224559303926058,
4.58523772856393));
#55666=CARTESIAN_POINT('Ctrl Pts',(20.2551948187402,-0.416355619511548,
4.46857330607325));
#55667=CARTESIAN_POINT('Ctrl Pts',(20.2711000974278,-0.51503297954037,4.29810345018796));
#55668=CARTESIAN_POINT('Ctrl Pts',(20.2870053761154,-0.613710339569191,
4.12763359430267));
#55669=CARTESIAN_POINT('Ctrl Pts',(20.302910654803,-0.619268744041345,3.90335830502277));
#55670=CARTESIAN_POINT('Ctrl Pts',(20.3188159334906,-0.529271009537506,
3.72809546473432));
#55671=CARTESIAN_POINT('Ctrl Pts',(20.3347212121782,-0.439273275033663,
3.55283262444587));
#55672=CARTESIAN_POINT('Ctrl Pts',(20.3506264908658,-0.253719401553817,
3.42658223314887));
#55673=CARTESIAN_POINT('Ctrl Pts',(20.3665317695535,-0.0575887485100287,
3.40762076142476));
#55674=CARTESIAN_POINT('Ctrl Pts',(20.3824370482411,0.138541904533748,3.38865928970065));
#55675=CARTESIAN_POINT('Ctrl Pts',(20.3983423269287,0.345249337141466,3.47698673754941));
#55676=CARTESIAN_POINT('Ctrl Pts',(20.4142476056163,0.467192899405167,3.63141813202173));
#55677=CARTESIAN_POINT('Ctrl Pts',(20.4301528843039,0.589136461668875,3.78584952649406));
#55678=CARTESIAN_POINT('Ctrl Pts',(20.4460581629915,0.626316153588557,4.00638486758996));
#55679=CARTESIAN_POINT('Ctrl Pts',(20.4619634416791,0.562534942182983,4.19337293359078));
#55680=CARTESIAN_POINT('Ctrl Pts',(20.4699160810229,0.530644336480201,4.28686696659118));
#55681=CARTESIAN_POINT('Ctrl Pts',(20.4778687203667,0.473513504946115,4.3719741808178));
#55682=CARTESIAN_POINT('Ctrl Pts',(20.4858213597105,0.400240502138227,4.43864269813793));
#55683=CARTESIAN_POINT('Ctrl Pts',(20.4937739990544,0.326967499330329,4.50531121545807));
#55684=CARTESIAN_POINT('Ctrl Pts',(20.5017266383982,0.237552325248626,4.55354103587171));
#55685=CARTESIAN_POINT('Ctrl Pts',(20.509679277742,0.141619450488441,4.57712494713439));
#55686=CARTESIAN_POINT('Ctrl Pts',(20.5135043814088,0.0954771353210092,
4.58846846487098));
#55687=CARTESIAN_POINT('Ctrl Pts',(20.5173294850756,0.0478269697500401,
4.59411022582368));
#55688=CARTESIAN_POINT('Ctrl Pts',(20.5211545887425,0.00014515264107467,
4.59408556636595));
#55689=CARTESIAN_POINT('Origin',(4.,0.,4.));
#55690=CARTESIAN_POINT('',(20.9288454112575,-6.4040329070536E-6,4.59405282094147));
#55691=CARTESIAN_POINT('',(20.8211545887425,5.65245430726296E-6,4.59414685459231));
#55692=CARTESIAN_POINT('',(4.,-7.27562663373442E-17,4.5941));
#55693=CARTESIAN_POINT('Ctrl Pts',(20.9288454112575,-6.4040329070536E-6,
4.59405282094147));
#55694=CARTESIAN_POINT('Ctrl Pts',(20.9243050993443,0.0564994875152707,
4.59403151438501));
#55695=CARTESIAN_POINT('Ctrl Pts',(20.9197647874311,0.113011285737041,4.58603249222448));
#55696=CARTESIAN_POINT('Ctrl Pts',(20.9152244755179,0.167207550221224,4.57013805289591));
#55697=CARTESIAN_POINT('Ctrl Pts',(20.9072718361741,0.262135685878584,4.5422979516059));
#55698=CARTESIAN_POINT('Ctrl Pts',(20.8993191968303,0.349959832061366,4.49023494241839));
#55699=CARTESIAN_POINT('Ctrl Pts',(20.8913665574865,0.419942299057043,4.42031443844746));
#55700=CARTESIAN_POINT('Ctrl Pts',(20.8834139181427,0.489924766052721,4.35039393447653));
#55701=CARTESIAN_POINT('Ctrl Pts',(20.8754612787989,0.542065553861293,4.26261593572219));
#55702=CARTESIAN_POINT('Ctrl Pts',(20.8675086394551,0.569989725359365,4.16771249585991));
#55703=CARTESIAN_POINT('Ctrl Pts',(20.8595560001113,0.597913896857441,4.07280905599763));
#55704=CARTESIAN_POINT('Ctrl Pts',(20.8516033607674,0.601621452045013,3.97078017502742));
#55705=CARTESIAN_POINT('Ctrl Pts',(20.8436507214236,0.580659121393648,3.87410027737825));
#55706=CARTESIAN_POINT('Ctrl Pts',(20.8356980820798,0.559696790742287,3.77742037972911));
#55707=CARTESIAN_POINT('Ctrl Pts',(20.827745442736,0.514064574252002,3.686089465401));
#55708=CARTESIAN_POINT('Ctrl Pts',(20.8197928033922,0.44934157601673,3.61127397478397));
#55709=CARTESIAN_POINT('Ctrl Pts',(20.8118401640484,0.384618577781443,3.53645848416692));
#55710=CARTESIAN_POINT('Ctrl Pts',(20.8038875247046,0.300804797801161,3.47815841726095));
#55711=CARTESIAN_POINT('Ctrl Pts',(20.7959348853608,0.208147717693743,3.44350176598286));
#55712=CARTESIAN_POINT('Ctrl Pts',(20.787982246017,0.115490637586335,3.40884511470477));
#55713=CARTESIAN_POINT('Ctrl Pts',(20.7800296066732,0.0139902573517945,
3.39783187905454));
#55714=CARTESIAN_POINT('Ctrl Pts',(20.7720769673294,-0.0839438183138644,
3.41180854931868));
#55715=CARTESIAN_POINT('Ctrl Pts',(20.7641243279856,-0.181877893979523,
3.42578521958283));
#55716=CARTESIAN_POINT('Ctrl Pts',(20.7561716886418,-0.2762456650763,3.46475179576135));
#55717=CARTESIAN_POINT('Ctrl Pts',(20.748219049298,-0.355509010203556,3.52394413563581));
#55718=CARTESIAN_POINT('Ctrl Pts',(20.7402664099542,-0.434772355330821,
3.58313647551028));
#55719=CARTESIAN_POINT('Ctrl Pts',(20.7323137706103,-0.498931274488562,
3.66255457908069));
#55720=CARTESIAN_POINT('Ctrl Pts',(20.7243611312665,-0.54014217617541,3.75248840252759));
#55721=CARTESIAN_POINT('Ctrl Pts',(20.7164084919227,-0.581353077862249,
3.84242222597448));
#55722=CARTESIAN_POINT('Ctrl Pts',(20.7084558525789,-0.599615962078206,
3.94287176929784));
#55723=CARTESIAN_POINT('Ctrl Pts',(20.7005032132351,-0.592696601504336,
4.0415558946729));
#55724=CARTESIAN_POINT('Ctrl Pts',(20.6925505738913,-0.585777240930466,
4.14024002004797));
#55725=CARTESIAN_POINT('Ctrl Pts',(20.6845979345475,-0.553675635566762,
4.23715872747472));
#55726=CARTESIAN_POINT('Ctrl Pts',(20.6766452952037,-0.50031917594212,4.32046203197985));
#55727=CARTESIAN_POINT('Ctrl Pts',(20.6686926558599,-0.446962716317479,
4.40376533648498));
#55728=CARTESIAN_POINT('Ctrl Pts',(20.6607400165161,-0.3723514024319,4.47345323806848));
#55729=CARTESIAN_POINT('Ctrl Pts',(20.6527873771723,-0.285602702553558,
4.52100610813718));
#55730=CARTESIAN_POINT('Ctrl Pts',(20.6448347378285,-0.198854002675205,
4.56855897820588));
#55731=CARTESIAN_POINT('Ctrl Pts',(20.6368820984847,-0.099967916804087,
4.59397681675976));
#55732=CARTESIAN_POINT('Ctrl Pts',(20.6289294591409,-0.00104364331035449,
4.59415068835528));
#55733=CARTESIAN_POINT('Ctrl Pts',(20.6289014431798,-0.000695147863829354,
4.59415130087895));
#55734=CARTESIAN_POINT('Ctrl Pts',(20.6288734272186,-0.000346651943377611,
4.59415160011295));
#55735=CARTESIAN_POINT('Ctrl Pts',(20.6288454112575,1.84392275237588E-6,
4.59415158619139));
#55736=CARTESIAN_POINT('Ctrl Pts',(20.5211545887425,0.00014515264107467,
4.59408556636595));
#55737=CARTESIAN_POINT('Ctrl Pts',(20.5252821244194,-0.0513066296901884,
4.59405895720698));
#55738=CARTESIAN_POINT('Ctrl Pts',(20.5294096600964,-0.102795266482965,
4.58743447362686));
#55739=CARTESIAN_POINT('Ctrl Pts',(20.5335371957734,-0.152465997634008,
4.57425651377355));
#55740=CARTESIAN_POINT('Ctrl Pts',(20.5414898351172,-0.248167995557571,
4.5488661670383));
#55741=CARTESIAN_POINT('Ctrl Pts',(20.549442474461,-0.33712141596603,4.49914747145609));
#55742=CARTESIAN_POINT('Ctrl Pts',(20.5573951138048,-0.408848640915227,
4.43107686705031));
#55743=CARTESIAN_POINT('Ctrl Pts',(20.5653477531486,-0.480575865864423,
4.36300626264453));
#55744=CARTESIAN_POINT('Ctrl Pts',(20.5733003924924,-0.535076895354358,
4.27658374941519));
#55745=CARTESIAN_POINT('Ctrl Pts',(20.5812530318362,-0.565476628275392,
4.18243021985824));
#55746=CARTESIAN_POINT('Ctrl Pts',(20.58920567118,-0.595876361196427,4.08827669030129));
#55747=CARTESIAN_POINT('Ctrl Pts',(20.5971583105238,-0.602174797548561,
3.98639214441672));
#55748=CARTESIAN_POINT('Ctrl Pts',(20.6051109498677,-0.58371402745925,3.88920441471463));
#55749=CARTESIAN_POINT('Ctrl Pts',(20.6130635892115,-0.565253257369939,
3.79201668501254));
#55750=CARTESIAN_POINT('Ctrl Pts',(20.6210162285553,-0.522033280839182,
3.69952577149293));
#55751=CARTESIAN_POINT('Ctrl Pts',(20.6289688678991,-0.459278917219465,
3.62305528060961));
#55752=CARTESIAN_POINT('Ctrl Pts',(20.6369215072429,-0.396524553599749,
3.54658478972629));
#55753=CARTESIAN_POINT('Ctrl Pts',(20.6448741465867,-0.314235802891072,
3.48613472147926));
#55754=CARTESIAN_POINT('Ctrl Pts',(20.6528267859305,-0.222505051509483,
3.44908779917463));
#55755=CARTESIAN_POINT('Ctrl Pts',(20.6607794252743,-0.130774300127894,
3.41204087687));
#55756=CARTESIAN_POINT('Ctrl Pts',(20.6687320646181,-0.029601548073392,
3.39839710050778));
#55757=CARTESIAN_POINT('Ctrl Pts',(20.6766847039619,0.0686601223983595,
3.40982890848785));
#55758=CARTESIAN_POINT('Ctrl Pts',(20.6846373433057,0.1669217928701,3.42126071646792));
#55759=CARTESIAN_POINT('Ctrl Pts',(20.6925899826495,0.262272381759091,3.45776810879028));
#55760=CARTESIAN_POINT('Ctrl Pts',(20.7005426219933,0.343045155251024,3.51488528173127));
#55761=CARTESIAN_POINT('Ctrl Pts',(20.7084952613371,0.423817928742975,3.57200245467228));
#55762=CARTESIAN_POINT('Ctrl Pts',(20.7164479006809,0.490012886837861,3.64972940823193));
#55763=CARTESIAN_POINT('Ctrl Pts',(20.7244005400247,0.533541468465666,3.73856417004634));
#55764=CARTESIAN_POINT('Ctrl Pts',(20.7323531793686,0.577070050093471,3.82739893186076));
#55765=CARTESIAN_POINT('Ctrl Pts',(20.7403058187123,0.597932255254196,3.92734150192994));
#55766=CARTESIAN_POINT('Ctrl Pts',(20.7482584580562,0.593574919799613,4.02617190099588));
#55767=CARTESIAN_POINT('Ctrl Pts',(20.7562110974,0.589217584345031,4.1250023000618));
#55768=CARTESIAN_POINT('Ctrl Pts',(20.7641637367438,0.559640708275147,4.22272052812447));
#55769=CARTESIAN_POINT('Ctrl Pts',(20.7721163760876,0.508461778515953,4.30737953925928));
#55770=CARTESIAN_POINT('Ctrl Pts',(20.7800690154314,0.457282848756759,4.39203855039408));
#55771=CARTESIAN_POINT('Ctrl Pts',(20.7880216547752,0.384501865308254,4.46363834460102));
#55772=CARTESIAN_POINT('Ctrl Pts',(20.795974294119,0.299016600344635,4.51342469267633));
#55773=CARTESIAN_POINT('Ctrl Pts',(20.8039269334628,0.213531335381016,4.56321104075164));
#55774=CARTESIAN_POINT('Ctrl Pts',(20.8118795728066,0.115341788902283,4.59118394269532));
#55775=CARTESIAN_POINT('Ctrl Pts',(20.8198322121504,0.0164533379892873,
4.59392342516246));
#55776=CARTESIAN_POINT('Ctrl Pts',(20.8202730043478,0.0109722321971217,
4.59407526688998));
#55777=CARTESIAN_POINT('Ctrl Pts',(20.8207137965451,0.00548897925183007,
4.59414958726715));
#55778=CARTESIAN_POINT('Ctrl Pts',(20.8211545887425,5.65245430726296E-6,
4.59414685459231));
#55779=CARTESIAN_POINT('Origin',(4.,0.,4.));
#55780=CARTESIAN_POINT('',(21.2288454112575,1.28243205298473E-5,4.59412621697841));
#55781=CARTESIAN_POINT('',(21.1211545887425,-1.09306879613159E-5,4.5940621922514));
#55782=CARTESIAN_POINT('',(4.,-7.27562663373442E-17,4.5941));
#55783=CARTESIAN_POINT('Ctrl Pts',(21.2288454112575,1.28243205298473E-5,
4.59412621697841));
#55784=CARTESIAN_POINT('Ctrl Pts',(21.2276894108138,0.0143945780386088,
4.59413985249388));
#55785=CARTESIAN_POINT('Ctrl Pts',(21.2265334103701,0.028775363636007,4.59362827285675));
#55786=CARTESIAN_POINT('Ctrl Pts',(21.2253774099263,0.043117441953227,4.59258471957415));
#55787=CARTESIAN_POINT('Ctrl Pts',(21.2174247705826,0.141782954511012,4.58540565408365));
#55788=CARTESIAN_POINT('Ctrl Pts',(21.2094721312387,0.238616577754522,4.55305001116024));
#55789=CARTESIAN_POINT('Ctrl Pts',(21.2015194918949,0.321779082392626,4.49947370882601));
#55790=CARTESIAN_POINT('Ctrl Pts',(21.1935668525511,0.404941587030731,4.44589740649178));
#55791=CARTESIAN_POINT('Ctrl Pts',(21.1856142132073,0.474432973063433,4.37110044474674));
#55792=CARTESIAN_POINT('Ctrl Pts',(21.1776615738635,0.521756972098598,4.28422777087894));
#55793=CARTESIAN_POINT('Ctrl Pts',(21.1697089345197,0.569080971133768,4.19735509701114));
#55794=CARTESIAN_POINT('Ctrl Pts',(21.1617562951759,0.594237583171398,4.09840671102057));
#55795=CARTESIAN_POINT('Ctrl Pts',(21.1538036558321,0.594151069756079,3.9994804007435));
#55796=CARTESIAN_POINT('Ctrl Pts',(21.1458510164883,0.59406455634076,3.90055409046644));
#55797=CARTESIAN_POINT('Ctrl Pts',(21.1378983771445,0.568734917472505,3.80164985590287));
#55798=CARTESIAN_POINT('Ctrl Pts',(21.1299457378007,0.521259046500119,3.71486008677882));
#55799=CARTESIAN_POINT('Ctrl Pts',(21.1219930984569,0.473783175527722,3.62807031765475));
#55800=CARTESIAN_POINT('Ctrl Pts',(21.114040459113,0.40416107245118,3.5533950139702));
#55801=CARTESIAN_POINT('Ctrl Pts',(21.1060878197692,0.320904987578411,3.49996424865404));
#55802=CARTESIAN_POINT('Ctrl Pts',(21.0981351804254,0.237648902705652,3.44653348333788));
#55803=CARTESIAN_POINT('Ctrl Pts',(21.0901825410817,0.140758836036697,3.41434725639011));
#55804=CARTESIAN_POINT('Ctrl Pts',(21.0822299017378,0.042080917889342,3.40734077242984));
#55805=CARTESIAN_POINT('Ctrl Pts',(21.074277262394,-0.056597000258024,3.40033428846957));
#55806=CARTESIAN_POINT('Ctrl Pts',(21.0663246230502,-0.157062769883762,
3.41850754749682));
#55807=CARTESIAN_POINT('Ctrl Pts',(21.0583719837064,-0.247033082431791,
3.45963862106718));
#55808=CARTESIAN_POINT('Ctrl Pts',(21.0504193443626,-0.337003394979799,
3.50076969463752));
#55809=CARTESIAN_POINT('Ctrl Pts',(21.0424667050188,-0.416478250450111,
3.56485858275095));
#55810=CARTESIAN_POINT('Ctrl Pts',(21.034514065675,-0.475740765152555,3.644069545988));
#55811=CARTESIAN_POINT('Ctrl Pts',(21.0265614263312,-0.535003279855012,
3.72328050922507));
#55812=CARTESIAN_POINT('Ctrl Pts',(21.0186087869874,-0.574053453789596,
3.81761354758578));
#55813=CARTESIAN_POINT('Ctrl Pts',(21.0106561476436,-0.588116871685884,
3.91553516229212));
#55814=CARTESIAN_POINT('Ctrl Pts',(21.0027035082998,-0.60218028958217,4.01345677699845));
#55815=CARTESIAN_POINT('Ctrl Pts',(20.994750868956,-0.591256951440166,4.11496696805043));
#55816=CARTESIAN_POINT('Ctrl Pts',(20.9867982296121,-0.556682383467722,
4.20765473214191));
#55817=CARTESIAN_POINT('Ctrl Pts',(20.9788455902683,-0.522107815495282,
4.30034249623339));
#55818=CARTESIAN_POINT('Ctrl Pts',(20.9708929509246,-0.463882017692404,
4.38420783336438));
#55819=CARTESIAN_POINT('Ctrl Pts',(20.9629403115808,-0.389123888092725,
4.4489970636758));
#55820=CARTESIAN_POINT('Ctrl Pts',(20.9549876722369,-0.314365758493028,
4.51378629398723));
#55821=CARTESIAN_POINT('Ctrl Pts',(20.9470350328931,-0.223075297096518,
4.5594994174791));
#55822=CARTESIAN_POINT('Ctrl Pts',(20.9390823935493,-0.12641400383229,4.58054738252877));
#55823=CARTESIAN_POINT('Ctrl Pts',(20.9356700661187,-0.0849384674446181,
4.58957866703598));
#55824=CARTESIAN_POINT('Ctrl Pts',(20.9322577386881,-0.0424741039190781,
4.59406883414683));
#55825=CARTESIAN_POINT('Ctrl Pts',(20.9288454112575,-6.4040329070536E-6,
4.59405282094147));
#55826=CARTESIAN_POINT('Ctrl Pts',(20.8211545887425,5.65245430726296E-6,
4.59414685459231));
#55827=CARTESIAN_POINT('Ctrl Pts',(20.8286664358889,-0.0934395423672534,
4.59410028517524));
#55828=CARTESIAN_POINT('Ctrl Pts',(20.8361782830354,-0.18690618531264,4.57167601133058));
#55829=CARTESIAN_POINT('Ctrl Pts',(20.8436901301818,-0.270133012248912,
4.529191754035));
#55830=CARTESIAN_POINT('Ctrl Pts',(20.8516427695256,-0.358243556226857,
4.4842145374498));
#55831=CARTESIAN_POINT('Ctrl Pts',(20.8595954088694,-0.434877288835492,
4.41675404128879));
#55832=CARTESIAN_POINT('Ctrl Pts',(20.8675480482133,-0.490664589397756,
4.33505825661903));
#55833=CARTESIAN_POINT('Ctrl Pts',(20.8755006875571,-0.546451889960021,
4.25336247194927));
#55834=CARTESIAN_POINT('Ctrl Pts',(20.8834533269009,-0.581392758475918,
4.15743139877076));
#55835=CARTESIAN_POINT('Ctrl Pts',(20.8914059662447,-0.591215252505097,
4.05899390323763));
#55836=CARTESIAN_POINT('Ctrl Pts',(20.8993586055885,-0.601037746534278,
3.96055640770449));
#55837=CARTESIAN_POINT('Ctrl Pts',(20.9073112449323,-0.585741866076735,
3.85961248981672));
#55838=CARTESIAN_POINT('Ctrl Pts',(20.9152638842761,-0.547197711916726,
3.76850392583047));
#55839=CARTESIAN_POINT('Ctrl Pts',(20.9232165236199,-0.508653557756717,
3.67739536184422));
#55840=CARTESIAN_POINT('Ctrl Pts',(20.9311691629637,-0.446861129894262,
3.59612215175949));
#55841=CARTESIAN_POINT('Ctrl Pts',(20.9391218023075,-0.369375409551539,
3.53462104847409));
#55842=CARTESIAN_POINT('Ctrl Pts',(20.9470744416513,-0.291889689208826,
3.4731199451887));
#55843=CARTESIAN_POINT('Ctrl Pts',(20.9550270809951,-0.198710676385865,
3.43139094870266));
#55844=CARTESIAN_POINT('Ctrl Pts',(20.9629797203389,-0.101230766359376,
3.41453599926792));
#55845=CARTESIAN_POINT('Ctrl Pts',(20.9709323596827,-0.00375085633288601,
3.39768104983318));
#55846=CARTESIAN_POINT('Ctrl Pts',(20.9788849990265,0.0980299508971346,
3.40570014744973));
#55847=CARTESIAN_POINT('Ctrl Pts',(20.9868376383704,0.191667561123074,3.43761284710704));
#55848=CARTESIAN_POINT('Ctrl Pts',(20.9947902777142,0.285305171349014,3.46952554676435));
#55849=CARTESIAN_POINT('Ctrl Pts',(21.002742917058,0.37079958457088,3.52533184846243));
#55850=CARTESIAN_POINT('Ctrl Pts',(21.0106955564018,0.437697946637459,3.59820867233944));
#55851=CARTESIAN_POINT('Ctrl Pts',(21.0186481957456,0.504596308704037,3.67108549621644));
#55852=CARTESIAN_POINT('Ctrl Pts',(21.0266008350894,0.552898619615334,3.76103284227238));
#55853=CARTESIAN_POINT('Ctrl Pts',(21.0345534744332,0.576699262792956,3.8570534220826));
#55854=CARTESIAN_POINT('Ctrl Pts',(21.042506113777,0.600499905970578,3.95307400189282));
#55855=CARTESIAN_POINT('Ctrl Pts',(21.0504587531208,0.599798881414527,4.05516781545734));
#55856=CARTESIAN_POINT('Ctrl Pts',(21.0584113924646,0.574681899562831,4.15085250374278));
#55857=CARTESIAN_POINT('Ctrl Pts',(21.0663640318084,0.549564917711138,4.24653719202821));
#55858=CARTESIAN_POINT('Ctrl Pts',(21.0743166711522,0.500031978563804,4.33581275503458));
#55859=CARTESIAN_POINT('Ctrl Pts',(21.082269310496,0.432139158218639,4.40776403918836));
#55860=CARTESIAN_POINT('Ctrl Pts',(21.0902219498398,0.364246337873458,4.47971532334216));
#55861=CARTESIAN_POINT('Ctrl Pts',(21.0981745891836,0.277993636330433,4.53434232864337));
#55862=CARTESIAN_POINT('Ctrl Pts',(21.1061272285274,0.183926621270441,4.56496615973523));
#55863=CARTESIAN_POINT('Ctrl Pts',(21.1111363485991,0.124676735433976,4.5842551580617));
#55864=CARTESIAN_POINT('Ctrl Pts',(21.1161454686708,0.0623266393968894,
4.59402126159141));
#55865=CARTESIAN_POINT('Ctrl Pts',(21.1211545887425,-1.09306879613159E-5,
4.5940621922514));
#55866=CARTESIAN_POINT('Origin',(4.,0.,4.));
#55867=CARTESIAN_POINT('',(21.5288454112575,-1.51073027558624E-5,4.59408477831653));
#55868=CARTESIAN_POINT('',(21.4211545887425,1.51733402061755E-5,4.59410821609125));
#55869=CARTESIAN_POINT('',(4.,-7.27562663373442E-17,4.5941));
#55870=CARTESIAN_POINT('Ctrl Pts',(21.5288454112575,-1.51073027558624E-5,
4.59408477831653));
#55871=CARTESIAN_POINT('Ctrl Pts',(21.5231210829395,0.0712153309254728,
4.59401644885886));
#55872=CARTESIAN_POINT('Ctrl Pts',(21.5173967546214,0.142469702059594,4.58119587380047));
#55873=CARTESIAN_POINT('Ctrl Pts',(21.5116724263034,0.209120766622247,4.55613331912479));
#55874=CARTESIAN_POINT('Ctrl Pts',(21.5037197869596,0.301717111362981,4.52131465616629));
#55875=CARTESIAN_POINT('Ctrl Pts',(21.4957671476158,0.385428743083265,4.46286809139133));
#55876=CARTESIAN_POINT('Ctrl Pts',(21.4878145082719,0.450020774675764,4.38793951336988));
#55877=CARTESIAN_POINT('Ctrl Pts',(21.4798618689281,0.514612806268249,4.31301093534845));
#55878=CARTESIAN_POINT('Ctrl Pts',(21.4719092295843,0.560085237732952,4.22160034408054));
#55879=CARTESIAN_POINT('Ctrl Pts',(21.4639565902405,0.58087844500124,4.1248839293359));
#55880=CARTESIAN_POINT('Ctrl Pts',(21.4560039508967,0.601671652269532,4.02816751459124));
#55881=CARTESIAN_POINT('Ctrl Pts',(21.4480513115529,0.597785635341394,3.92614527636987));
#55882=CARTESIAN_POINT('Ctrl Pts',(21.4400986722091,0.569695512712777,3.83129082280931));
#55883=CARTESIAN_POINT('Ctrl Pts',(21.4321460328653,0.541605390084162,3.73643636924876));
#55884=CARTESIAN_POINT('Ctrl Pts',(21.4241933935215,0.489311161755075,3.64874970034904));
#55885=CARTESIAN_POINT('Ctrl Pts',(21.4162407541777,0.419206509371839,3.57895170565158));
#55886=CARTESIAN_POINT('Ctrl Pts',(21.4082881148339,0.349101856988603,3.50915371095413));
#55887=CARTESIAN_POINT('Ctrl Pts',(21.4003354754901,0.261186780551223,3.45724439045894));
#55888=CARTESIAN_POINT('Ctrl Pts',(21.3923828361463,0.16621009553345,3.42957036558731));
#55889=CARTESIAN_POINT('Ctrl Pts',(21.3844301968025,0.0712334105156764,
3.40189634071567));
#55890=CARTESIAN_POINT('Ctrl Pts',(21.3764775574587,-0.0308048830825163,
3.3984576114676));
#55891=CARTESIAN_POINT('Ctrl Pts',(21.3685249181149,-0.127429214135013,
3.41967460932821));
#55892=CARTESIAN_POINT('Ctrl Pts',(21.360572278771,-0.22405354518751,3.44089160718882));
#55893=CARTESIAN_POINT('Ctrl Pts',(21.3526196394272,-0.315263913694308,
3.4867643321581));
#55894=CARTESIAN_POINT('Ctrl Pts',(21.3446670000834,-0.389908609845283,
3.5516842188346));
#55895=CARTESIAN_POINT('Ctrl Pts',(21.3367143607396,-0.464553305996249,
3.6166041055111));
#55896=CARTESIAN_POINT('Ctrl Pts',(21.3287617213958,-0.522632329791381,
3.70057115389483));
#55897=CARTESIAN_POINT('Ctrl Pts',(21.320809082052,-0.557044729551177,3.79331924871262));
#55898=CARTESIAN_POINT('Ctrl Pts',(21.3128564427082,-0.591457129310977,
3.88606734353042));
#55899=CARTESIAN_POINT('Ctrl Pts',(21.3049038033644,-0.602202905035458,
3.9875964847823));
#55900=CARTESIAN_POINT('Ctrl Pts',(21.2969511640206,-0.587968239287942,
4.08549335215105));
#55901=CARTESIAN_POINT('Ctrl Pts',(21.2889985246768,-0.573733573540424,
4.18339021951981));
#55902=CARTESIAN_POINT('Ctrl Pts',(21.281045885333,-0.534518466320906,4.27765481300544));
#55903=CARTESIAN_POINT('Ctrl Pts',(21.2730932459892,-0.47511749858569,4.35676200219639));
#55904=CARTESIAN_POINT('Ctrl Pts',(21.2651406066454,-0.415716530850488,
4.43586919138732));
#55905=CARTESIAN_POINT('Ctrl Pts',(21.2571879673016,-0.336129702599601,
4.49981897628356));
#55906=CARTESIAN_POINT('Ctrl Pts',(21.2492353279577,-0.246087587538132,
4.54079262470289));
#55907=CARTESIAN_POINT('Ctrl Pts',(21.2424386890577,-0.169134048541188,
4.57581031891556));
#55908=CARTESIAN_POINT('Ctrl Pts',(21.2356420501576,-0.0845438791841879,
4.59404604774026));
#55909=CARTESIAN_POINT('Ctrl Pts',(21.2288454112575,1.28243205298473E-5,
4.59412621697841));
#55910=CARTESIAN_POINT('Ctrl Pts',(21.1211545887425,-1.09306879613159E-5,
4.5940621922514));
#55911=CARTESIAN_POINT('Ctrl Pts',(21.1240981080146,-0.0366424819978743,
4.5940862444172));
#55912=CARTESIAN_POINT('Ctrl Pts',(21.1270416272867,-0.0732697079540161,
4.59075208378119));
#55913=CARTESIAN_POINT('Ctrl Pts',(21.1299851465589,-0.109260984540888,
4.58401866488291));
#55914=CARTESIAN_POINT('Ctrl Pts',(21.1379377859027,-0.20650024671525,4.56582668205621));
#55915=CARTESIAN_POINT('Ctrl Pts',(21.1458904252465,-0.299097442487026,
4.52282205952027));
#55916=CARTESIAN_POINT('Ctrl Pts',(21.1538430645903,-0.375731303474415,
4.46026269810429));
#55917=CARTESIAN_POINT('Ctrl Pts',(21.1617957039341,-0.452365164461805,
4.3977033366883));
#55918=CARTESIAN_POINT('Ctrl Pts',(21.1697483432779,-0.513035690664809,
4.31558923639226));
#55919=CARTESIAN_POINT('Ctrl Pts',(21.1777009826217,-0.550325083965727,
4.22395996434209));
#55920=CARTESIAN_POINT('Ctrl Pts',(21.1856536219655,-0.587614477266646,
4.13233069229192));
#55921=CARTESIAN_POINT('Ctrl Pts',(21.1936062613093,-0.601522737665479,
4.03118624848761));
#55922=CARTESIAN_POINT('Ctrl Pts',(21.2015589006531,-0.590349390887683,
3.93289291874755));
#55923=CARTESIAN_POINT('Ctrl Pts',(21.2095115399969,-0.579176044109886,
3.83459958900749));
#55924=CARTESIAN_POINT('Ctrl Pts',(21.2174641793407,-0.542921090155459,
3.73915737333167));
#55925=CARTESIAN_POINT('Ctrl Pts',(21.2254168186845,-0.486017190935348,
3.65823538248142));
#55926=CARTESIAN_POINT('Ctrl Pts',(21.2333694580283,-0.429113291715238,
3.57731339163117));
#55927=CARTESIAN_POINT('Ctrl Pts',(21.2413220973721,-0.351560447229444,
3.51091162560648));
#55928=CARTESIAN_POINT('Ctrl Pts',(21.249274736716,-0.262840548960938,3.46714860467879));
#55929=CARTESIAN_POINT('Ctrl Pts',(21.2572273760598,-0.174120650692433,
3.4233855837511));
#55930=CARTESIAN_POINT('Ctrl Pts',(21.2651800154036,-0.0742336986412151,
3.40226130792041));
#55931=CARTESIAN_POINT('Ctrl Pts',(21.2731326547474,0.0246077668693877,
3.40635850761334));
#55932=CARTESIAN_POINT('Ctrl Pts',(21.2810852940912,0.123449232380002,3.41045570730627));
#55933=CARTESIAN_POINT('Ctrl Pts',(21.289037933435,0.221245211350001,3.43977438252282));
#55934=CARTESIAN_POINT('Ctrl Pts',(21.2969905727788,0.306038813396919,3.49072992590572));
#55935=CARTESIAN_POINT('Ctrl Pts',(21.3049432121226,0.390832415443818,3.54168546928862));
#55936=CARTESIAN_POINT('Ctrl Pts',(21.3128958514664,0.462623640567642,3.61427788083785));
#55937=CARTESIAN_POINT('Ctrl Pts',(21.3208484908102,0.512635033719562,3.69963174955258));
#55938=CARTESIAN_POINT('Ctrl Pts',(21.328801130154,0.562646426871494,3.78498561826733));
#55939=CARTESIAN_POINT('Ctrl Pts',(21.3367537694978,0.590877988051513,3.88310094414759));
#55940=CARTESIAN_POINT('Ctrl Pts',(21.3447064088416,0.59387802439953,3.98198179230066));
#55941=CARTESIAN_POINT('Ctrl Pts',(21.3526590481854,0.596878060747546,4.08086264045372));
#55942=CARTESIAN_POINT('Ctrl Pts',(21.3606116875293,0.574646572263566,4.1805090108796));
#55943=CARTESIAN_POINT('Ctrl Pts',(21.3685643268731,0.529901661201384,4.26873777763737));
#55944=CARTESIAN_POINT('Ctrl Pts',(21.3765169662169,0.485156750139203,4.35696654439514));
#55945=CARTESIAN_POINT('Ctrl Pts',(21.3844696055607,0.417898416498819,4.4337777074848));
#55946=CARTESIAN_POINT('Ctrl Pts',(21.3924222449045,0.336349907607971,4.48978005607163));
#55947=CARTESIAN_POINT('Ctrl Pts',(21.4003748842483,0.254801398717122,4.54578240465847));
#55948=CARTESIAN_POINT('Ctrl Pts',(21.4083275235921,0.158962714575808,4.58097593874246));
#55949=CARTESIAN_POINT('Ctrl Pts',(21.4162801629359,0.0605514396169286,
4.59105776945554));
#55950=CARTESIAN_POINT('Ctrl Pts',(21.4179049715381,0.0404449719157324,
4.59311759444699));
#55951=CARTESIAN_POINT('Ctrl Pts',(21.4195297801403,0.0202311170044278,
4.59412918598148));
#55952=CARTESIAN_POINT('Ctrl Pts',(21.4211545887425,1.51733402061755E-5,
4.59410821609125));
#55953=CARTESIAN_POINT('Origin',(4.,0.,4.));
#55954=CARTESIAN_POINT('',(21.8288454112575,1.47252919898561E-5,4.59408074293421));
#55955=CARTESIAN_POINT('',(21.7211545887425,-1.54601956517634E-5,4.59410286710644));
#55956=CARTESIAN_POINT('',(4.,-7.27562663373442E-17,4.5941));
#55957=CARTESIAN_POINT('Ctrl Pts',(21.8288454112575,1.47252919898561E-5,
4.59408074293421));
#55958=CARTESIAN_POINT('Ctrl Pts',(21.826505394409,0.0291331941223908,4.59410767674242));
#55959=CARTESIAN_POINT('Ctrl Pts',(21.8241653775604,0.0582478076928112,
4.59200528777341));
#55960=CARTESIAN_POINT('Ctrl Pts',(21.8218253607118,0.0870422430987805,
4.58774093918134));
#55961=CARTESIAN_POINT('Ctrl Pts',(21.813872721368,0.184901264939656,4.57324838268129));
#55962=CARTESIAN_POINT('Ctrl Pts',(21.8059200820242,0.279062206656402,4.53378504179028));
#55963=CARTESIAN_POINT('Ctrl Pts',(21.7979674426804,0.358012610677869,4.47417584741217));
#55964=CARTESIAN_POINT('Ctrl Pts',(21.7900148033366,0.436963014699336,4.41456665303406));
#55965=CARTESIAN_POINT('Ctrl Pts',(21.7820621639928,0.500702881025523,4.33481160516884));
#55966=CARTESIAN_POINT('Ctrl Pts',(21.774109524649,0.541439142878506,4.24466184465998));
#55967=CARTESIAN_POINT('Ctrl Pts',(21.7661568853052,0.58217540473149,4.15451208415111));
#55968=CARTESIAN_POINT('Ctrl Pts',(21.7582042459614,0.599908062111268,4.0539676109986));
#55969=CARTESIAN_POINT('Ctrl Pts',(21.7502516066176,0.59246905613922,3.95532135643358));
#55970=CARTESIAN_POINT('Ctrl Pts',(21.7422989672738,0.585030050167171,3.85667510186855));
#55971=CARTESIAN_POINT('Ctrl Pts',(21.73434632793,0.552419380843296,3.759927065891));
#55972=CARTESIAN_POINT('Ctrl Pts',(21.7263936885861,0.498624146640836,3.67690601358098));
#55973=CARTESIAN_POINT('Ctrl Pts',(21.7184410492423,0.444828912438376,3.59388496127097));
#55974=CARTESIAN_POINT('Ctrl Pts',(21.7104884098985,0.369849113357332,3.52459089262848));
#55975=CARTESIAN_POINT('Ctrl Pts',(21.7025357705547,0.28285205103972,3.47749595131133));
#55976=CARTESIAN_POINT('Ctrl Pts',(21.6945831312109,0.195854988722108,3.43040100999418));
#55977=CARTESIAN_POINT('Ctrl Pts',(21.6866304918671,0.0968406631679286,
3.40550519600236));
#55978=CARTESIAN_POINT('Ctrl Pts',(21.6786778525233,-0.00208507577578169,
3.40585236167057));
#55979=CARTESIAN_POINT('Ctrl Pts',(21.6707252131795,-0.101010814719503,
3.40619952733877));
#55980=CARTESIAN_POINT('Ctrl Pts',(21.6627725738357,-0.199847967052756,
3.431789672667));
#55981=CARTESIAN_POINT('Ctrl Pts',(21.6548199344919,-0.28651234476781,3.47949405385809));
#55982=CARTESIAN_POINT('Ctrl Pts',(21.6468672951481,-0.373176722482865,
3.52719843504918));
#55983=CARTESIAN_POINT('Ctrl Pts',(21.6389146558043,-0.44766832557972,3.59701705210314));
#55984=CARTESIAN_POINT('Ctrl Pts',(21.6309620164605,-0.500879541024521,
3.68041362817464));
#55985=CARTESIAN_POINT('Ctrl Pts',(21.6230093771167,-0.55409075646931,3.76381020424612));
#55986=CARTESIAN_POINT('Ctrl Pts',(21.6150567377728,-0.586021584262053,
3.86078473933514));
#55987=CARTESIAN_POINT('Ctrl Pts',(21.607104098429,-0.592768045815946,3.95948077576042));
#55988=CARTESIAN_POINT('Ctrl Pts',(21.5991514590852,-0.599514507369841,
4.05817681218572));
#55989=CARTESIAN_POINT('Ctrl Pts',(21.5911988197414,-0.581076602684875,
4.15859434994728));
#55990=CARTESIAN_POINT('Ctrl Pts',(21.5832461803976,-0.539708616728004,
4.24845597739434));
#55991=CARTESIAN_POINT('Ctrl Pts',(21.5752935410538,-0.498340630771147,
4.33831760484137));
#55992=CARTESIAN_POINT('Ctrl Pts',(21.56734090171,-0.434042563542403,4.41762332197391));
#55993=CARTESIAN_POINT('Ctrl Pts',(21.5593882623662,-0.354675729482573,
4.47667692475034));
#55994=CARTESIAN_POINT('Ctrl Pts',(21.5514356230224,-0.275308895422716,
4.53573052752678));
#55995=CARTESIAN_POINT('Ctrl Pts',(21.5434829836786,-0.180873294531764,
4.57453201594709));
#55996=CARTESIAN_POINT('Ctrl Pts',(21.5355303443348,-0.0829149652056982,
4.58833737958621));
#55997=CARTESIAN_POINT('Ctrl Pts',(21.533302033309,-0.055467269432644,4.59220561033096));
#55998=CARTESIAN_POINT('Ctrl Pts',(21.5310737222833,-0.0277430016607059,
4.5941113769453));
#55999=CARTESIAN_POINT('Ctrl Pts',(21.5288454112575,-1.51073027558624E-5,
4.59408477831653));
#56000=CARTESIAN_POINT('Ctrl Pts',(21.4211545887425,1.51733402061755E-5,
4.59410821609125));
#56001=CARTESIAN_POINT('Ctrl Pts',(21.4274824194841,-0.0787159889745399,
4.59402654867773));
#56002=CARTESIAN_POINT('Ctrl Pts',(21.4338102502257,-0.15747883181342,4.57828382012605));
#56003=CARTESIAN_POINT('Ctrl Pts',(21.4401380809673,-0.230053504748576,
4.54780575811717));
#56004=CARTESIAN_POINT('Ctrl Pts',(21.4480907203111,-0.321263308378747,
4.50950178872359));
#56005=CARTESIAN_POINT('Ctrl Pts',(21.4560433596549,-0.402699049862651,
4.44792372259427));
#56006=CARTESIAN_POINT('Ctrl Pts',(21.4639959989987,-0.464404100671371,
4.37060031698995));
#56007=CARTESIAN_POINT('Ctrl Pts',(21.4719486383425,-0.526109151480106,
4.2932769113856));
#56008=CARTESIAN_POINT('Ctrl Pts',(21.4799012776864,-0.568083511613643,
4.20020816630624));
#56009=CARTESIAN_POINT('Ctrl Pts',(21.4878539170302,-0.585195243866348,
4.10277300340868));
#56010=CARTESIAN_POINT('Ctrl Pts',(21.495806556374,-0.602306976119048,4.00533784051114));
#56011=CARTESIAN_POINT('Ctrl Pts',(21.5037591957178,-0.594556080490919,
3.90353625979537));
#56012=CARTESIAN_POINT('Ctrl Pts',(21.5117118350616,-0.562890209537588,
3.80981489101362));
#56013=CARTESIAN_POINT('Ctrl Pts',(21.5196644744054,-0.53122433858425,3.71609352223184));
#56014=CARTESIAN_POINT('Ctrl Pts',(21.5276171137492,-0.47564349230572,3.63045236538409));
#56015=CARTESIAN_POINT('Ctrl Pts',(21.535569753093,-0.402943186155437,3.56336221830407));
#56016=CARTESIAN_POINT('Ctrl Pts',(21.5435223924368,-0.330242880005154,
3.49627207122406));
#56017=CARTESIAN_POINT('Ctrl Pts',(21.5514750317806,-0.24042311398314,3.44773293391182));
#56018=CARTESIAN_POINT('Ctrl Pts',(21.5594276711244,-0.144465577806233,
3.42367937699355));
#56019=CARTESIAN_POINT('Ctrl Pts',(21.5673803104682,-0.0485080416293372,
3.39962582007528));
#56020=CARTESIAN_POINT('Ctrl Pts',(21.575332949812,0.0535872647024426,3.40005784355098));
#56021=CARTESIAN_POINT('Ctrl Pts',(21.5832855891558,0.149337799479898,3.42492262666669));
#56022=CARTESIAN_POINT('Ctrl Pts',(21.5912382284996,0.245088334257342,3.44978740978241));
#56023=CARTESIAN_POINT('Ctrl Pts',(21.5991908678434,0.33449409748049,3.49908495253815));
#56024=CARTESIAN_POINT('Ctrl Pts',(21.6071435071872,0.406624016913212,3.56678795891296));
#56025=CARTESIAN_POINT('Ctrl Pts',(21.6150961465311,0.478753936345942,3.63449096528778));
#56026=CARTESIAN_POINT('Ctrl Pts',(21.6230487858749,0.533608011988269,3.72059943528167));
#56027=CARTESIAN_POINT('Ctrl Pts',(21.6310014252187,0.564479585995414,3.81458543566408));
#56028=CARTESIAN_POINT('Ctrl Pts',(21.6389540645625,0.595351160002559,3.90857143604649));
#56029=CARTESIAN_POINT('Ctrl Pts',(21.6469067039063,0.602240232374519,4.0104349668174));
#56030=CARTESIAN_POINT('Ctrl Pts',(21.6548593432501,0.584304520186539,4.10772182398666));
#56031=CARTESIAN_POINT('Ctrl Pts',(21.6628119825939,0.566368807998562,4.2050086811559));
#56032=CARTESIAN_POINT('Ctrl Pts',(21.6707646219377,0.523608311250652,4.29771886472347));
#56033=CARTESIAN_POINT('Ctrl Pts',(21.6787172612815,0.461251083056512,4.37451729206089));
#56034=CARTESIAN_POINT('Ctrl Pts',(21.6866699006253,0.398893854862358,4.45131571939834));
#56035=CARTESIAN_POINT('Ctrl Pts',(21.6946225399691,0.316939895221968,4.51220239050563));
#56036=CARTESIAN_POINT('Ctrl Pts',(21.7025751793129,0.225409191891896,4.54973308058009));
#56037=CARTESIAN_POINT('Ctrl Pts',(21.7087683157894,0.15412944274098,4.5789601931952));
#56038=CARTESIAN_POINT('Ctrl Pts',(21.7149614522659,0.0770418275534371,
4.59402294959611));
#56039=CARTESIAN_POINT('Ctrl Pts',(21.7211545887425,-1.54601956517634E-5,
4.59410286710644));
#56040=CARTESIAN_POINT('Origin',(4.,0.,4.));
#56041=CARTESIAN_POINT('',(22.1288454112575,-1.19684274697274E-5,4.59413016891312));
#56042=CARTESIAN_POINT('',(22.0211545887425,1.20066176157995E-5,4.59406577061205));
#56043=CARTESIAN_POINT('',(4.,-7.27562663373442E-17,4.5941));
#56044=CARTESIAN_POINT('Ctrl Pts',(22.1288454112575,-1.19684274697274E-5,
4.59413016891312));
#56045=CARTESIAN_POINT('Ctrl Pts',(22.1219370665346,0.0859328098890183,
4.59405244111828));
#56046=CARTESIAN_POINT('Ctrl Pts',(22.1150287218117,0.171910584533005,4.57519344187135));
#56047=CARTESIAN_POINT('Ctrl Pts',(22.1081203770888,0.24987714748571,4.53905210772026));
#56048=CARTESIAN_POINT('Ctrl Pts',(22.100167737745,0.339629466009183,4.49744749656716));
#56049=CARTESIAN_POINT('Ctrl Pts',(22.0922150984012,0.418765494330909,4.4329406966096));
#56050=CARTESIAN_POINT('Ctrl Pts',(22.0842624590574,0.477609775176754,4.35341854270704));
#56051=CARTESIAN_POINT('Ctrl Pts',(22.0763098197136,0.536454056022584,4.2738963888045));
#56052=CARTESIAN_POINT('Ctrl Pts',(22.0683571803698,0.575006589392542,4.17935888095698));
#56053=CARTESIAN_POINT('Ctrl Pts',(22.060404541026,0.588553803007579,4.081364517074));
#56054=CARTESIAN_POINT('Ctrl Pts',(22.0524519016822,0.60210101662262,3.983370153191));
#56055=CARTESIAN_POINT('Ctrl Pts',(22.0444992623384,0.590642910482727,3.88191893327255));
#56056=CARTESIAN_POINT('Ctrl Pts',(22.0365466229946,0.55558039411957,3.78941465069146));
#56057=CARTESIAN_POINT('Ctrl Pts',(22.0285939836508,0.520517877756421,3.69691036811039));
#56058=CARTESIAN_POINT('Ctrl Pts',(22.020641344307,0.461850951170019,3.61335302286667));
#56059=CARTESIAN_POINT('Ctrl Pts',(22.0126887049632,0.386752445163155,3.5489586384446));
#56060=CARTESIAN_POINT('Ctrl Pts',(22.0047360656194,0.311653939156274,3.48456425402251));
#56061=CARTESIAN_POINT('Ctrl Pts',(21.9967834262756,0.220123853728924,3.43933283042207));
#56062=CARTESIAN_POINT('Ctrl Pts',(21.9888307869318,0.123352988439278,3.41879452521803));
#56063=CARTESIAN_POINT('Ctrl Pts',(21.980878147588,0.0265821231496428,3.398256220014));
#56064=CARTESIAN_POINT('Ctrl Pts',(21.9729255082441,-0.075429522002288,
3.40241103320635));
#56065=CARTESIAN_POINT('Ctrl Pts',(21.9649728689003,-0.170209634025949,
3.43075098229493));
#56066=CARTESIAN_POINT('Ctrl Pts',(21.9570202295565,-0.26498974604961,3.4590909313835));
#56067=CARTESIAN_POINT('Ctrl Pts',(21.9490675902127,-0.352538324945002,
3.5116160163683));
#56068=CARTESIAN_POINT('Ctrl Pts',(21.9411149508689,-0.422151364554475,
3.58190433023263));
#56069=CARTESIAN_POINT('Ctrl Pts',(21.9331623115251,-0.491764404163956,
3.65219264409696));
#56070=CARTESIAN_POINT('Ctrl Pts',(21.9252096721813,-0.543441904487514,
3.74024418684083));
#56071=CARTESIAN_POINT('Ctrl Pts',(21.9172570328375,-0.570865587277161,
3.83529345812586));
#56072=CARTESIAN_POINT('Ctrl Pts',(21.9093043934937,-0.598289270066803,
3.93034272941087));
#56073=CARTESIAN_POINT('Ctrl Pts',(21.9013517541499,-0.601459135322544,
4.03238972923704));
#56074=CARTESIAN_POINT('Ctrl Pts',(21.8933991148061,-0.579987623844179,
4.12895782202339));
#56075=CARTESIAN_POINT('Ctrl Pts',(21.8854464754623,-0.558516112365809,
4.22552591480976));
#56076=CARTESIAN_POINT('Ctrl Pts',(21.8774938361185,-0.512403224153321,
4.31661510055631));
#56077=CARTESIAN_POINT('Ctrl Pts',(21.8695411967747,-0.447286887835617,
4.39108848569571));
#56078=CARTESIAN_POINT('Ctrl Pts',(21.8615885574308,-0.38217055151792,4.46556187083511));
#56079=CARTESIAN_POINT('Ctrl Pts',(21.853635918087,-0.298050767095013,4.52341945536736));
#56080=CARTESIAN_POINT('Ctrl Pts',(21.8456832787432,-0.205212323901057,
4.55758736157894));
#56081=CARTESIAN_POINT('Ctrl Pts',(21.840070656248,-0.139691040693493,4.58170156451555));
#56082=CARTESIAN_POINT('Ctrl Pts',(21.8344580337528,-0.0698270680627233,
4.59401614113532));
#56083=CARTESIAN_POINT('Ctrl Pts',(21.8288454112575,1.47252919898561E-5,
4.59408074293421));
#56084=CARTESIAN_POINT('Ctrl Pts',(21.7211545887425,-1.54601956517634E-5,
4.59410286710644));
#56085=CARTESIAN_POINT('Ctrl Pts',(21.7229140916097,-0.0219078436841643,
4.59412557209431));
#56086=CARTESIAN_POINT('Ctrl Pts',(21.724673594477,-0.0437977792686499,
4.59293892497318));
#56087=CARTESIAN_POINT('Ctrl Pts',(21.7264330973443,-0.0655513867134097,
4.59052415646896));
#56088=CARTESIAN_POINT('Ctrl Pts',(21.7343857366881,-0.163873814968881,
4.57960983324176));
#56089=CARTESIAN_POINT('Ctrl Pts',(21.742338376032,-0.259411224460086,4.54360647774573));
#56090=CARTESIAN_POINT('Ctrl Pts',(21.7502910153758,-0.340482865683332,
4.48691599054611));
#56091=CARTESIAN_POINT('Ctrl Pts',(21.7582436547196,-0.421554506906578,
4.4302255033465));
#56092=CARTESIAN_POINT('Ctrl Pts',(21.7661962940634,-0.488160379861865,
4.3528478844433));
#56093=CARTESIAN_POINT('Ctrl Pts',(21.7741489334072,-0.532157009426634,
4.26424360160945));
#56094=CARTESIAN_POINT('Ctrl Pts',(21.782101572751,-0.576153638991403,4.1756393187756));
#56095=CARTESIAN_POINT('Ctrl Pts',(21.7900542120948,-0.597541025165654,
4.0758083720111));
#56096=CARTESIAN_POINT('Ctrl Pts',(21.7980068514386,-0.593704268699233,
3.9769564542281));
#56097=CARTESIAN_POINT('Ctrl Pts',(21.8059594907824,-0.589867512232813,
3.87810453644509));
#56098=CARTESIAN_POINT('Ctrl Pts',(21.8139121301262,-0.560806613125721,
3.78023164764359));
#56099=CARTESIAN_POINT('Ctrl Pts',(21.82186476947,-0.510074662095298,3.69530408148155));
#56100=CARTESIAN_POINT('Ctrl Pts',(21.8298174088138,-0.459342711064876,
3.61037651531951));
#56101=CARTESIAN_POINT('Ctrl Pts',(21.8377700481576,-0.386939708111122,
3.53839427179695));
#56102=CARTESIAN_POINT('Ctrl Pts',(21.8457226875014,-0.301717906454235,
3.48815816056295));
#56103=CARTESIAN_POINT('Ctrl Pts',(21.8536753268452,-0.216496104797349,
3.43792204932895));
#56104=CARTESIAN_POINT('Ctrl Pts',(21.8616279661891,-0.118455504437329,
3.40943207038352));
#56105=CARTESIAN_POINT('Ctrl Pts',(21.8695806055329,-0.0195829040543552,
3.40617151167847));
#56106=CARTESIAN_POINT('Ctrl Pts',(21.8775332448767,0.0792896963286298,
3.40291095297342));
#56107=CARTESIAN_POINT('Ctrl Pts',(21.8854858842205,0.178994296734569,3.42487981450875));
#56108=CARTESIAN_POINT('Ctrl Pts',(21.8934385235643,0.267340651814441,3.46939210375187));
#56109=CARTESIAN_POINT('Ctrl Pts',(21.9013911629081,0.355687006894294,3.51390439299499));
#56110=CARTESIAN_POINT('Ctrl Pts',(21.9093438022519,0.432675116648084,3.58096010994589));
#56111=CARTESIAN_POINT('Ctrl Pts',(21.9172964415957,0.488892136101412,3.66236077992681));
#56112=CARTESIAN_POINT('Ctrl Pts',(21.9252490809395,0.545109155554752,3.74376144990775));
#56113=CARTESIAN_POINT('Ctrl Pts',(21.9332017202833,0.580555084707621,3.8395070729187));
#56114=CARTESIAN_POINT('Ctrl Pts',(21.9411543596271,0.590896175957217,3.93789144251738));
#56115=CARTESIAN_POINT('Ctrl Pts',(21.9491069989709,0.601237267206812,4.03627581211605));
#56116=CARTESIAN_POINT('Ctrl Pts',(21.9570596383147,0.58647352055314,4.13729892830245));
#56117=CARTESIAN_POINT('Ctrl Pts',(21.9650122776585,0.548410005102802,4.22860933921557));
#56118=CARTESIAN_POINT('Ctrl Pts',(21.9729649170023,0.510346489652465,4.31991975012869));
#56119=CARTESIAN_POINT('Ctrl Pts',(21.9809175563462,0.448983205405461,4.40151745576853));
#56120=CARTESIAN_POINT('Ctrl Pts',(21.98887019569,0.371822649612145,4.46342602528218));
#56121=CARTESIAN_POINT('Ctrl Pts',(21.9968228350338,0.29466209381883,4.52533459479583));
#56122=CARTESIAN_POINT('Ctrl Pts',(22.0047754743776,0.201704266479203,4.5675540281833));
#56123=CARTESIAN_POINT('Ctrl Pts',(22.0127281137214,0.104314528045707,4.58492242469582));
#56124=CARTESIAN_POINT('Ctrl Pts',(22.0155369387284,0.069917050565085,4.59105683924014));
#56125=CARTESIAN_POINT('Ctrl Pts',(22.0183457637354,0.0349667096964542,
4.59409118517947));
#56126=CARTESIAN_POINT('Ctrl Pts',(22.0211545887425,1.20066176157995E-5,
4.59406577061205));
#56127=CARTESIAN_POINT('Origin',(4.,0.,4.));
#56128=CARTESIAN_POINT('',(22.4288454112575,5.18920962550018E-6,4.59405135764298));
#56129=CARTESIAN_POINT('',(22.3211545887424,-7.30827440488969E-6,4.59414400810326));
#56130=CARTESIAN_POINT('',(4.,-7.27562663373442E-17,4.5941));
#56131=CARTESIAN_POINT('Ctrl Pts',(22.4288454112575,5.18920962550018E-6,
4.59405135764298));
#56132=CARTESIAN_POINT('Ctrl Pts',(22.4253213780041,0.0438634191921666,
4.5940647188338));
#56133=CARTESIAN_POINT('Ctrl Pts',(22.4217973447507,0.0877187745911938,
4.589273164082));
#56134=CARTESIAN_POINT('Ctrl Pts',(22.4182733114973,0.130485535360993,4.57964583089408));
#56135=CARTESIAN_POINT('Ctrl Pts',(22.4103206721535,0.226996720088313,4.55791995512033));
#56136=CARTESIAN_POINT('Ctrl Pts',(22.4023680328097,0.317964089339764,4.51156722320365));
#56137=CARTESIAN_POINT('Ctrl Pts',(22.3944153934659,0.392265646131591,4.44625488916104));
#56138=CARTESIAN_POINT('Ctrl Pts',(22.3864627541221,0.4665672029234,4.38094255511845));
#56139=CARTESIAN_POINT('Ctrl Pts',(22.3785101147783,0.524202947255594,4.29667061894994));
#56140=CARTESIAN_POINT('Ctrl Pts',(22.3705574754345,0.558126122886914,4.20374247196213));
#56141=CARTESIAN_POINT('Ctrl Pts',(22.3626048360906,0.592049298518242,4.11081432497429));
#56142=CARTESIAN_POINT('Ctrl Pts',(22.3546521967468,0.602259905448686,4.00922996716717));
#56143=CARTESIAN_POINT('Ctrl Pts',(22.346699557403,0.587509558716917,3.91140947017845));
#56144=CARTESIAN_POINT('Ctrl Pts',(22.3387469180592,0.572759211985149,3.81358897318973));
#56145=CARTESIAN_POINT('Ctrl Pts',(22.3307942787154,0.533047911591167,3.71953233701942));
#56146=CARTESIAN_POINT('Ctrl Pts',(22.3228416393716,0.473230904440663,3.6407392662825));
#56147=CARTESIAN_POINT('Ctrl Pts',(22.3148890000278,0.413413897290173,3.5619461955456));
#56148=CARTESIAN_POINT('Ctrl Pts',(22.306936360684,0.333491183383171,3.49841669024209));
#56149=CARTESIAN_POINT('Ctrl Pts',(22.2989837213402,0.243234403245124,3.45791809774646));
#56150=CARTESIAN_POINT('Ctrl Pts',(22.2910310819964,0.152977623107077,3.41741950525082));
#56151=CARTESIAN_POINT('Ctrl Pts',(22.2830784426526,0.0523867767379842,
3.39995182556307));
#56152=CARTESIAN_POINT('Ctrl Pts',(22.2751258033088,-0.0462395349927855,
3.40765072037886));
#56153=CARTESIAN_POINT('Ctrl Pts',(22.267173163965,-0.144865846723578,3.41534961519466));
#56154=CARTESIAN_POINT('Ctrl Pts',(22.2592205246212,-0.241527623816046,
3.448215084514));
#56155=CARTESIAN_POINT('Ctrl Pts',(22.2512678852774,-0.324406647450603,
3.50222887712101));
#56156=CARTESIAN_POINT('Ctrl Pts',(22.2433152459336,-0.40728567108515,3.55624266972802));
#56157=CARTESIAN_POINT('Ctrl Pts',(22.2353626065897,-0.476381941261788,
3.63140478562268));
#56158=CARTESIAN_POINT('Ctrl Pts',(22.2274099672459,-0.523247497912515,
3.71852563243507));
#56159=CARTESIAN_POINT('Ctrl Pts',(22.2194573279021,-0.570113054563243,
3.80564647924745));
#56160=CARTESIAN_POINT('Ctrl Pts',(22.2115046885583,-0.59474789768806,3.90472605697756));
#56161=CARTESIAN_POINT('Ctrl Pts',(22.2035520492145,-0.594140082177443,
4.00365053781872));
#56162=CARTESIAN_POINT('Ctrl Pts',(22.1955994098707,-0.593532266666827,
4.10257501865988));
#56163=CARTESIAN_POINT('Ctrl Pts',(22.1876467705269,-0.567681792520777,
4.2013444026121));
#56164=CARTESIAN_POINT('Ctrl Pts',(22.1796941311831,-0.519749232289404,
4.2878827872712));
#56165=CARTESIAN_POINT('Ctrl Pts',(22.1717414918393,-0.471816672058032,
4.37442117193029));
#56166=CARTESIAN_POINT('Ctrl Pts',(22.1637888524955,-0.401802025741336,
4.44872855729627));
#56167=CARTESIAN_POINT('Ctrl Pts',(22.1558362131517,-0.318265537426909,
4.50171985346399));
#56168=CARTESIAN_POINT('Ctrl Pts',(22.1478835738079,-0.234729049112483,
4.55471114963171));
#56169=CARTESIAN_POINT('Ctrl Pts',(22.1399309344641,-0.137670718800326,
4.58638635660118));
#56170=CARTESIAN_POINT('Ctrl Pts',(22.1319782951203,-0.0389572492816432,
4.5928727489116));
#56171=CARTESIAN_POINT('Ctrl Pts',(22.1309340004994,-0.0259947671705595,
4.5937245044491));
#56172=CARTESIAN_POINT('Ctrl Pts',(22.1298897058784,-0.0130037447923657,
4.5941419185755));
#56173=CARTESIAN_POINT('Ctrl Pts',(22.1288454112575,-1.19684274697274E-5,
4.59413016891312));
#56174=CARTESIAN_POINT('Ctrl Pts',(22.0211545887425,1.20066176157995E-5,
4.59406577061205));
#56175=CARTESIAN_POINT('Ctrl Pts',(22.0262984030792,-0.064000704172389,
4.59401922879619));
#56176=CARTESIAN_POINT('Ctrl Pts',(22.031442217416,-0.128028044405449,4.5837112392356));
#56177=CARTESIAN_POINT('Ctrl Pts',(22.0365860317528,-0.188701337098646,
4.56338935830438));
#56178=CARTESIAN_POINT('Ctrl Pts',(22.0445386710966,-0.282505814282095,
4.53197053576284));
#56179=CARTESIAN_POINT('Ctrl Pts',(22.0524913104404,-0.368293119121642,
4.4766155310422));
#56180=CARTESIAN_POINT('Ctrl Pts',(22.0604439497842,-0.435574585201076,
4.40409224738955));
#56181=CARTESIAN_POINT('Ctrl Pts',(22.068396589128,-0.502856051280518,4.33156896373689));
#56182=CARTESIAN_POINT('Ctrl Pts',(22.0763492284718,-0.551631678599843,
4.24187740115222));
#56183=CARTESIAN_POINT('Ctrl Pts',(22.0843018678156,-0.575937982408454,
4.14598357473613));
#56184=CARTESIAN_POINT('Ctrl Pts',(22.0922545071594,-0.600244286217068,
4.05008974832002));
#56185=CARTESIAN_POINT('Ctrl Pts',(22.1002071465032,-0.600081266514962,
3.94799365807249));
#56186=CARTESIAN_POINT('Ctrl Pts',(22.1081597858471,-0.575468854681199,
3.85217794154701));
#56187=CARTESIAN_POINT('Ctrl Pts',(22.1161124251909,-0.550856442847438,
3.75636222502155));
#56188=CARTESIAN_POINT('Ctrl Pts',(22.1240650645347,-0.501794638882025,
3.66682688221814));
#56189=CARTESIAN_POINT('Ctrl Pts',(22.1320177038785,-0.434281916527717,
3.5945188282416));
#56190=CARTESIAN_POINT('Ctrl Pts',(22.1399703432223,-0.366769194173409,
3.52221077426505));
#56191=CARTESIAN_POINT('Ctrl Pts',(22.1479229825661,-0.280805553430205,
3.46713000911538));
#56192=CARTESIAN_POINT('Ctrl Pts',(22.1558756219099,-0.186901220180937,
3.43601090651668));
#56193=CARTESIAN_POINT('Ctrl Pts',(22.1638282612537,-0.0929968869316588,
3.40489180391798));
#56194=CARTESIAN_POINT('Ctrl Pts',(22.1717809005975,0.00884813882368474,
3.39773436387026));
#56195=CARTESIAN_POINT('Ctrl Pts',(22.1797335399413,0.106181915586414,3.41541368090248));
#56196=CARTESIAN_POINT('Ctrl Pts',(22.1876861792851,0.203515692349121,3.4330929979347));
#56197=CARTESIAN_POINT('Ctrl Pts',(22.1956388186289,0.296338220119215,3.47560907204686));
#56198=CARTESIAN_POINT('Ctrl Pts',(22.2035914579727,0.373300680656879,3.53776373412001));
#56199=CARTESIAN_POINT('Ctrl Pts',(22.2115440973165,0.450263141194552,3.59991839619317));
#56200=CARTESIAN_POINT('Ctrl Pts',(22.2194967366603,0.511365534499791,3.68171164622733));
#56201=CARTESIAN_POINT('Ctrl Pts',(22.2274493760041,0.549137260797828,3.7731431454068));
#56202=CARTESIAN_POINT('Ctrl Pts',(22.2354020153479,0.586908987095865,3.86457464458628));
#56203=CARTESIAN_POINT('Ctrl Pts',(22.2433546546918,0.6013500463867,3.96564439291107));
#56204=CARTESIAN_POINT('Ctrl Pts',(22.2513072940356,0.590694822479903,4.06399523710107));
#56205=CARTESIAN_POINT('Ctrl Pts',(22.2592599333794,0.580039598573106,4.16234608129106));
#56206=CARTESIAN_POINT('Ctrl Pts',(22.2672125727232,0.544288091468676,4.25797802134625));
#56207=CARTESIAN_POINT('Ctrl Pts',(22.275165212067,0.487811409852587,4.33919875012361));
#56208=CARTESIAN_POINT('Ctrl Pts',(22.2831178514108,0.431334728236497,4.42041947890096));
#56209=CARTESIAN_POINT('Ctrl Pts',(22.2910704907546,0.354132872108749,4.48722899640046));
#56210=CARTESIAN_POINT('Ctrl Pts',(22.2990231300984,0.265644819817582,4.53145892916239));
#56211=CARTESIAN_POINT('Ctrl Pts',(22.3064002829798,0.183560135512932,4.57248819778762));
#56212=CARTESIAN_POINT('Ctrl Pts',(22.3137774358611,0.0917635873240076,
4.59408754951618));
#56213=CARTESIAN_POINT('Ctrl Pts',(22.3211545887424,-7.30827440488969E-6,
4.59414400810326));
#56214=CARTESIAN_POINT('Origin',(4.,0.,4.));
#56215=CARTESIAN_POINT('',(22.7288454112575,-7.11440487624268E-7,4.59414971000239));
#56216=CARTESIAN_POINT('',(22.6211545887425,-1.51245797256638E-7,4.59404869726453));
#56217=CARTESIAN_POINT('',(4.,-7.27562663373442E-17,4.5941));
#56218=CARTESIAN_POINT('Ctrl Pts',(22.7288454112575,-7.11440487624268E-7,
4.59414971000239));
#56219=CARTESIAN_POINT('Ctrl Pts',(22.7287056894736,0.0017373052546791,
4.59414999869406));
#56220=CARTESIAN_POINT('Ctrl Pts',(22.7285659676897,0.0034753215591825,
4.59414251282321));
#56221=CARTESIAN_POINT('Ctrl Pts',(22.7284262459057,0.00521327185949689,
4.59412723628209));
#56222=CARTESIAN_POINT('Ctrl Pts',(22.7204736065619,0.104133365400505,4.59325773105135));
#56223=CARTESIAN_POINT('Ctrl Pts',(22.7125209672181,0.202839630323109,4.56714939948764));
#56224=CARTESIAN_POINT('Ctrl Pts',(22.7045683278743,0.289252680684759,4.51898953373575));
#56225=CARTESIAN_POINT('Ctrl Pts',(22.6966156885305,0.375665731046408,4.47082966798385));
#56226=CARTESIAN_POINT('Ctrl Pts',(22.6886630491867,0.449785566847107,4.40061826804377));
#56227=CARTESIAN_POINT('Ctrl Pts',(22.6807104098429,0.502555912967013,4.31694216252228));
#56228=CARTESIAN_POINT('Ctrl Pts',(22.6727577704991,0.555326259086918,4.23326605700079));
#56229=CARTESIAN_POINT('Ctrl Pts',(22.6648051311553,0.586747115526033,4.13612524589788));
#56230=CARTESIAN_POINT('Ctrl Pts',(22.6568524918115,0.592973744123511,4.03739517928057));
#56231=CARTESIAN_POINT('Ctrl Pts',(22.6488998524677,0.59920037272099,3.93866511266326));
#56232=CARTESIAN_POINT('Ctrl Pts',(22.6409472131239,0.580232773476834,3.83834579053153));
#56233=CARTESIAN_POINT('Ctrl Pts',(22.6329945737801,0.538391640361539,3.74870332422701));
#56234=CARTESIAN_POINT('Ctrl Pts',(22.6250419344363,0.496550507246239,3.65906085792248));
#56235=CARTESIAN_POINT('Ctrl Pts',(22.6170892950925,0.431835840259791,3.58009524744515));
#56236=CARTESIAN_POINT('Ctrl Pts',(22.6091366557487,0.35215901686313,3.52146073929621));
#56237=CARTESIAN_POINT('Ctrl Pts',(22.6011840164048,0.272482193466486,3.46282623114728));
#56238=CARTESIAN_POINT('Ctrl Pts',(22.593231377061,0.17784321365963,3.42452282532672));
#56239=CARTESIAN_POINT('Ctrl Pts',(22.5852787377172,0.0798134434713266,
3.41123383340666));
#56240=CARTESIAN_POINT('Ctrl Pts',(22.5773260983734,-0.0182163267169884,
3.3979448414866));
#56241=CARTESIAN_POINT('Ctrl Pts',(22.5693734590296,-0.119636887286728,
3.40967026346704));
#56242=CARTESIAN_POINT('Ctrl Pts',(22.5614208196858,-0.212048437952692,
3.44497640167274));
#56243=CARTESIAN_POINT('Ctrl Pts',(22.553468180342,-0.304459988618666,3.48028253987845));
#56244=CARTESIAN_POINT('Ctrl Pts',(22.5455155409982,-0.387862529380837,
3.53916939430943));
#56245=CARTESIAN_POINT('Ctrl Pts',(22.5375629016544,-0.452058834188948,
3.61443730067171));
#56246=CARTESIAN_POINT('Ctrl Pts',(22.5296102623106,-0.516255138997059,
3.689705207034));
#56247=CARTESIAN_POINT('Ctrl Pts',(22.5216576229668,-0.561245207851117,
3.7813541653276));
#56248=CARTESIAN_POINT('Ctrl Pts',(22.513704983623,-0.581528460676763,3.87817881267738));
#56249=CARTESIAN_POINT('Ctrl Pts',(22.5057523442792,-0.601811713502406,
3.97500346002715));
#56250=CARTESIAN_POINT('Ctrl Pts',(22.4977997049354,-0.597388150299644,
4.07700379643311));
#56251=CARTESIAN_POINT('Ctrl Pts',(22.4898470655916,-0.568798575589296,
4.17170890717095));
#56252=CARTESIAN_POINT('Ctrl Pts',(22.4818944262477,-0.540209000878948,
4.26641401790879));
#56253=CARTESIAN_POINT('Ctrl Pts',(22.4739417869039,-0.487453414661012,
4.35382390297851));
#56254=CARTESIAN_POINT('Ctrl Pts',(22.4659891475601,-0.416981925106977,
4.42325150516024));
#56255=CARTESIAN_POINT('Ctrl Pts',(22.4580365082163,-0.346510435552941,
4.49267910734197));
#56256=CARTESIAN_POINT('Ctrl Pts',(22.4500838688725,-0.258323042662803,
4.54412442663572));
#56257=CARTESIAN_POINT('Ctrl Pts',(22.4421312295287,-0.163201846116148,
4.57129757646718));
#56258=CARTESIAN_POINT('Ctrl Pts',(22.4377026234383,-0.11023146834083,4.58642955613285));
#56259=CARTESIAN_POINT('Ctrl Pts',(22.4332740173479,-0.0551108697057404,
4.59403456681078));
#56260=CARTESIAN_POINT('Ctrl Pts',(22.4288454112575,5.18920962550018E-6,
4.59405135764298));
#56261=CARTESIAN_POINT('Ctrl Pts',(22.3211545887424,-7.30827440488969E-6,
4.59414400810326));
#56262=CARTESIAN_POINT('Ctrl Pts',(22.3217300752049,-0.00716629073194701,
4.59414841239758));
#56263=CARTESIAN_POINT('Ctrl Pts',(22.3223055616673,-0.0143251170819474,
4.59402171850555));
#56264=CARTESIAN_POINT('Ctrl Pts',(22.3228810481298,-0.0214791647150919,
4.59376292335171));
#56265=CARTESIAN_POINT('Ctrl Pts',(22.3308336874736,-0.120340848501978,
4.59018663675477));
#56266=CARTESIAN_POINT('Ctrl Pts',(22.3387863268174,-0.218289967621164,
4.56138371553656));
#56267=CARTESIAN_POINT('Ctrl Pts',(22.3467389661612,-0.303350908332583,
4.51087570903952));
#56268=CARTESIAN_POINT('Ctrl Pts',(22.3546916055051,-0.388411849044011,
4.46036770254246));
#56269=CARTESIAN_POINT('Ctrl Pts',(22.3626442448489,-0.460584611347669,
4.38815461076656));
#56270=CARTESIAN_POINT('Ctrl Pts',(22.3705968841927,-0.511045091866278,
4.3030654678256));
#56271=CARTESIAN_POINT('Ctrl Pts',(22.3785495235365,-0.561505572384874,
4.21797632488466));
#56272=CARTESIAN_POINT('Ctrl Pts',(22.3865021628803,-0.590253771118432,
4.12001113077866));
#56273=CARTESIAN_POINT('Ctrl Pts',(22.3944548022241,-0.593774829630164,
4.02114746451658));
#56274=CARTESIAN_POINT('Ctrl Pts',(22.4024074415679,-0.597295888141896,
3.92228379825449));
#56275=CARTESIAN_POINT('Ctrl Pts',(22.4103600809117,-0.575589806431797,
3.82252165983632));
#56276=CARTESIAN_POINT('Ctrl Pts',(22.4183127202555,-0.531310447862662,
3.73405832985033));
#56277=CARTESIAN_POINT('Ctrl Pts',(22.4262653595993,-0.487031089293526,
3.64559499986435));
#56278=CARTESIAN_POINT('Ctrl Pts',(22.4342179989431,-0.420178453865353,
3.56843047831055));
#56279=CARTESIAN_POINT('Ctrl Pts',(22.4421706382869,-0.338926188203527,
3.51199917808983));
#56280=CARTESIAN_POINT('Ctrl Pts',(22.4501232776307,-0.257673922541701,
3.45556787786912));
#56281=CARTESIAN_POINT('Ctrl Pts',(22.4580759169745,-0.162022026646223,
3.41986979898149));
#56282=CARTESIAN_POINT('Ctrl Pts',(22.4660285563183,-0.0636652448434586,
3.40926951931498));
#56283=CARTESIAN_POINT('Ctrl Pts',(22.4739811956621,0.0346915369593057,
3.39866923964846));
#56284=CARTESIAN_POINT('Ctrl Pts',(22.4819338350059,0.135753204669356,3.41316675920307));
#56285=CARTESIAN_POINT('Ctrl Pts',(22.4898864743497,0.227163587879617,3.45098955584192));
#56286=CARTESIAN_POINT('Ctrl Pts',(22.4978391136936,0.318573971089878,3.48881235248077));
#56287=CARTESIAN_POINT('Ctrl Pts',(22.5057917530374,0.40033306980035,3.54996042620388));
#56288=CARTESIAN_POINT('Ctrl Pts',(22.5137443923812,0.462444730281743,3.62695759769032));
#56289=CARTESIAN_POINT('Ctrl Pts',(22.521697031725,0.524556390763143,3.70395476917678));
#56290=CARTESIAN_POINT('Ctrl Pts',(22.5296496710688,0.567020613015458,3.79680103842659));
#56291=CARTESIAN_POINT('Ctrl Pts',(22.5376023104126,0.584645549343987,3.89414467407578));
#56292=CARTESIAN_POINT('Ctrl Pts',(22.5455549497564,0.602270485672515,3.99148830972497));
#56293=CARTESIAN_POINT('Ctrl Pts',(22.5535075891002,0.595056136077256,4.09332931177355));
#56294=CARTESIAN_POINT('Ctrl Pts',(22.561460228444,0.563884587368514,4.18721625032571));
#56295=CARTESIAN_POINT('Ctrl Pts',(22.5694128677878,0.532713038659782,4.28110318887784));
#56296=CARTESIAN_POINT('Ctrl Pts',(22.5773655071316,0.477584290837583,4.36703606393356));
#56297=CARTESIAN_POINT('Ctrl Pts',(22.5853181464754,0.405238519368296,4.43450837402952));
#56298=CARTESIAN_POINT('Ctrl Pts',(22.5932707858192,0.332892747898984,4.5019806841255));
#56299=CARTESIAN_POINT('Ctrl Pts',(22.601223425163,0.24332995278257,4.55099242926169));
#56300=CARTESIAN_POINT('Ctrl Pts',(22.6091760645068,0.14750052788588,4.57555132613148));
#56301=CARTESIAN_POINT('Ctrl Pts',(22.6131689059187,0.0993867282199646,
4.58788179608141));
#56302=CARTESIAN_POINT('Ctrl Pts',(22.6171617473306,0.0496932250345643,
4.5940481472271));
#56303=CARTESIAN_POINT('Ctrl Pts',(22.6211545887425,-1.51173456864708E-7,
4.59404872180247));
#56304=CARTESIAN_POINT('Origin',(3.42660065607856,0.,4.));
#56305=CARTESIAN_POINT('',(22.7766006560786,-4.98014040841517E-7,4.41590979742004));
#56306=CARTESIAN_POINT('',(22.8,4.87367679877478E-13,4.415875));
#56307=CARTESIAN_POINT('',(3.42660065607856,4.87367679877478E-13,4.415875));
#56308=CARTESIAN_POINT('',(22.8,-0.195748955928421,4.36692555359082));
#56309=CARTESIAN_POINT('Ctrl Pts',(22.7766006560786,-4.98014040834069E-7,
4.41590979742004));
#56310=CARTESIAN_POINT('Ctrl Pts',(22.7844004373857,-0.0679170312443507,
4.41589851620688));
#56311=CARTESIAN_POINT('Ctrl Pts',(22.7922002186928,-0.135834416676695,
4.39892762624317));
#56312=CARTESIAN_POINT('Ctrl Pts',(22.8,-0.195762566582618,4.36695865185838));
#56313=CARTESIAN_POINT('Origin',(22.8,0.,4.));
#56314=CARTESIAN_POINT('Origin',(3.42660065607856,0.,4.));
#56315=CARTESIAN_POINT('',(22.4766006560785,3.63249072247605E-6,4.41584094994071));
#56316=CARTESIAN_POINT('',(22.5733993439214,-1.05822049303872E-7,4.41583910483016));
#56317=CARTESIAN_POINT('',(3.42660065607856,4.87367679877478E-13,4.415875));
#56318=CARTESIAN_POINT('Ctrl Pts',(22.4766006560785,3.63249072248342E-6,
4.41584094994071));
#56319=CARTESIAN_POINT('Ctrl Pts',(22.4810292621689,-0.0385780726118879,
4.41582919621688));
#56320=CARTESIAN_POINT('Ctrl Pts',(22.4934105076031,-0.146451497349971,
4.40094585736882));
#56321=CARTESIAN_POINT('Ctrl Pts',(22.5137443923812,-0.304292138366774,
4.30886736509782));
#56322=CARTESIAN_POINT('Ctrl Pts',(22.5376023104126,-0.415080201412036,
4.12530439950267));
#56323=CARTESIAN_POINT('Ctrl Pts',(22.561460228444,-0.424369795825249,3.91110111771763));
#56324=CARTESIAN_POINT('Ctrl Pts',(22.5853181464754,-0.329889515310188,
3.71863599132299));
#56325=CARTESIAN_POINT('Ctrl Pts',(22.6091760645068,-0.154742073939436,
3.59497211022641));
#56326=CARTESIAN_POINT('Ctrl Pts',(22.6330339825383,0.0582436639512456,
3.57034842802071));
#56327=CARTESIAN_POINT('Ctrl Pts',(22.6568919005697,0.256987911016647,3.65078654733876));
#56328=CARTESIAN_POINT('Ctrl Pts',(22.6807498186011,0.39289034562191,3.81661632308649));
#56329=CARTESIAN_POINT('Ctrl Pts',(22.7046077366325,0.432722782933869,4.02728943245291));
#56330=CARTESIAN_POINT('Ctrl Pts',(22.7284656546639,0.366738191089385,4.2312875884069));
#56331=CARTESIAN_POINT('Ctrl Pts',(22.7523235726953,0.211084664509997,4.37873330099785));
#56332=CARTESIAN_POINT('Ctrl Pts',(22.7683685731669,0.0716802821347026,
4.41560650088387));
#56333=CARTESIAN_POINT('Ctrl Pts',(22.7764609342946,0.00121612829983627,
4.41590999950663));
#56334=CARTESIAN_POINT('Ctrl Pts',(22.7766006560786,-4.98014040834069E-7,
4.41590979742004));
#56335=CARTESIAN_POINT('',(22.8,0.415641328671541,4.01393920819689));
#56336=CARTESIAN_POINT('Origin',(22.8,0.,4.));
#56337=CARTESIAN_POINT('Ctrl Pts',(22.5733993439214,-1.0582204931428E-7,
4.41583910483016));
#56338=CARTESIAN_POINT('Ctrl Pts',(22.5773591418533,-0.034498011376554,
4.41583950370926));
#56339=CARTESIAN_POINT('Ctrl Pts',(22.5892715791291,-0.138279341065089,
4.40307041914735));
#56340=CARTESIAN_POINT('Ctrl Pts',(22.6091366557487,-0.295063722636797,
4.31769517074077));
#56341=CARTESIAN_POINT('Ctrl Pts',(22.6329945737801,-0.411209141905604,
4.13747522778479));
#56342=CARTESIAN_POINT('Ctrl Pts',(22.6568524918115,-0.426804986482714,
3.92363755172126));
#56343=CARTESIAN_POINT('Ctrl Pts',(22.6807104098429,-0.33803111495158,3.72847502015617));
#56344=CARTESIAN_POINT('Ctrl Pts',(22.7045683278743,-0.16660749730952,3.59970312177549));
#56345=CARTESIAN_POINT('Ctrl Pts',(22.7284262459057,0.0455714674079685,
3.56882345794434));
#56346=CARTESIAN_POINT('Ctrl Pts',(22.7522841639372,0.246577802732478,3.64336153500176));
#56347=CARTESIAN_POINT('Ctrl Pts',(22.7761420819686,0.387346815298129,3.80514019809748));
#56348=CARTESIAN_POINT('Ctrl Pts',(22.7920473606562,0.417963038852713,3.94471011778788));
#56349=CARTESIAN_POINT('Ctrl Pts',(22.8,0.415641328671541,4.01393920819689));
#56350=CARTESIAN_POINT('Origin',(3.42660065607856,0.,4.));
#56351=CARTESIAN_POINT('',(22.1766006560786,-8.37799962078257E-6,4.41589611849309));
#56352=CARTESIAN_POINT('',(22.2733993439214,-5.11585294796223E-6,4.41590580604266));
#56353=CARTESIAN_POINT('',(3.42660065607856,4.87367679877478E-13,4.415875));
#56354=CARTESIAN_POINT('Ctrl Pts',(22.1766006560786,-8.37799962077716E-6,
4.41589611849309));
#56355=CARTESIAN_POINT('Ctrl Pts',(22.1776449506995,-0.0091027307950905,
4.41590434335565));
#56356=CARTESIAN_POINT('Ctrl Pts',(22.1866418846642,-0.0874489573854402,
4.4133870032437));
#56357=CARTESIAN_POINT('Ctrl Pts',(22.2035914579727,-0.232253957950086,
4.36612956178204));
#56358=CARTESIAN_POINT('Ctrl Pts',(22.2274493760041,-0.379286482964224,
4.21008217638027));
#56359=CARTESIAN_POINT('Ctrl Pts',(22.2513072940356,-0.433573131350875,
4.00266397632408));
#56360=CARTESIAN_POINT('Ctrl Pts',(22.275165212067,-0.381839338801546,3.79459436150246));
#56361=CARTESIAN_POINT('Ctrl Pts',(22.2990231300984,-0.236735426869051,
3.63675202040985));
#56362=CARTESIAN_POINT('Ctrl Pts',(22.3228810481298,-0.0337432544318164,
3.56773370504276));
#56363=CARTESIAN_POINT('Ctrl Pts',(22.3467389661613,0.177500062688638,3.60441627341574));
#56364=CARTESIAN_POINT('Ctrl Pts',(22.3705968841926,0.345339779804043,3.73782983856348));
#56365=CARTESIAN_POINT('Ctrl Pts',(22.3944548022241,0.428734513273282,3.93535114928888));
#56366=CARTESIAN_POINT('Ctrl Pts',(22.4183127202555,0.407291980919218,4.1486808655136));
#56367=CARTESIAN_POINT('Ctrl Pts',(22.4421706382869,0.286255462618544,4.32565405918856));
#56368=CARTESIAN_POINT('Ctrl Pts',(22.4615999502279,0.130682174689606,4.40492695636159));
#56369=CARTESIAN_POINT('Ctrl Pts',(22.4730766228251,0.0307047625933256,
4.41585030288671));
#56370=CARTESIAN_POINT('Ctrl Pts',(22.4766006560785,3.63249072248342E-6,
4.41584094994071));
#56371=CARTESIAN_POINT('Ctrl Pts',(22.2733993439214,-5.11585294797612E-6,
4.41590580604266));
#56372=CARTESIAN_POINT('Ctrl Pts',(22.2739748303838,-0.0050164638240448,
4.41590888908576));
#56373=CARTESIAN_POINT('Ctrl Pts',(22.2825029561901,-0.0792779396689182,
4.41459464077989));
#56374=CARTESIAN_POINT('Ctrl Pts',(22.2989837213402,-0.221370022215225,
4.37281103827166));
#56375=CARTESIAN_POINT('Ctrl Pts',(22.3228416393716,-0.372934645290675,
4.22116172228637));
#56376=CARTESIAN_POINT('Ctrl Pts',(22.346699557403,-0.43330658847365,4.01543234121164));
#56377=CARTESIAN_POINT('Ctrl Pts',(22.3705574754345,-0.387723268841402,
3.80592933171158));
#56378=CARTESIAN_POINT('Ctrl Pts',(22.3944153934659,-0.247331046528593,
3.64388188817752));
#56379=CARTESIAN_POINT('Ctrl Pts',(22.4182733114973,-0.0464596501027702,
3.56891502119853));
#56380=CARTESIAN_POINT('Ctrl Pts',(22.4421312295287,0.165772403721094,3.59936017830047));
#56381=CARTESIAN_POINT('Ctrl Pts',(22.4659891475602,0.337468575289321,3.7277726770023));
#56382=CARTESIAN_POINT('Ctrl Pts',(22.4898470655915,0.426644514167594,3.92275218663495));
#56383=CARTESIAN_POINT('Ctrl Pts',(22.513704983623,0.411494197867752,4.13662086224655));
#56384=CARTESIAN_POINT('Ctrl Pts',(22.5375629016544,0.295722435535401,4.31708206952049));
#56385=CARTESIAN_POINT('Ctrl Pts',(22.5574610217539,0.138855410360913,4.40292493148274));
#56386=CARTESIAN_POINT('Ctrl Pts',(22.5694065025095,0.0347856757474044,
4.41583870262252));
#56387=CARTESIAN_POINT('Ctrl Pts',(22.5733993439214,-1.0582204931428E-7,
4.41583910483016));
#56388=CARTESIAN_POINT('Origin',(3.42660065607856,0.,4.));
#56389=CARTESIAN_POINT('',(21.8766006560786,1.03078286340212E-5,4.41586151989188));
#56390=CARTESIAN_POINT('',(21.9733993439214,8.40473402259622E-6,4.41585103914036));
#56391=CARTESIAN_POINT('',(3.42660065607856,4.87367679877478E-13,4.415875));
#56392=CARTESIAN_POINT('Ctrl Pts',(21.8766006560786,1.03078286340201E-5,
4.41586151989188));
#56393=CARTESIAN_POINT('Ctrl Pts',(21.8822132785738,-0.0488795353146484,
4.415816298089));
#56394=CARTESIAN_POINT('Ctrl Pts',(21.8957785404128,-0.167079919178725,
4.39498170153279));
#56395=CARTESIAN_POINT('Ctrl Pts',(21.9172964415957,-0.326407159500644,
4.28539643168872));
#56396=CARTESIAN_POINT('Ctrl Pts',(21.9411543596271,-0.423245389017799,
4.09410684177624));
#56397=CARTESIAN_POINT('Ctrl Pts',(21.9650122776585,-0.416588591947193,
3.87980556563057));
#56398=CARTESIAN_POINT('Ctrl Pts',(21.98887019569,-0.30806453650007,3.69489510271888));
#56399=CARTESIAN_POINT('Ctrl Pts',(22.0127281137213,-0.12421031036921,3.58459109808296));
#56400=CARTESIAN_POINT('Ctrl Pts',(22.0365860317528,0.0900167200678817,
3.57586588547707));
#56401=CARTESIAN_POINT('Ctrl Pts',(22.0604439497842,0.282232210442068,3.67085301705332));
#56402=CARTESIAN_POINT('Ctrl Pts',(22.0843018678157,0.405434237512275,3.8463255517439));
#56403=CARTESIAN_POINT('Ctrl Pts',(22.108159785847,0.429496549703537,4.05937567504088));
#56404=CARTESIAN_POINT('Ctrl Pts',(22.1320177038785,0.348535256241736,4.25790682842971));
#56405=CARTESIAN_POINT('Ctrl Pts',(22.1548313272889,0.18962186617866,4.38744320371645));
#56406=CARTESIAN_POINT('Ctrl Pts',(22.1696923113557,0.0601536901409818,
4.41584170838249));
#56407=CARTESIAN_POINT('Ctrl Pts',(22.1766006560786,-8.37799962077716E-6,
4.41589611849309));
#56408=CARTESIAN_POINT('Ctrl Pts',(21.9733993439214,8.40473402260317E-6,
4.41585103914036));
#56409=CARTESIAN_POINT('Ctrl Pts',(21.9785431582582,-0.044801031555974,
4.41581845947763));
#56410=CARTESIAN_POINT('Ctrl Pts',(21.9916396119388,-0.158914563981884,
4.39744691543598));
#56411=CARTESIAN_POINT('Ctrl Pts',(22.0126887049632,-0.317860118355158,
4.29488591379237));
#56412=CARTESIAN_POINT('Ctrl Pts',(22.0365466229946,-0.420290167226249,
4.10653136780738));
#56413=CARTESIAN_POINT('Ctrl Pts',(22.060404541026,-0.419947821735935,3.89212700053744));
#56414=CARTESIAN_POINT('Ctrl Pts',(22.0842624590574,-0.316916794682727,
3.70410052003731));
#56415=CARTESIAN_POINT('Ctrl Pts',(22.1081203770888,-0.136390978688423,
3.58842952252864));
#56416=CARTESIAN_POINT('Ctrl Pts',(22.1319782951203,0.0774861468089536,
3.57339871771534));
#56417=CARTESIAN_POINT('Ctrl Pts',(22.1558362131517,0.27241579873489,3.66268354680831));
#56418=CARTESIAN_POINT('Ctrl Pts',(22.1796941311831,0.400732367405962,3.83445143701846));
#56419=CARTESIAN_POINT('Ctrl Pts',(22.2035520492145,0.431058956528623,4.04670046033727));
#56420=CARTESIAN_POINT('Ctrl Pts',(22.227409967246,0.355979888945518,4.24752994899471));
#56421=CARTESIAN_POINT('Ctrl Pts',(22.2506923988149,0.197764744804664,4.38444734931837));
#56422=CARTESIAN_POINT('Ctrl Pts',(22.26602219104,0.064235283418036,4.41586628455644));
#56423=CARTESIAN_POINT('Ctrl Pts',(22.2733993439214,-5.11585294797612E-6,
4.41590580604266));
#56424=CARTESIAN_POINT('Origin',(3.42660065607856,0.,4.));
#56425=CARTESIAN_POINT('',(21.5766006560785,-1.05752387382048E-5,4.41586434469346));
#56426=CARTESIAN_POINT('',(21.6733993439214,-1.08222664516599E-5,4.41587700699864));
#56427=CARTESIAN_POINT('',(3.42660065607856,4.87367679877478E-13,4.415875));
#56428=CARTESIAN_POINT('Ctrl Pts',(21.5766006560785,-1.05752387381843E-5,
4.41586434469346));
#56429=CARTESIAN_POINT('Ctrl Pts',(21.5788289671043,-0.0194203346498642,
4.41588296395747));
#56430=CARTESIAN_POINT('Ctrl Pts',(21.5890099174739,-0.10809016089515,4.40978779866957));
#56431=CARTESIAN_POINT('Ctrl Pts',(21.6071435071872,-0.258824259222961,
4.34785450957493));
#56432=CARTESIAN_POINT('Ctrl Pts',(21.6310014252187,-0.39385182381868,4.18131050126406));
#56433=CARTESIAN_POINT('Ctrl Pts',(21.6548593432501,-0.432571889182456,
3.97043113659525));
#56434=CARTESIAN_POINT('Ctrl Pts',(21.6787172612815,-0.365516344619441,
3.76678216446856));
#56435=CARTESIAN_POINT('Ctrl Pts',(21.702575179313,-0.209082097331647,3.62016130585559));
#56436=CARTESIAN_POINT('Ctrl Pts',(21.7264330973443,-0.00152158196427748,
3.56642135455923));
#56437=CARTESIAN_POINT('Ctrl Pts',(21.7502910153758,0.206411001640417,3.61870319251831));
#56438=CARTESIAN_POINT('Ctrl Pts',(21.7741489334072,0.363870472821225,3.76422248622317));
#56439=CARTESIAN_POINT('Ctrl Pts',(21.7980068514386,0.432353701764573,3.96739580449697));
#56440=CARTESIAN_POINT('Ctrl Pts',(21.82186476947,0.395114673548107,4.17854173669174));
#56441=CARTESIAN_POINT('Ctrl Pts',(21.8457226875014,0.261259344941517,4.3460293508861));
#56442=CARTESIAN_POINT('Ctrl Pts',(21.8639679830376,0.110037800305057,4.4094070875278));
#56443=CARTESIAN_POINT('Ctrl Pts',(21.87426063923,0.0203934810735595,4.41588037378429));
#56444=CARTESIAN_POINT('Ctrl Pts',(21.8766006560786,1.03078286340201E-5,
4.41586151989188));
#56445=CARTESIAN_POINT('Ctrl Pts',(21.6733993439214,-1.0822266451653E-5,
4.41587700699864));
#56446=CARTESIAN_POINT('Ctrl Pts',(21.6751588467887,-0.0153356749568721,
4.41589290068126));
#56447=CARTESIAN_POINT('Ctrl Pts',(21.6848709889998,-0.0999166717736498,
4.41130778913604));
#56448=CARTESIAN_POINT('Ctrl Pts',(21.7025357705547,-0.248467031045983,
4.35532645760922));
#56449=CARTESIAN_POINT('Ctrl Pts',(21.7263936885861,-0.388341045935521,
4.1928315042612));
#56450=CARTESIAN_POINT('Ctrl Pts',(21.7502516066176,-0.433255096896122,
3.98318399549658));
#56451=CARTESIAN_POINT('Ctrl Pts',(21.774109524649,-0.372226475033738,3.77764845789182));
#56452=CARTESIAN_POINT('Ctrl Pts',(21.7979674426804,-0.220178340780001,
3.62648392906691));
#56453=CARTESIAN_POINT('Ctrl Pts',(21.8218253607118,-0.0142906046679706,
3.56665425395863));
#56454=CARTESIAN_POINT('Ctrl Pts',(21.8456832787432,0.195091573553633,3.61278941785858));
#56455=CARTESIAN_POINT('Ctrl Pts',(21.8695411967747,0.356768547853618,3.75360811649661));
#56456=CARTESIAN_POINT('Ctrl Pts',(21.8933991148061,0.431205894023261,3.95467634223136));
#56457=CARTESIAN_POINT('Ctrl Pts',(21.9172570328375,0.400201653291494,4.16682743688221));
#56458=CARTESIAN_POINT('Ctrl Pts',(21.941114950869,0.271337207055788,4.33818467892719));
#56459=CARTESIAN_POINT('Ctrl Pts',(21.9598290545635,0.118211900824938,4.40773087908456));
#56460=CARTESIAN_POINT('Ctrl Pts',(21.9705905189143,0.0244769910710258,
4.41586882955141));
#56461=CARTESIAN_POINT('Ctrl Pts',(21.9733993439214,8.40473402260317E-6,
4.41585103914036));
#56462=CARTESIAN_POINT('Origin',(3.42660065607856,0.,4.));
#56463=CARTESIAN_POINT('',(21.2766006560785,8.9771325895615E-6,4.41589335210553));
#56464=CARTESIAN_POINT('',(21.3733993439214,1.06214664634743E-5,4.41588075133303));
#56465=CARTESIAN_POINT('',(3.42660065607856,4.87367679877478E-13,4.415875));
#56466=CARTESIAN_POINT('Ctrl Pts',(21.2766006560785,8.97713258955941E-6,
4.41589335210553));
#56467=CARTESIAN_POINT('Ctrl Pts',(21.2833972949786,-0.0591814269577189,
4.41583723296416));
#56468=CARTESIAN_POINT('Ctrl Pts',(21.2981465732225,-0.187680420990878,
4.38813575385326));
#56469=CARTESIAN_POINT('Ctrl Pts',(21.3208484908102,-0.346716519889314,
4.26034671465164));
#56470=CARTESIAN_POINT('Ctrl Pts',(21.3447064088417,-0.429069235164158,
4.0623886883135));
#56471=CARTESIAN_POINT('Ctrl Pts',(21.368564326873,-0.406502834830527,3.8491749282489));
#56472=CARTESIAN_POINT('Ctrl Pts',(21.3924222449045,-0.284535418465691,
3.67284200661995));
#56473=CARTESIAN_POINT('Ctrl Pts',(21.4162801629359,-0.0929913416969399,
3.5765081259772));
#56474=CARTESIAN_POINT('Ctrl Pts',(21.4401380809674,0.121291651150069,3.58372954422009));
#56475=CARTESIAN_POINT('Ctrl Pts',(21.4639959989987,0.305915531372611,3.69274042788069));
#56476=CARTESIAN_POINT('Ctrl Pts',(21.4878539170302,0.415734731202803,3.87688464650718));
#56477=CARTESIAN_POINT('Ctrl Pts',(21.5117118350615,0.423895464867194,4.09113392265755));
#56478=CARTESIAN_POINT('Ctrl Pts',(21.535569753093,0.328402210690932,4.28309847227994));
#56479=CARTESIAN_POINT('Ctrl Pts',(21.5571993600986,0.169024930905334,4.39437398220882));
#56480=CARTESIAN_POINT('Ctrl Pts',(21.5708763277605,0.0498513310028489,
4.41581651349798));
#56481=CARTESIAN_POINT('Ctrl Pts',(21.5766006560785,-1.05752387381843E-5,
4.41586434469346));
#56482=CARTESIAN_POINT('Ctrl Pts',(21.3733993439214,1.06214664634605E-5,
4.41588075133303));
#56483=CARTESIAN_POINT('Ctrl Pts',(21.379727174663,-0.0551018547626871,
4.41582358345633));
#56484=CARTESIAN_POINT('Ctrl Pts',(21.3940076447484,-0.1795281855266,4.39095386216025));
#56485=CARTESIAN_POINT('Ctrl Pts',(21.4162407541777,-0.338898428465248,
4.27044521104599));
#56486=CARTESIAN_POINT('Ctrl Pts',(21.4400986722091,-0.427045644525908,
4.07499849655415));
#56487=CARTESIAN_POINT('Ctrl Pts',(21.4639565902406,-0.410768568010174,
3.86121260673678));
#56488=CARTESIAN_POINT('Ctrl Pts',(21.4878145082719,-0.294047387504818,
3.68136401506497));
#56489=CARTESIAN_POINT('Ctrl Pts',(21.5116724263034,-0.105423611064507,
3.57943060117972));
#56490=CARTESIAN_POINT('Ctrl Pts',(21.5355303443348,0.108979109962582,3.58033786138646));
#56491=CARTESIAN_POINT('Ctrl Pts',(21.5593882623662,0.296733470072461,3.68386394585134));
#56492=CARTESIAN_POINT('Ctrl Pts',(21.5832461803976,0.411928413892185,3.86469390692879));
#56493=CARTESIAN_POINT('Ctrl Pts',(21.6071040984291,0.426395639810567,4.07860989342611));
#56494=CARTESIAN_POINT('Ctrl Pts',(21.6309620164605,0.33659751701124,4.27330361969026));
#56495=CARTESIAN_POINT('Ctrl Pts',(21.6530604316246,0.177184770587036,4.39173732935402));
#56496=CARTESIAN_POINT('Ctrl Pts',(21.6672062074449,0.0539299276789421,
4.41582106406873));
#56497=CARTESIAN_POINT('Ctrl Pts',(21.6733993439214,-1.0822266451653E-5,
4.41587700699864));
#56498=CARTESIAN_POINT('Origin',(3.42660065607856,0.,4.));
#56499=CARTESIAN_POINT('',(20.9766006560786,-4.48287659654576E-6,4.41584197426197));
#56500=CARTESIAN_POINT('',(21.0733993439214,-7.65157297119567E-6,4.41584853425778));
#56501=CARTESIAN_POINT('',(3.42660065607856,4.87367679877478E-13,4.415875));
#56502=CARTESIAN_POINT('Ctrl Pts',(20.9766006560786,-4.48287659652116E-6,
4.41584197426197));
#56503=CARTESIAN_POINT('Ctrl Pts',(20.9800129835092,-0.0297322302090305,
4.41585318364051));
#56504=CARTESIAN_POINT('Ctrl Pts',(20.9913779502836,-0.128734546054536,
4.40538471300776));
#56505=CARTESIAN_POINT('Ctrl Pts',(21.0106955564018,-0.28396276796243,4.32765515869354));
#56506=CARTESIAN_POINT('Ctrl Pts',(21.0345534744332,-0.40623841344949,4.15153583326342));
#56507=CARTESIAN_POINT('Ctrl Pts',(21.0584113924646,-0.429177699343215,
3.93836186909709));
#56508=CARTESIAN_POINT('Ctrl Pts',(21.082269310496,-0.347171348131155,3.74026010679315));
#56509=CARTESIAN_POINT('Ctrl Pts',(21.1061272285274,-0.180272145040548,
3.605671823621));
#56510=CARTESIAN_POINT('Ctrl Pts',(21.1299851465589,0.0307085077608185,
3.56750752082027));
#56511=CARTESIAN_POINT('Ctrl Pts',(21.1538430645903,0.234180094072738,3.63509941005724));
#56512=CARTESIAN_POINT('Ctrl Pts',(21.1777009826217,0.380388268371489,3.79191943321731));
#56513=CARTESIAN_POINT('Ctrl Pts',(21.2015589006531,0.433581149524578,3.99962082296209));
#56514=CARTESIAN_POINT('Ctrl Pts',(21.2254168186846,0.380751629084578,4.2074149318183));
#56515=CARTESIAN_POINT('Ctrl Pts',(21.2492747367159,0.234817963878357,4.36449043997717));
#56516=CARTESIAN_POINT('Ctrl Pts',(21.2663360158473,0.0893960873046664,
4.41308118928586));
#56517=CARTESIAN_POINT('Ctrl Pts',(21.2754446556348,0.0100763257733538,
4.41590289708112));
#56518=CARTESIAN_POINT('Ctrl Pts',(21.2766006560785,8.97713258955941E-6,
4.41589335210553));
#56519=CARTESIAN_POINT('Ctrl Pts',(21.0733993439214,-7.65157297121996E-6,
4.41584853425778));
#56520=CARTESIAN_POINT('Ctrl Pts',(21.0763428631935,-0.0256500457845501,
4.41586537097631));
#56521=CARTESIAN_POINT('Ctrl Pts',(21.0872390218095,-0.120560449820324,
4.40722571769055));
#56522=CARTESIAN_POINT('Ctrl Pts',(21.1060878197692,-0.274189543318984,
4.33587624407661));
#56523=CARTESIAN_POINT('Ctrl Pts',(21.1299457378007,-0.401599180171465,
4.16343456021562));
#56524=CARTESIAN_POINT('Ctrl Pts',(21.1538036558321,-0.430806878168669,
3.95102867450389));
#56525=CARTESIAN_POINT('Ctrl Pts',(21.1776615738635,-0.354670559489406,
3.75059761183336));
#56526=CARTESIAN_POINT('Ctrl Pts',(21.2015194918949,-0.191807627993766,
3.61115222665144));
#56527=CARTESIAN_POINT('Ctrl Pts',(21.2253774099264,0.0179574932869785,
3.56679071405539));
#56528=CARTESIAN_POINT('Ctrl Pts',(21.2492353279577,0.223331518303719,3.62836067225603));
#56529=CARTESIAN_POINT('Ctrl Pts',(21.2730932459892,0.374094903668402,3.78080656934254));
#56530=CARTESIAN_POINT('Ctrl Pts',(21.2969511640206,0.433381894944723,3.98685123093373));
#56531=CARTESIAN_POINT('Ctrl Pts',(21.320809082052,0.386695207821707,4.19611112472705));
#56532=CARTESIAN_POINT('Ctrl Pts',(21.3446670000834,0.245451009020076,4.35741650656472));
#56533=CARTESIAN_POINT('Ctrl Pts',(21.3621970873732,0.0975684711839555,
4.41172139589413));
#56534=CARTESIAN_POINT('Ctrl Pts',(21.3717745353192,0.014161952170494,4.41589543043265));
#56535=CARTESIAN_POINT('Ctrl Pts',(21.3733993439214,1.06214664634605E-5,
4.41588075133303));
#56536=CARTESIAN_POINT('Origin',(3.42660065607856,0.,4.));
#56537=CARTESIAN_POINT('',(20.6766006560786,1.29204965968245E-6,4.41591114679826));
#56538=CARTESIAN_POINT('',(20.7733993439214,3.9567662055099E-6,4.41590779860895));
#56539=CARTESIAN_POINT('',(3.42660065607856,4.87367679877478E-13,4.415875));
#56540=CARTESIAN_POINT('Ctrl Pts',(20.6766006560786,1.29076178055295E-6,
4.41591111076812));
#56541=CARTESIAN_POINT('Ctrl Pts',(20.6766286720397,-0.000242659277546582,
4.41591112051333));
#56542=CARTESIAN_POINT('Ctrl Pts',(20.6846093273446,-0.0697345275278937,
4.41585145172406));
#56543=CARTESIAN_POINT('Ctrl Pts',(20.7005426219933,-0.208420567790133,
4.38020336888205));
#56544=CARTESIAN_POINT('Ctrl Pts',(20.7244005400248,-0.365106210756856,
4.23385701605743));
#56545=CARTESIAN_POINT('Ctrl Pts',(20.7482584580562,-0.432520392530856,
4.03032528343114));
#56546=CARTESIAN_POINT('Ctrl Pts',(20.7721163760876,-0.394167874571092,
3.81937870627435));
#56547=CARTESIAN_POINT('Ctrl Pts',(20.795974294119,-0.259432524437891,3.65259868360638));
#56548=CARTESIAN_POINT('Ctrl Pts',(20.8198322121504,-0.0612578225112809,
3.57076788979259));
#56549=CARTESIAN_POINT('Ctrl Pts',(20.8436901301819,0.151895538690754,3.5938959627232));
#56550=CARTESIAN_POINT('Ctrl Pts',(20.8675480482132,0.327906592802717,3.71632757520176));
#56551=CARTESIAN_POINT('Ctrl Pts',(20.8914059662447,0.423735399567132,3.90812480123879));
#56552=CARTESIAN_POINT('Ctrl Pts',(20.9152638842761,0.415949440063929,4.12238802732943));
#56553=CARTESIAN_POINT('Ctrl Pts',(20.9391218023075,0.30645246920106,4.30672404095661));
#56554=CARTESIAN_POINT('Ctrl Pts',(20.9595673929083,0.148398440326279,4.40042000858165));
#56555=CARTESIAN_POINT('Ctrl Pts',(20.9720603441653,0.0395501167658222,
4.4158270594931));
#56556=CARTESIAN_POINT('Ctrl Pts',(20.9766006560786,-4.48287659652116E-6,
4.41584197426197));
#56557=CARTESIAN_POINT('Ctrl Pts',(20.7733993439214,3.95676620551077E-6,
4.41590779860895));
#56558=CARTESIAN_POINT('Ctrl Pts',(20.7809111910678,-0.0654084660523611,
4.41587519962517));
#56559=CARTESIAN_POINT('Ctrl Pts',(20.7963756775582,-0.200102595337945,
4.3835597345012));
#56560=CARTESIAN_POINT('Ctrl Pts',(20.8197928033922,-0.358062019934396,
4.24450842127602));
#56561=CARTESIAN_POINT('Ctrl Pts',(20.8436507214237,-0.431438726014498,
4.04305074550709));
#56562=CARTESIAN_POINT('Ctrl Pts',(20.867508639455,-0.399316990859146,3.83106596928302));
#56563=CARTESIAN_POINT('Ctrl Pts',(20.8913665574865,-0.269551332195825,
3.66039017609669));
#56564=CARTESIAN_POINT('Ctrl Pts',(20.9152244755179,-0.0738730526583281,
3.57275822989076));
#56565=CARTESIAN_POINT('Ctrl Pts',(20.9390823935493,0.139869212314499,3.58959853735383));
#56566=CARTESIAN_POINT('Ctrl Pts',(20.9629403115807,0.319409638666883,3.70679317993256));
#56567=CARTESIAN_POINT('Ctrl Pts',(20.9867982296122,0.420845711130686,3.8956848776653));
#56568=CARTESIAN_POINT('Ctrl Pts',(21.0106561476436,0.419373541863394,4.11008446384341));
#56569=CARTESIAN_POINT('Ctrl Pts',(21.034514065675,0.315353119032788,4.29756540021079));
#56570=CARTESIAN_POINT('Ctrl Pts',(21.0554284644342,0.156567902793621,4.39812991232556));
#56571=CARTESIAN_POINT('Ctrl Pts',(21.0683902238497,0.0436291721249729,
4.41581988245125));
#56572=CARTESIAN_POINT('Ctrl Pts',(21.0733993439214,-7.65157297121996E-6,
4.41584853425778));
#56573=CARTESIAN_POINT('Origin',(3.42660065607856,0.,4.));
#56574=CARTESIAN_POINT('',(20.3766006560786,0.000383027521040961,4.41597069455794));
#56575=CARTESIAN_POINT('',(20.4733993439214,0.000101608071013781,4.41586489633469));
#56576=CARTESIAN_POINT('',(3.42660065607856,4.87367679877478E-13,4.415875));
#56577=CARTESIAN_POINT('Ctrl Pts',(20.3766006560786,0.000383027521040954,
4.41597069455794));
#56578=CARTESIAN_POINT('Ctrl Pts',(20.3891496392578,-0.108893832387875,
4.41487837761012));
#56579=CARTESIAN_POINT('Ctrl Pts',(20.4176039011246,-0.35839559572325,4.31454223548297));
#56580=CARTESIAN_POINT('Ctrl Pts',(20.4540108023354,-0.457800032585507,
3.97025345815189));
#56581=CARTESIAN_POINT('Ctrl Pts',(20.4858213597105,-0.325993724402262,
3.71529210935379));
#56582=CARTESIAN_POINT('Ctrl Pts',(20.509679277742,-0.15096738523986,3.59329490328468));
#56583=CARTESIAN_POINT('Ctrl Pts',(20.5335371957734,0.0630371972956549,
3.57102347342756));
#56584=CARTESIAN_POINT('Ctrl Pts',(20.5573951138048,0.260511246441404,3.65349437971329));
#56585=CARTESIAN_POINT('Ctrl Pts',(20.5812530318362,0.394877283734959,3.82077798440408));
#56586=CARTESIAN_POINT('Ctrl Pts',(20.6051109498677,0.432370081305563,4.03184236506754));
#56587=CARTESIAN_POINT('Ctrl Pts',(20.6289688678991,0.364303478986858,4.23514367899931));
#56588=CARTESIAN_POINT('Ctrl Pts',(20.6527987699694,0.207251017164088,4.38076243960928));
#56589=CARTESIAN_POINT('Ctrl Pts',(20.6686760326959,0.0690052481014253,
4.41590835422812));
#56590=CARTESIAN_POINT('Ctrl Pts',(20.6766006560786,1.29076178055295E-6,
4.41591111076812));
#56591=CARTESIAN_POINT('Ctrl Pts',(20.4733993439214,0.000101608071013788,
4.4158648963347));
#56592=CARTESIAN_POINT('Ctrl Pts',(20.4775268795984,-0.0359150725839473,
4.41584626969953));
#56593=CARTESIAN_POINT('Ctrl Pts',(20.4896070546192,-0.141401612166324,
4.40227446254147));
#56594=CARTESIAN_POINT('Ctrl Pts',(20.5096398689838,-0.298255971346869,
4.31460392554555));
#56595=CARTESIAN_POINT('Ctrl Pts',(20.5334977870152,-0.412709509332759,
4.13311446574462));
#56596=CARTESIAN_POINT('Ctrl Pts',(20.5573557050466,-0.425936384696969,
3.91915434697803));
#56597=CARTESIAN_POINT('Ctrl Pts',(20.581213623078,-0.335173342752607,3.72492109335083));
#56598=CARTESIAN_POINT('Ctrl Pts',(20.6050715411095,-0.162364888615448,
3.59797442377207));
#56599=CARTESIAN_POINT('Ctrl Pts',(20.6289294591408,0.0501004451364318,
3.56932214892951));
#56600=CARTESIAN_POINT('Ctrl Pts',(20.6527873771723,0.250339089241223,3.64598859455508));
#56601=CARTESIAN_POINT('Ctrl Pts',(20.6766452952037,0.389350172549011,3.80921715950176));
#56602=CARTESIAN_POINT('Ctrl Pts',(20.7005032132352,0.433161330121289,4.01909908002448));
#56603=CARTESIAN_POINT('Ctrl Pts',(20.7243611312665,0.371049143609512,4.22430982617278));
#56604=CARTESIAN_POINT('Ctrl Pts',(20.748219049298,0.218207240773441,4.37467120177868));
#56605=CARTESIAN_POINT('Ctrl Pts',(20.7645651201829,0.0769305199015265,
4.41491906931248));
#56606=CARTESIAN_POINT('Ctrl Pts',(20.772958551724,0.00384233167249433,
4.41590971150433));
#56607=CARTESIAN_POINT('Ctrl Pts',(20.7733993439214,3.95676620551077E-6,
4.41590779860895));
#56608=CARTESIAN_POINT('Origin',(3.42660065607856,0.,4.));
#56609=CARTESIAN_POINT('',(20.0766006560786,-0.000186622634748148,4.41645953600834));
#56610=CARTESIAN_POINT('',(20.1733993439214,-0.000111611226006447,4.41653056081536));
#56611=CARTESIAN_POINT('',(3.42660065607856,4.87367679877478E-13,4.415875));
#56612=CARTESIAN_POINT('Ctrl Pts',(20.0766006560786,-0.000186622634748109,
4.41645953600834));
#56613=CARTESIAN_POINT('Ctrl Pts',(20.0778126884445,-0.0107019642254321,
4.4165186149328));
#56614=CARTESIAN_POINT('Ctrl Pts',(20.0949299994981,-0.159149739060163,
4.41138240526969));
#56615=CARTESIAN_POINT('Ctrl Pts',(20.1279525892393,-0.432744382500041,
4.23375285658289));
#56616=CARTESIAN_POINT('Ctrl Pts',(20.1756684253021,-0.430649333670284,
3.76246031529274));
#56617=CARTESIAN_POINT('Ctrl Pts',(20.223384261365,-0.033136228617316,3.50924504180455));
#56618=CARTESIAN_POINT('Ctrl Pts',(20.2711000974278,0.394908089060633,3.70680919012016));
#56619=CARTESIAN_POINT('Ctrl Pts',(20.3188159334906,0.460110046434968,4.17340395051402));
#56620=CARTESIAN_POINT('Ctrl Pts',(20.3539827863742,0.197028357007358,4.40022211154544));
#56621=CARTESIAN_POINT('Ctrl Pts',(20.3732443605702,0.0296097328916507,
4.416262840815));
#56622=CARTESIAN_POINT('Ctrl Pts',(20.3766006560786,0.000383027521040954,
4.41597069455794));
#56623=CARTESIAN_POINT('Ctrl Pts',(20.1733993439214,-0.000111611226006447,
4.41653056081536));
#56624=CARTESIAN_POINT('Ctrl Pts',(20.1741425681289,-0.00655727229825777,
4.41655465488103));
#56625=CARTESIAN_POINT('Ctrl Pts',(20.190791071024,-0.150919726673813,4.41348743992374));
#56626=CARTESIAN_POINT('Ctrl Pts',(20.2233448526067,-0.425711472830213,
4.24633918020534));
#56627=CARTESIAN_POINT('Ctrl Pts',(20.2710606886696,-0.437384262562023,
3.77535541015343));
#56628=CARTESIAN_POINT('Ctrl Pts',(20.3187765247324,-0.0477164433392854,
3.51022640082505));
#56629=CARTESIAN_POINT('Ctrl Pts',(20.3664923607953,0.386374384143037,3.69571627142296));
#56630=CARTESIAN_POINT('Ctrl Pts',(20.4062555575143,0.45143962727185,4.08165775845481));
#56631=CARTESIAN_POINT('Ctrl Pts',(20.4380661148895,0.291471375703242,4.31996082336987));
#56632=CARTESIAN_POINT('Ctrl Pts',(20.4577964972439,0.136183087716603,4.40372206768731));
#56633=CARTESIAN_POINT('Ctrl Pts',(20.4695742402546,0.0334792813416625,
4.41588215816259));
#56634=CARTESIAN_POINT('Ctrl Pts',(20.4733993439214,0.000101608071013788,
4.4158648963347));
#56635=CARTESIAN_POINT('Origin',(3.42660065607856,0.,4.));
#56636=CARTESIAN_POINT('',(19.7766006560786,-0.000280998963924209,4.41539029291088));
#56637=CARTESIAN_POINT('',(19.8733993439214,-0.000322938566065189,4.41548189938477));
#56638=CARTESIAN_POINT('',(3.42660065607856,4.87367679877478E-13,4.415875));
#56639=CARTESIAN_POINT('Ctrl Pts',(19.7766006560786,-0.000280998963924181,
4.41539029291088));
#56640=CARTESIAN_POINT('Ctrl Pts',(19.7823810163188,-0.0507615353771658,
4.41570272077311));
#56641=CARTESIAN_POINT('Ctrl Pts',(19.8040666552467,-0.23976299482565,4.3837755623668));
#56642=CARTESIAN_POINT('Ctrl Pts',(19.8416575728622,-0.481212499922896,
4.10168523844358));
#56643=CARTESIAN_POINT('Ctrl Pts',(19.8893734089251,-0.345789702982467,
3.65023692191923));
#56644=CARTESIAN_POINT('Ctrl Pts',(19.9370892449879,0.107175910646637,3.51998011832295));
#56645=CARTESIAN_POINT('Ctrl Pts',(19.9848050810508,0.461722480014006,3.83053541934297));
#56646=CARTESIAN_POINT('Ctrl Pts',(20.0313088847476,0.394022427012164,4.28486673161383));
#56647=CARTESIAN_POINT('Ctrl Pts',(20.0619074097569,0.127288937001902,4.4157433330307));
#56648=CARTESIAN_POINT('Ctrl Pts',(20.0766006560786,-0.000186622634748109,
4.41645953600834));
#56649=CARTESIAN_POINT('Ctrl Pts',(19.8733993439214,-0.000322938566065196,
4.41548189938477));
#56650=CARTESIAN_POINT('Ctrl Pts',(19.8787108960032,-0.0466836533228258,
4.41581668875846));
#56651=CARTESIAN_POINT('Ctrl Pts',(19.8999277267727,-0.231469429366377,
4.38724295332581));
#56652=CARTESIAN_POINT('Ctrl Pts',(19.9370498362297,-0.47800980043334,4.11581244897344));
#56653=CARTESIAN_POINT('Ctrl Pts',(19.9847656722926,-0.355939225796451,
3.66057517601247));
#56654=CARTESIAN_POINT('Ctrl Pts',(20.0324815083554,0.0929888682922082,
3.51702731322357));
#56655=CARTESIAN_POINT('Ctrl Pts',(20.0801973444182,0.456536973876988,3.81701888067549));
#56656=CARTESIAN_POINT('Ctrl Pts',(20.1271699562736,0.401683300383188,4.27772103607547));
#56657=CARTESIAN_POINT('Ctrl Pts',(20.1582372894413,0.131382308576697,4.41603903277767));
#56658=CARTESIAN_POINT('Ctrl Pts',(20.1733993439214,-0.000111611226006447,
4.41653056081536));
#56659=CARTESIAN_POINT('Origin',(3.42660065607856,0.,4.));
#56660=CARTESIAN_POINT('',(19.4766006560786,0.000302289446139524,4.41543216566181));
#56661=CARTESIAN_POINT('',(19.5733993439214,0.000255464646300079,4.41534829948978));
#56662=CARTESIAN_POINT('',(3.42660065607856,4.87367679877478E-13,4.415875));
#56663=CARTESIAN_POINT('Ctrl Pts',(19.4766006560786,0.000302289446139546,
4.41543216566181));
#56664=CARTESIAN_POINT('Ctrl Pts',(19.4869493441932,-0.0900510892866153,
4.41482666801407));
#56665=CARTESIAN_POINT('Ctrl Pts',(19.5132033109954,-0.320168095705801,
4.3413809155508));
#56666=CARTESIAN_POINT('Ctrl Pts',(19.5553625564852,-0.490312813065352,
3.96128857502183));
#56667=CARTESIAN_POINT('Ctrl Pts',(19.603078392548,-0.232620797759261,3.56664935826393));
#56668=CARTESIAN_POINT('Ctrl Pts',(19.6507942286109,0.238690449241969,3.56996267500769));
#56669=CARTESIAN_POINT('Ctrl Pts',(19.6985100646737,0.490808633485035,3.96818593857384));
#56670=CARTESIAN_POINT('Ctrl Pts',(19.7404455404963,0.316268156276861,4.34384396940031));
#56671=CARTESIAN_POINT('Ctrl Pts',(19.7664757376312,0.0881410531427697,
4.41484304213512));
#56672=CARTESIAN_POINT('Ctrl Pts',(19.7766006560786,-0.000280998963924181,
4.41539029291088));
#56673=CARTESIAN_POINT('Ctrl Pts',(19.5733993439214,0.000255464646300094,
4.41534829948978));
#56674=CARTESIAN_POINT('Ctrl Pts',(19.5832792238775,-0.0860485087386658,
4.41486588036018));
#56675=CARTESIAN_POINT('Ctrl Pts',(19.6090643825213,-0.311990568344336,
4.34649332259355));
#56676=CARTESIAN_POINT('Ctrl Pts',(19.6507548198527,-0.491240257057309,
3.97574594767572));
#56677=CARTESIAN_POINT('Ctrl Pts',(19.6984706559155,-0.245282818621706,
3.57368850533185));
#56678=CARTESIAN_POINT('Ctrl Pts',(19.7461864919783,0.225921452997342,3.56311925573479));
#56679=CARTESIAN_POINT('Ctrl Pts',(19.7939023280412,0.489658867576397,3.95374471702426));
#56680=CARTESIAN_POINT('Ctrl Pts',(19.8363066120222,0.324430886710512,4.33863507066385));
#56681=CARTESIAN_POINT('Ctrl Pts',(19.8628056173156,0.0921420753912029,
4.4148141723173));
#56682=CARTESIAN_POINT('Ctrl Pts',(19.8733993439214,-0.000322938566065196,
4.41548189938477));
#56683=CARTESIAN_POINT('Origin',(3.42660065607856,0.,4.));
#56684=CARTESIAN_POINT('',(19.1766006560786,0.000155842099650094,4.41649089206047));
#56685=CARTESIAN_POINT('',(19.2733993439214,0.000220989830587742,4.4164164649367));
#56686=CARTESIAN_POINT('',(3.42660065607856,4.87367679877478E-13,4.415875));
#56687=CARTESIAN_POINT('Ctrl Pts',(19.1766006560786,0.000155842099650088,
4.41649089206047));
#56688=CARTESIAN_POINT('Ctrl Pts',(19.1915176720675,-0.129233580897558,
4.41587069825202));
#56689=CARTESIAN_POINT('Ctrl Pts',(19.2223399667441,-0.397695790553126,
4.28149179527637));
#56690=CARTESIAN_POINT('Ctrl Pts',(19.2690675401082,-0.459293044881286,
3.82405931712685));
#56691=CARTESIAN_POINT('Ctrl Pts',(19.316783376171,-0.100417177000157,3.51852142809106));
#56692=CARTESIAN_POINT('Ctrl Pts',(19.3644992122339,0.350673329058588,3.65513271950473));
#56693=CARTESIAN_POINT('Ctrl Pts',(19.4122150482967,0.479735122332443,4.10844094226069));
#56694=CARTESIAN_POINT('Ctrl Pts',(19.4495821962449,0.235804435834584,4.38544967282755));
#56695=CARTESIAN_POINT('Ctrl Pts',(19.4710440655056,0.0488163355692654,
4.4157572795781));
#56696=CARTESIAN_POINT('Ctrl Pts',(19.4766006560786,0.000302289446139546,
4.41543216566181));
#56697=CARTESIAN_POINT('Ctrl Pts',(19.2733993439214,0.000220989830587761,
4.4164164649367));
#56698=CARTESIAN_POINT('Ctrl Pts',(19.2878475517519,-0.125161313229646,
4.41561068768233));
#56699=CARTESIAN_POINT('Ctrl Pts',(19.31820103827,-0.389985711500173,4.28851341748863));
#56700=CARTESIAN_POINT('Ctrl Pts',(19.3644598034757,-0.464275578741542,
3.8376626582024));
#56701=CARTESIAN_POINT('Ctrl Pts',(19.4121756395385,-0.114554038379521,
3.52168776344319));
#56702=CARTESIAN_POINT('Ctrl Pts',(19.4598914756013,0.340364234683876,3.64495435060606));
#56703=CARTESIAN_POINT('Ctrl Pts',(19.5076073116642,0.482720800247919,4.09426482953845));
#56704=CARTESIAN_POINT('Ctrl Pts',(19.5454432677708,0.244097666198316,4.38190156491584));
#56705=CARTESIAN_POINT('Ctrl Pts',(19.5673739451899,0.0528892875329133,
4.41564251031262));
#56706=CARTESIAN_POINT('Ctrl Pts',(19.5733993439214,0.000255464646300094,
4.41534829948978));
#56707=CARTESIAN_POINT('Origin',(3.42660065607856,0.,4.));
#56708=CARTESIAN_POINT('',(18.8766006560785,-0.00038196507782994,4.41590683121974));
#56709=CARTESIAN_POINT('',(18.9733993439214,-0.000368287616214491,4.41603142687637));
#56710=CARTESIAN_POINT('',(3.42660065607856,4.87367679877478E-13,4.415875));
#56711=CARTESIAN_POINT('Ctrl Pts',(18.8766006560785,-0.000381965077829925,
4.41590683121974));
#56712=CARTESIAN_POINT('Ctrl Pts',(18.8801807212542,-0.0315488007868432,
4.41619587167324));
#56713=CARTESIAN_POINT('Ctrl Pts',(18.8996660651174,-0.200861076696893,
4.39874895857547));
#56714=CARTESIAN_POINT('Ctrl Pts',(18.9350566876684,-0.462607878309702,
4.16703046362027));
#56715=CARTESIAN_POINT('Ctrl Pts',(18.9827725237311,-0.39069124519864,3.70122654773242));
#56716=CARTESIAN_POINT('Ctrl Pts',(19.030488359794,0.0400031699426168,3.50979089028978));
#56717=CARTESIAN_POINT('Ctrl Pts',(19.0782041958568,0.433962058584907,3.76852180111673));
#56718=CARTESIAN_POINT('Ctrl Pts',(19.1259200319197,0.429406911488226,4.23982270375453));
#56719=CARTESIAN_POINT('Ctrl Pts',(19.1587188519936,0.155221332864305,4.41240136130926));
#56720=CARTESIAN_POINT('Ctrl Pts',(19.1756123933799,0.00872798149047904,
4.41653198033223));
#56721=CARTESIAN_POINT('Ctrl Pts',(19.1766006560786,0.000155842099650088,
4.41649089206047));
#56722=CARTESIAN_POINT('Ctrl Pts',(18.9733993439214,-0.000368287616214533,
4.41603142687637));
#56723=CARTESIAN_POINT('Ctrl Pts',(18.9765106009386,-0.0274330213022572,
4.4162811262788));
#56724=CARTESIAN_POINT('Ctrl Pts',(18.9955271366434,-0.192586232161443,
4.40152565608163));
#56725=CARTESIAN_POINT('Ctrl Pts',(19.0304489510358,-0.457487847288108,
4.18058265263639));
#56726=CARTESIAN_POINT('Ctrl Pts',(19.0781647870987,-0.399321187381313,
3.71286272589862));
#56727=CARTESIAN_POINT('Ctrl Pts',(19.1258806231614,0.0255482632835279,
3.50882537619781));
#56728=CARTESIAN_POINT('Ctrl Pts',(19.1735964592243,0.426956350589889,3.75584124112414));
#56729=CARTESIAN_POINT('Ctrl Pts',(19.2213122952871,0.436283851722622,4.22707185138688));
#56730=CARTESIAN_POINT('Ctrl Pts',(19.2545799235195,0.163455264474221,4.41023200720537));
#56731=CARTESIAN_POINT('Ctrl Pts',(19.2719422730642,0.0128655269200745,
4.41649772584937));
#56732=CARTESIAN_POINT('Ctrl Pts',(19.2733993439214,0.000220989830587761,
4.4164164649367));
#56733=CARTESIAN_POINT('Origin',(3.42660065607856,0.,4.));
#56734=CARTESIAN_POINT('',(18.5766006560786,2.82854505807383E-5,4.41518799822097));
#56735=CARTESIAN_POINT('',(18.6733993439214,-3.94222854199766E-5,4.41518963037823));
#56736=CARTESIAN_POINT('',(3.42660065607856,4.87367679877478E-13,4.415875));
#56737=CARTESIAN_POINT('Ctrl Pts',(18.5766006560786,2.82854505807215E-5,
4.41518799822097));
#56738=CARTESIAN_POINT('Ctrl Pts',(18.5847490491285,-0.0712192880865648,
4.41514491699706));
#56739=CARTESIAN_POINT('Ctrl Pts',(18.6088027208661,-0.281596950705947,
4.36382162423513));
#56740=CARTESIAN_POINT('Ctrl Pts',(18.6487616712913,-0.49096944006335,4.0292272779409));
#56741=CARTESIAN_POINT('Ctrl Pts',(18.6964775073541,-0.290120809601049,
3.60284116440841));
#56742=CARTESIAN_POINT('Ctrl Pts',(18.744193343417,0.177150224400508,3.54117212067402));
#56743=CARTESIAN_POINT('Ctrl Pts',(18.7919091794797,0.481741481528227,3.90085177849878));
#56744=CARTESIAN_POINT('Ctrl Pts',(18.836044950367,0.354281053487698,4.31776308733785));
#56745=CARTESIAN_POINT('Ctrl Pts',(18.8642754425666,0.106917172161326,4.4149117417093));
#56746=CARTESIAN_POINT('Ctrl Pts',(18.8766006560785,-0.000381965077829925,
4.41590683121974));
#56747=CARTESIAN_POINT('Ctrl Pts',(18.6733993439214,-3.94222854199489E-5,
4.41518963037823));
#56748=CARTESIAN_POINT('Ctrl Pts',(18.6810789288129,-0.0671871929144198,
4.41524623173262));
#56749=CARTESIAN_POINT('Ctrl Pts',(18.704663792392,-0.273330541024821,4.36810584919535));
#56750=CARTESIAN_POINT('Ctrl Pts',(18.7441539346588,-0.489895661254576,
4.0436745456279));
#56751=CARTESIAN_POINT('Ctrl Pts',(18.7918697707216,-0.301692008317894,
3.6115580391236));
#56752=CARTESIAN_POINT('Ctrl Pts',(18.8395856067845,0.163560057986223,3.53615376224111));
#56753=CARTESIAN_POINT('Ctrl Pts',(18.8873014428472,0.478612406344963,3.88670662268212));
#56754=CARTESIAN_POINT('Ctrl Pts',(18.9319060218929,0.362263203066427,4.31165738429376));
#56755=CARTESIAN_POINT('Ctrl Pts',(18.960605322251,0.110926532249199,4.41500462017153));
#56756=CARTESIAN_POINT('Ctrl Pts',(18.9733993439214,-0.000368287616214533,
4.41603142687637));
#56757=CARTESIAN_POINT('Origin',(3.42660065607856,0.,4.));
#56758=CARTESIAN_POINT('',(18.2766006560786,0.000371443240938316,4.41601098728712));
#56759=CARTESIAN_POINT('',(18.3733993439214,0.000382963303967143,4.41588626824893));
#56760=CARTESIAN_POINT('',(3.42660065607856,4.87367679877478E-13,4.415875));
#56761=CARTESIAN_POINT('Ctrl Pts',(18.2766006560785,0.000371443240938293,
4.41601098728712));
#56762=CARTESIAN_POINT('Ctrl Pts',(18.2893173770028,-0.110264925490287,
4.41498710445335));
#56763=CARTESIAN_POINT('Ctrl Pts',(18.3179393766147,-0.360950442388199,
4.31267773405576));
#56764=CARTESIAN_POINT('Ctrl Pts',(18.3624666549143,-0.479157019140895,
3.88903254594255));
#56765=CARTESIAN_POINT('Ctrl Pts',(18.4101824909771,-0.165810997523729,
3.5369536330429));
#56766=CARTESIAN_POINT('Ctrl Pts',(18.4578983270399,0.299801814449608,3.61009732380414));
#56767=CARTESIAN_POINT('Ctrl Pts',(18.5056141631028,0.49010200717001,4.04129464153984));
#56768=CARTESIAN_POINT('Ctrl Pts',(18.5451816061157,0.274694351318236,4.36741107590602));
#56769=CARTESIAN_POINT('Ctrl Pts',(18.5688437704409,0.0678526130816757,
4.41522900951301));
#56770=CARTESIAN_POINT('Ctrl Pts',(18.5766006560786,2.82854505807215E-5,
4.41518799822097));
#56771=CARTESIAN_POINT('Ctrl Pts',(18.3733993439214,0.000382963303967157,
4.41588626824893));
#56772=CARTESIAN_POINT('Ctrl Pts',(18.3856472566872,-0.106256708375174,
4.41489942083623));
#56773=CARTESIAN_POINT('Ctrl Pts',(18.4138004481407,-0.352960303644862,
4.31875095920395));
#56774=CARTESIAN_POINT('Ctrl Pts',(18.4578589182817,-0.482217355384067,
3.90319273261591));
#56775=CARTESIAN_POINT('Ctrl Pts',(18.5055747543446,-0.179376629827252,
3.54203793877243));
#56776=CARTESIAN_POINT('Ctrl Pts',(18.5532905904074,0.288188414964166,3.60143675240633));
#56777=CARTESIAN_POINT('Ctrl Pts',(18.6010064264702,0.491105603945206,4.02684232898929));
#56778=CARTESIAN_POINT('Ctrl Pts',(18.6410426776416,0.282958802096416,4.36309886994028));
#56779=CARTESIAN_POINT('Ctrl Pts',(18.6651736501253,0.0718833454275778,
4.41512900400112));
#56780=CARTESIAN_POINT('Ctrl Pts',(18.6733993439214,-3.94222854199489E-5,
4.41518963037823));
#56781=CARTESIAN_POINT('Origin',(3.42660065607856,0.,4.));
#56782=CARTESIAN_POINT('',(17.9766006560786,-0.000210814279110197,4.41643020456723));
#56783=CARTESIAN_POINT('',(18.0733993439214,-0.000144384975211464,4.41650095473263));
#56784=CARTESIAN_POINT('',(3.42660065607856,4.87367679877478E-13,4.415875));
#56785=CARTESIAN_POINT('Ctrl Pts',(17.9766006560786,-0.000210814279110157,
4.41643020456723));
#56786=CARTESIAN_POINT('Ctrl Pts',(17.9779804261896,-0.0121834889824064,
4.41650424974197));
#56787=CARTESIAN_POINT('Ctrl Pts',(17.9952654749882,-0.162096873242269,
4.41059855206721));
#56788=CARTESIAN_POINT('Ctrl Pts',(18.0284558024744,-0.435175833605105,
4.22918817311999));
#56789=CARTESIAN_POINT('Ctrl Pts',(18.0761716385373,-0.428137176707308,
3.75791781814212));
#56790=CARTESIAN_POINT('Ctrl Pts',(18.1238874746,-0.0279335627019553,3.5089552556775));
#56791=CARTESIAN_POINT('Ctrl Pts',(18.1716033106629,0.397921871745719,3.71092663761881));
#56792=CARTESIAN_POINT('Ctrl Pts',(18.2193191467257,0.458359528554279,4.17835853620019));
#56793=CARTESIAN_POINT('Ctrl Pts',(18.2543182618643,0.193950155243433,4.40107745006558));
#56794=CARTESIAN_POINT('Ctrl Pts',(18.2734120983152,0.0281121206155762,
4.41626771302466));
#56795=CARTESIAN_POINT('Ctrl Pts',(18.2766006560785,0.000371443240938293,
4.41601098728712));
#56796=CARTESIAN_POINT('Ctrl Pts',(18.0733993439214,-0.000144384975211439,
4.41650095473263));
#56797=CARTESIAN_POINT('Ctrl Pts',(18.0743103058739,-0.00804551399413891,
4.41653639380418));
#56798=CARTESIAN_POINT('Ctrl Pts',(18.0911265465141,-0.153864670001157,
4.41274680364665));
#56799=CARTESIAN_POINT('Ctrl Pts',(18.1238480658419,-0.428237044548737,
4.24190547436581));
#56800=CARTESIAN_POINT('Ctrl Pts',(18.1715639019047,-0.435081213444543,
3.7706322547532));
#56801=CARTESIAN_POINT('Ctrl Pts',(18.2192797379675,-0.0423836094492617,
3.50999096487715));
#56802=CARTESIAN_POINT('Ctrl Pts',(18.2669955740304,0.389235515258945,3.69933251171255));
#56803=CARTESIAN_POINT('Ctrl Pts',(18.3147114100932,0.463413677146622,4.16478163940629));
#56804=CARTESIAN_POINT('Ctrl Pts',(18.3501793333902,0.202226156869028,4.39827758107438));
#56805=CARTESIAN_POINT('Ctrl Pts',(18.3697419779996,0.0322267809866215,
4.41618095209965));
#56806=CARTESIAN_POINT('Ctrl Pts',(18.3733993439214,0.000382963303967157,
4.41588626824893));
#56807=CARTESIAN_POINT('Origin',(3.42660065607856,0.,4.));
#56808=CARTESIAN_POINT('',(17.6766006560786,-0.000263771022561219,4.41536107794487));
#56809=CARTESIAN_POINT('',(17.7733993439214,-0.000309142357869163,4.41544738986064));
#56810=CARTESIAN_POINT('',(3.42660065607856,4.87367679877478E-13,4.415875));
#56811=CARTESIAN_POINT('Ctrl Pts',(17.6766006560786,-0.000263771022561289,
4.41536107794487));
#56812=CARTESIAN_POINT('Ctrl Pts',(17.6825487540639,-0.0522183410383149,
4.41566152300153));
#56813=CARTESIAN_POINT('Ctrl Pts',(17.7044021307368,-0.24273028972288,4.38249735042552));
#56814=CARTESIAN_POINT('Ctrl Pts',(17.7421607860973,-0.48225726547346,4.09660825404716));
#56815=CARTESIAN_POINT('Ctrl Pts',(17.7898766221602,-0.342084653792828,
3.64661166616396));
#56816=CARTESIAN_POINT('Ctrl Pts',(17.837592458223,0.112229559114723,3.52113702282083));
#56817=CARTESIAN_POINT('Ctrl Pts',(17.8853082942859,0.463481641013499,3.83540961967535));
#56818=CARTESIAN_POINT('Ctrl Pts',(17.9316443602377,0.391261919872151,4.28736986940801));
#56819=CARTESIAN_POINT('Ctrl Pts',(17.962075147502,0.125831334120538,4.41565069513148));
#56820=CARTESIAN_POINT('Ctrl Pts',(17.9766006560786,-0.000210814279110157,
4.41643020456723));
#56821=CARTESIAN_POINT('Ctrl Pts',(17.7733993439214,-0.000309142357869142,
4.41544738986064));
#56822=CARTESIAN_POINT('Ctrl Pts',(17.7788786337482,-0.0481438769258273,
4.41577602216682));
#56823=CARTESIAN_POINT('Ctrl Pts',(17.8002632022627,-0.23443694547481,4.38601982759396));
#56824=CARTESIAN_POINT('Ctrl Pts',(17.8375530494648,-0.479202773223469,
4.11076970247734));
#56825=CARTESIAN_POINT('Ctrl Pts',(17.8852688855277,-0.352344189444135,
3.65683998336499));
#56826=CARTESIAN_POINT('Ctrl Pts',(17.9329847215905,0.0980774850139738,
3.51803938772416));
#56827=CARTESIAN_POINT('Ctrl Pts',(17.9807005576534,0.458433095867658,3.82183063825345));
#56828=CARTESIAN_POINT('Ctrl Pts',(18.0275054317636,0.3989600628602,4.28031410431705));
#56829=CARTESIAN_POINT('Ctrl Pts',(18.0584050271863,0.129907183855675,4.41591763216682));
#56830=CARTESIAN_POINT('Ctrl Pts',(18.0733993439214,-0.000144384975211439,
4.41650095473263));
#56831=CARTESIAN_POINT('Origin',(3.42660065607856,0.,4.));
#56832=CARTESIAN_POINT('',(17.3766006560786,0.000316824918469052,4.41546566829253));
#56833=CARTESIAN_POINT('',(17.4733993439214,0.000273208168652644,4.41537657040552));
#56834=CARTESIAN_POINT('',(3.42660065607856,4.87367679877478E-13,4.415875));
#56835=CARTESIAN_POINT('Ctrl Pts',(17.3766006560786,0.000316824918469058,
4.41546566829253));
#56836=CARTESIAN_POINT('Ctrl Pts',(17.3871170819382,-0.0914824399419538,
4.4148173972429));
#56837=CARTESIAN_POINT('Ctrl Pts',(17.4135387864855,-0.323087181591141,
4.33950699049548));
#56838=CARTESIAN_POINT('Ctrl Pts',(17.4558657697204,-0.489877595596684,
3.956123284257));
#56839=CARTESIAN_POINT('Ctrl Pts',(17.5035816057832,-0.228040769637767,
3.56422180844494));
#56840=CARTESIAN_POINT('Ctrl Pts',(17.551297441846,0.243209403937772,3.57250215124727));
#56841=CARTESIAN_POINT('Ctrl Pts',(17.5990132779089,0.491116639619549,3.97336034645914));
#56842=CARTESIAN_POINT('Ctrl Pts',(17.6407810159864,0.313340775136121,4.34566293955037));
#56843=CARTESIAN_POINT('Ctrl Pts',(17.6666434753763,0.0867087440962768,
4.41485812965324));
#56844=CARTESIAN_POINT('Ctrl Pts',(17.6766006560786,-0.000263771022561289,
4.41536107794487));
#56845=CARTESIAN_POINT('Ctrl Pts',(17.4733993439214,0.000273208168652693,
4.41537657040552));
#56846=CARTESIAN_POINT('Ctrl Pts',(17.4834469616226,-0.0874810350323011,
4.41484969107387));
#56847=CARTESIAN_POINT('Ctrl Pts',(17.5093998580114,-0.314919534962053,
4.34468516187688));
#56848=CARTESIAN_POINT('Ctrl Pts',(17.5512580330878,-0.490957336521241,
3.97057010757845));
#56849=CARTESIAN_POINT('Ctrl Pts',(17.5989738691507,-0.240776309167652,
3.57112706567612));
#56850=CARTESIAN_POINT('Ctrl Pts',(17.6466897052135,0.230513307714322,3.56552463842171));
#56851=CARTESIAN_POINT('Ctrl Pts',(17.6944055412763,0.490119007219086,3.95890762096741));
#56852=CARTESIAN_POINT('Ctrl Pts',(17.7366420875123,0.321513805022658,4.34052027563639));
#56853=CARTESIAN_POINT('Ctrl Pts',(17.7629733550606,0.090710757213051,4.41482206853766));
#56854=CARTESIAN_POINT('Ctrl Pts',(17.7733993439214,-0.000309142357869142,
4.41544738986064));
#56855=CARTESIAN_POINT('Origin',(3.42660065607856,0.,4.));
#56856=CARTESIAN_POINT('',(17.0766006560786,0.000130763213737631,4.41651185352269));
#56857=CARTESIAN_POINT('',(17.1733993439214,0.000198609043858391,4.41644558073401));
#56858=CARTESIAN_POINT('',(3.42660065607856,4.87367679877478E-13,4.415875));
#56859=CARTESIAN_POINT('Ctrl Pts',(17.0766006560786,0.000130763213737628,
4.41651185352269));
#56860=CARTESIAN_POINT('Ctrl Pts',(17.0916854098125,-0.130696083011285,
4.41597403242798));
#56861=CARTESIAN_POINT('Ctrl Pts',(17.1226754422341,-0.400436570105288,
4.2789290971087));
#56862=CARTESIAN_POINT('Ctrl Pts',(17.1695707533433,-0.457413284126125,
3.81922856321607));
#56863=CARTESIAN_POINT('Ctrl Pts',(17.2172865894061,-0.0953372598908034,
3.51748986360026));
#56864=CARTESIAN_POINT('Ctrl Pts',(17.265002425469,0.354288437054553,3.6588476466131));
#56865=CARTESIAN_POINT('Ctrl Pts',(17.3127182615318,0.478565610824392,4.11349088504481));
#56866=CARTESIAN_POINT('Ctrl Pts',(17.349917671735,0.232837083242772,4.38668157013213));
#56867=CARTESIAN_POINT('Ctrl Pts',(17.3712118032506,0.0473568302064652,
4.41579785693967));
#56868=CARTESIAN_POINT('Ctrl Pts',(17.3766006560786,0.000316824918469058,
4.41546566829253));
#56869=CARTESIAN_POINT('Ctrl Pts',(17.1733993439214,0.000198609043858397,
4.41644558073401));
#56870=CARTESIAN_POINT('Ctrl Pts',(17.1880152894969,-0.126615914365149,
4.41569892234974));
#56871=CARTESIAN_POINT('Ctrl Pts',(17.2185365137601,-0.392752582168809,
4.28602487069057));
#56872=CARTESIAN_POINT('Ctrl Pts',(17.2649630167107,-0.462538907526291,
3.83277863809798));
#56873=CARTESIAN_POINT('Ctrl Pts',(17.3126788527736,-0.109506707187599,
3.52050703244687));
#56874=CARTESIAN_POINT('Ctrl Pts',(17.3603946888365,0.344087187338735,3.64856119684745));
#56875=CARTESIAN_POINT('Ctrl Pts',(17.4081105248993,0.481700523269991,4.09934702176407));
#56876=CARTESIAN_POINT('Ctrl Pts',(17.4457787432609,0.241130489326423,4.3831889686244));
#56877=CARTESIAN_POINT('Ctrl Pts',(17.467541682935,0.0514330574063097,4.41568373580506));
#56878=CARTESIAN_POINT('Ctrl Pts',(17.4733993439214,0.000273208168652693,
4.41537657040552));
#56879=CARTESIAN_POINT('Origin',(3.42660065607856,0.,4.));
#56880=CARTESIAN_POINT('',(16.7766006560786,-0.000383680820852129,4.41586226484778));
#56881=CARTESIAN_POINT('',(16.8733993439214,-0.000374684679869397,4.41598699190495));
#56882=CARTESIAN_POINT('',(3.42660065607856,4.87367679877478E-13,4.415875));
#56883=CARTESIAN_POINT('Ctrl Pts',(16.7766006560786,-0.000383680820852189,
4.41586226484779));
#56884=CARTESIAN_POINT('Ctrl Pts',(16.7803484589992,-0.0330197262611539,
4.41616320579436));
#56885=CARTESIAN_POINT('Ctrl Pts',(16.8000015406075,-0.203823433586872,
4.39772119122577));
#56886=CARTESIAN_POINT('Ctrl Pts',(16.8355599009034,-0.464342533291602,
4.16214572651883));
#56887=CARTESIAN_POINT('Ctrl Pts',(16.8832757369663,-0.387520750342007,
3.69712561530174));
#56888=CARTESIAN_POINT('Ctrl Pts',(16.9309915730291,0.0451673004198413,
3.51023971187451));
#56889=CARTESIAN_POINT('Ctrl Pts',(16.978707409092,0.436377524217892,3.7731082169636));
#56890=CARTESIAN_POINT('Ctrl Pts',(17.0264232451548,0.426855552995382,4.24433493759383));
#56891=CARTESIAN_POINT('Ctrl Pts',(17.0590543274837,0.152277829190936,4.41314658311127));
#56892=CARTESIAN_POINT('Ctrl Pts',(17.0757801311249,0.00724700082869906,
4.41654110793655));
#56893=CARTESIAN_POINT('Ctrl Pts',(17.0766006560786,0.000130763213737628,
4.41651185352269));
#56894=CARTESIAN_POINT('Ctrl Pts',(16.8733993439214,-0.000374684679869387,
4.41598699190495));
#56895=CARTESIAN_POINT('Ctrl Pts',(16.8766783386836,-0.0289064002234668,
4.4162516892709));
#56896=CARTESIAN_POINT('Ctrl Pts',(16.8958626121335,-0.195546116663039,
4.40054826733105));
#56897=CARTESIAN_POINT('Ctrl Pts',(16.9309521642709,-0.459365614209645,
4.17575112327883));
#56898=CARTESIAN_POINT('Ctrl Pts',(16.9786680003337,-0.396272847821079,
3.70867019559999));
#56899=CARTESIAN_POINT('Ctrl Pts',(17.0263838363966,0.0307233721630972,
3.5091219099869));
#56900=CARTESIAN_POINT('Ctrl Pts',(17.0740996724594,0.429505846750062,3.76035452756312));
#56901=CARTESIAN_POINT('Ctrl Pts',(17.1218155085223,0.433866493469502,4.23165726989771));
#56902=CARTESIAN_POINT('Ctrl Pts',(17.1549153990096,0.160507997039396,4.41102293437065));
#56903=CARTESIAN_POINT('Ctrl Pts',(17.1721100108093,0.0113854435377776,
4.41651144656345));
#56904=CARTESIAN_POINT('Ctrl Pts',(17.1733993439214,0.000198609043858397,
4.41644558073401));
#56905=CARTESIAN_POINT('Origin',(3.42660065607856,0.,4.));
#56906=CARTESIAN_POINT('',(16.4766006560786,5.2409936866527E-5,4.41519222098806));
#56907=CARTESIAN_POINT('',(16.5733993439214,-1.52272386678698E-5,4.41518677123726));
#56908=CARTESIAN_POINT('',(3.42660065607856,4.87367679877478E-13,4.415875));
#56909=CARTESIAN_POINT('Ctrl Pts',(16.4766006560786,5.2409936866539E-5,
4.41519222098806));
#56910=CARTESIAN_POINT('Ctrl Pts',(16.4849167868736,-0.0726599781719204,
4.41511070701236));
#56911=CARTESIAN_POINT('Ctrl Pts',(16.5091381963562,-0.284551613766983,
4.36224737480062));
#56912=CARTESIAN_POINT('Ctrl Pts',(16.5492648845264,-0.4912502013546,4.02405128938415));
#56913=CARTESIAN_POINT('Ctrl Pts',(16.5969807205893,-0.285919008936969,
3.59980561575594));
#56914=CARTESIAN_POINT('Ctrl Pts',(16.6446965566521,0.181976008816936,3.54306460296116));
#56915=CARTESIAN_POINT('Ctrl Pts',(16.6924123927149,0.482759657613431,3.90593439612197));
#56916=CARTESIAN_POINT('Ctrl Pts',(16.7363804258571,0.351413532087107,4.31989995948535));
#56917=CARTESIAN_POINT('Ctrl Pts',(16.7644431803116,0.105484194296011,4.41488604428797));
#56918=CARTESIAN_POINT('Ctrl Pts',(16.7766006560786,-0.000383680820852189,
4.41586226484779));
#56919=CARTESIAN_POINT('Ctrl Pts',(16.5733993439214,-1.52272386678906E-5,
4.41518677123726));
#56920=CARTESIAN_POINT('Ctrl Pts',(16.5812466665579,-0.0686308195205231,
4.41520910309265));
#56921=CARTESIAN_POINT('Ctrl Pts',(16.6049992678821,-0.276289552895371,
4.36659242126669));
#56922=CARTESIAN_POINT('Ctrl Pts',(16.6446571478939,-0.490328743065594,
4.03850907134293));
#56923=CARTESIAN_POINT('Ctrl Pts',(16.6923729839567,-0.297581432841348,
3.60840005658827));
#56924=CARTESIAN_POINT('Ctrl Pts',(16.7400888200196,0.168439486040012,3.53790329540825));
#56925=CARTESIAN_POINT('Ctrl Pts',(16.7878046560824,0.479779833116189,3.89175704832657));
#56926=CARTESIAN_POINT('Ctrl Pts',(16.832241497383,0.359412856911567,4.31386464726761));
#56927=CARTESIAN_POINT('Ctrl Pts',(16.860773059996,0.109491163683573,4.41496773315674));
#56928=CARTESIAN_POINT('Ctrl Pts',(16.8733993439214,-0.000374684679869387,
4.41598699190495));
#56929=CARTESIAN_POINT('Origin',(3.42660065607856,0.,4.));
#56930=CARTESIAN_POINT('',(16.1766006560786,0.000364146841390381,4.41605523138122));
#56931=CARTESIAN_POINT('',(16.2733993439214,0.000380345806842055,4.41593091837313));
#56932=CARTESIAN_POINT('',(3.42660065607856,4.87367679877478E-13,4.415875));
#56933=CARTESIAN_POINT('Ctrl Pts',(16.1766006560786,0.000364146841390366,
4.41605523138122));
#56934=CARTESIAN_POINT('Ctrl Pts',(16.1894851147479,-0.111700864104492,
4.41502624848758));
#56935=CARTESIAN_POINT('Ctrl Pts',(16.2182748521048,-0.363797281821349,
4.31045679267864));
#56936=CARTESIAN_POINT('Ctrl Pts',(16.2629698681494,-0.477960913216358,
3.88398883549692));
#56937=CARTESIAN_POINT('Ctrl Pts',(16.3106857042122,-0.160921706883503,
3.53523185446324));
#56938=CARTESIAN_POINT('Ctrl Pts',(16.358401540275,0.303894378979202,3.6132786128531));
#56939=CARTESIAN_POINT('Ctrl Pts',(16.4061173763379,0.489639580609251,4.04645757153336));
#56940=CARTESIAN_POINT('Ctrl Pts',(16.4455170816057,0.271734615807756,4.36891289568356));
#56941=CARTESIAN_POINT('Ctrl Pts',(16.4690115081859,0.0664083969439258,
4.41526660914191));
#56942=CARTESIAN_POINT('Ctrl Pts',(16.4766006560786,5.2409936866539E-5,
4.41519222098806));
#56943=CARTESIAN_POINT('Ctrl Pts',(16.2733993439214,0.000380345806842052,
4.41593091837313));
#56944=CARTESIAN_POINT('Ctrl Pts',(16.2858149944323,-0.107690075887363,
4.41492720978183));
#56945=CARTESIAN_POINT('Ctrl Pts',(16.3141359236307,-0.35582464097624,4.31660057631701));
#56946=CARTESIAN_POINT('Ctrl Pts',(16.3583621315169,-0.481170314810987,
3.89811598262401));
#56947=CARTESIAN_POINT('Ctrl Pts',(16.4060779675797,-0.174540169679895,
3.54017290856226));
#56948=CARTESIAN_POINT('Ctrl Pts',(16.4537938036425,0.292372898913969,3.60449612791703));
#56949=CARTESIAN_POINT('Ctrl Pts',(16.5015096397054,0.490795435699827,4.0320166386149));
#56950=CARTESIAN_POINT('Ctrl Pts',(16.5413781531317,0.280003220364278,4.36466130212541));
#56951=CARTESIAN_POINT('Ctrl Pts',(16.5653413878703,0.0704421061260754,
4.4151638399628));
#56952=CARTESIAN_POINT('Ctrl Pts',(16.5733993439214,-1.52272386678906E-5,
4.41518677123726));
#56953=CARTESIAN_POINT('Origin',(3.42660065607856,0.,4.));
#56954=CARTESIAN_POINT('',(15.8766006560786,-0.00023258108979477,4.41639972388928));
#56955=CARTESIAN_POINT('',(15.9733993439214,-0.000169011902647176,4.4164782780785));
#56956=CARTESIAN_POINT('',(3.42660065607856,4.87367679877478E-13,4.415875));
#56957=CARTESIAN_POINT('Ctrl Pts',(15.8766006560786,-0.000232581089794846,
4.41639972388928));
#56958=CARTESIAN_POINT('Ctrl Pts',(15.8781481639346,-0.0136633580705269,
4.41648966084242));
#56959=CARTESIAN_POINT('Ctrl Pts',(15.8956009504782,-0.165044849757219,
4.40979870506104));
#56960=CARTESIAN_POINT('Ctrl Pts',(15.9289590157095,-0.437567097060412,
4.22458909239344));
#56961=CARTESIAN_POINT('Ctrl Pts',(15.9766748517724,-0.425562075928853,
3.75341909160864));
#56962=CARTESIAN_POINT('Ctrl Pts',(16.0243906878352,-0.0227568523576073,
3.50868813313462));
#56963=CARTESIAN_POINT('Ctrl Pts',(16.072106523898,0.400946338892803,3.71513642180785));
#56964=CARTESIAN_POINT('Ctrl Pts',(16.1198223599609,0.456454337785543,4.1831793175245));
#56965=CARTESIAN_POINT('Ctrl Pts',(16.1546537373544,0.190990792023167,4.40204523666471));
#56966=CARTESIAN_POINT('Ctrl Pts',(16.1735798360603,0.0266382990664043,
4.41629648110721));
#56967=CARTESIAN_POINT('Ctrl Pts',(16.1766006560786,0.000364146841390366,
4.41605523138122));
#56968=CARTESIAN_POINT('Ctrl Pts',(15.9733993439214,-0.000169011902647174,
4.4164782780785));
#56969=CARTESIAN_POINT('Ctrl Pts',(15.974478043619,-0.00952634975615679,
4.4165263696097));
#56970=CARTESIAN_POINT('Ctrl Pts',(15.9914620220042,-0.156808910032117,
4.4119928338179));
#56971=CARTESIAN_POINT('Ctrl Pts',(16.024351279077,-0.430762722000766,4.23737881579128));
#56972=CARTESIAN_POINT('Ctrl Pts',(16.0720671151398,-0.432639725453012,
3.76605963834362));
#56973=CARTESIAN_POINT('Ctrl Pts',(16.1197829512026,-0.0372170120039125,
3.50957149464017));
#56974=CARTESIAN_POINT('Ctrl Pts',(16.1674987872655,0.392382656225717,3.70345139362117));
#56975=CARTESIAN_POINT('Ctrl Pts',(16.2152146233283,0.461651293660056,4.16965644082667));
#56976=CARTESIAN_POINT('Ctrl Pts',(16.2505148088803,0.199264245432362,4.39929555075695));
#56977=CARTESIAN_POINT('Ctrl Pts',(16.2699097157447,0.0307553622657438,
4.41621302761729));
#56978=CARTESIAN_POINT('Ctrl Pts',(16.2733993439214,0.000380345806842052,
4.41593091837313));
#56979=CARTESIAN_POINT('Origin',(3.42660065607856,0.,4.));
#56980=CARTESIAN_POINT('',(15.5766006560786,-0.000245472137683418,4.41533389801214));
#56981=CARTESIAN_POINT('',(15.6733993439214,-0.00029394562308721,4.41541483535501));
#56982=CARTESIAN_POINT('',(3.42660065607856,4.87367679877478E-13,4.415875));
#56983=CARTESIAN_POINT('Ctrl Pts',(15.5766006560786,-0.000245472137683396,
4.41533389801214));
#56984=CARTESIAN_POINT('Ctrl Pts',(15.5827164918089,-0.0536739331835165,
4.41562024719655));
#56985=CARTESIAN_POINT('Ctrl Pts',(15.6047376062269,-0.245697356182912,
4.38119912149661));
#56986=CARTESIAN_POINT('Ctrl Pts',(15.6426639993325,-0.483248643997369,
4.09152034160055));
#56987=CARTESIAN_POINT('Ctrl Pts',(15.6903798353953,-0.338341267922855,
3.64302603558196));
#56988=CARTESIAN_POINT('Ctrl Pts',(15.7380956714582,0.117270100534806,3.52234641383892));
#56989=CARTESIAN_POINT('Ctrl Pts',(15.785811507521,0.465190531238913,3.84030342991275));
#56990=CARTESIAN_POINT('Ctrl Pts',(15.8319798357278,0.388490242362186,4.28984418805176));
#56991=CARTESIAN_POINT('Ctrl Pts',(15.862242885247,0.124378106492246,4.41556528924811));
#56992=CARTESIAN_POINT('Ctrl Pts',(15.8766006560786,-0.000232581089794846,
4.41639972388928));
#56993=CARTESIAN_POINT('Ctrl Pts',(15.6733993439214,-0.000293945623087231,
4.41541483535501));
#56994=CARTESIAN_POINT('Ctrl Pts',(15.6790463714933,-0.0496027558454661,
4.41573527017753));
#56995=CARTESIAN_POINT('Ctrl Pts',(15.7005986777528,-0.23740431922453,4.38477730872224));
#56996=CARTESIAN_POINT('Ctrl Pts',(15.7380562626999,-0.480343569999647,
4.1057131950703));
#56997=CARTESIAN_POINT('Ctrl Pts',(15.7857720987628,-0.348708030819167,
3.6531456586776));
#56998=CARTESIAN_POINT('Ctrl Pts',(15.8334879348256,0.103151458625294,3.5190998009613));
#56999=CARTESIAN_POINT('Ctrl Pts',(15.8812037708885,0.460285376424935,3.82667199562295));
#57000=CARTESIAN_POINT('Ctrl Pts',(15.9278409072537,0.396214095655672,4.28286244744368));
#57001=CARTESIAN_POINT('Ctrl Pts',(15.9585727649314,0.128446309981357,4.41581726659612));
#57002=CARTESIAN_POINT('Ctrl Pts',(15.9733993439214,-0.000169011902647174,
4.4164782780785));
#57003=CARTESIAN_POINT('Origin',(3.42660065607856,0.,4.));
#57004=CARTESIAN_POINT('',(15.2766006560786,0.000330084823988869,4.41550084660604));
#57005=CARTESIAN_POINT('',(15.3733993439214,0.000289868078815952,4.41540680128743));
#57006=CARTESIAN_POINT('',(3.42660065607856,4.87367679877478E-13,4.415875));
#57007=CARTESIAN_POINT('Ctrl Pts',(15.2766006560786,0.000330084823988861,
4.41550084660604));
#57008=CARTESIAN_POINT('Ctrl Pts',(15.2872848196833,-0.0929135079625664,
4.41481081573461));
#57009=CARTESIAN_POINT('Ctrl Pts',(15.3138742619755,-0.32600240339937,4.33760928826424));
#57010=CARTESIAN_POINT('Ctrl Pts',(15.3563689829555,-0.489387968817152,
3.95096286275689));
#57011=CARTESIAN_POINT('Ctrl Pts',(15.4040848190183,-0.223435404337718,
3.56184267101825));
#57012=CARTESIAN_POINT('Ctrl Pts',(15.4518006550811,0.24770132994065,3.57508909640066));
#57013=CARTESIAN_POINT('Ctrl Pts',(15.499516491144,0.491370121559653,3.97853774265298));
#57014=CARTESIAN_POINT('Ctrl Pts',(15.5411164914764,0.310410063586636,4.3474585185963));
#57015=CARTESIAN_POINT('Ctrl Pts',(15.5668112131213,0.0852759340546689,
4.41487554708019));
#57016=CARTESIAN_POINT('Ctrl Pts',(15.5766006560786,-0.000245472137683396,
4.41533389801214));
#57017=CARTESIAN_POINT('Ctrl Pts',(15.3733993439214,0.000289868078815973,
4.41540680128743));
#57018=CARTESIAN_POINT('Ctrl Pts',(15.3836146993676,-0.0889130762729256,
4.41483587894927));
#57019=CARTESIAN_POINT('Ctrl Pts',(15.4097353335015,-0.317845114095608,
4.34285359523591));
#57020=CARTESIAN_POINT('Ctrl Pts',(15.4517612463229,-0.490619905976795,
3.96539750426199));
#57021=CARTESIAN_POINT('Ctrl Pts',(15.4994770823858,-0.236243011612202,
3.56861332390027));
#57022=CARTESIAN_POINT('Ctrl Pts',(15.5471929184486,0.235079475381852,3.56797816593814));
#57023=CARTESIAN_POINT('Ctrl Pts',(15.5949087545115,0.490524862970081,3.9640753057054));
#57024=CARTESIAN_POINT('Ctrl Pts',(15.6369775630024,0.318592711010818,4.34238143198936));
#57025=CARTESIAN_POINT('Ctrl Pts',(15.6631410928057,0.0892792238074376,
4.41483274135358));
#57026=CARTESIAN_POINT('Ctrl Pts',(15.6733993439214,-0.000293945623087231,
4.41541483535501));
#57027=CARTESIAN_POINT('Origin',(3.42660065607856,0.,4.));
#57028=CARTESIAN_POINT('',(14.9766006560786,0.000104941934236194,4.41652945172571));
#57029=CARTESIAN_POINT('',(15.0733993439214,0.000175165248676303,4.41647198785975));
#57030=CARTESIAN_POINT('',(3.42660065607856,4.87367679877478E-13,4.415875));
#57031=CARTESIAN_POINT('Ctrl Pts',(14.9766006560786,0.000104941934236227,
4.41652945172572));
#57032=CARTESIAN_POINT('Ctrl Pts',(14.9918531475576,-0.132161740438444,
4.41608294134065));
#57033=CARTESIAN_POINT('Ctrl Pts',(15.0230109177242,-0.40316752945992,4.27633971254324));
#57034=CARTESIAN_POINT('Ctrl Pts',(15.0700739665785,-0.455482716161518,
3.8144178884426));
#57035=CARTESIAN_POINT('Ctrl Pts',(15.1177898026413,-0.0902467530057116,
3.51651189422706));
#57036=CARTESIAN_POINT('Ctrl Pts',(15.1655056387041,0.357864192060027,3.66260046696357));
#57037=CARTESIAN_POINT('Ctrl Pts',(15.2132214747669,0.47734294310866,4.11852822244656));
#57038=CARTESIAN_POINT('Ctrl Pts',(15.2502531472251,0.229869832763757,4.3878938710325));
#57039=CARTESIAN_POINT('Ctrl Pts',(15.2713795409956,0.0458961718568525,
4.41583804947224));
#57040=CARTESIAN_POINT('Ctrl Pts',(15.2766006560786,0.000330084823988861,
4.41550084660604));
#57041=CARTESIAN_POINT('Ctrl Pts',(15.0733993439214,0.000175165248676341,
4.41647198785975));
#57042=CARTESIAN_POINT('Ctrl Pts',(15.0881830272419,-0.128073190246274,
4.41579247653651));
#57043=CARTESIAN_POINT('Ctrl Pts',(15.1188719892501,-0.395510344386944,
4.28350986851547));
#57044=CARTESIAN_POINT('Ctrl Pts',(15.1654662299459,-0.46075086019608,3.82791319143947));
#57045=CARTESIAN_POINT('Ctrl Pts',(15.2131820660087,-0.104447211543591,
3.51937956259357));
#57046=CARTESIAN_POINT('Ctrl Pts',(15.2608979020716,0.347771918596306,3.652207076714));
#57047=CARTESIAN_POINT('Ctrl Pts',(15.3086137381344,0.480626744730421,4.10441818376995));
#57048=CARTESIAN_POINT('Ctrl Pts',(15.346114218751,0.238163166260598,4.38445638366753));
#57049=CARTESIAN_POINT('Ctrl Pts',(15.36770942068,0.0499756483669043,4.41572480336754));
#57050=CARTESIAN_POINT('Ctrl Pts',(15.3733993439214,0.000289868078815973,
4.41540680128743));
#57051=CARTESIAN_POINT('Origin',(3.42660065607856,0.,4.));
#57052=CARTESIAN_POINT('',(14.6766006560786,-0.000383732061438463,4.41581798673635));
#57053=CARTESIAN_POINT('',(14.7733993439214,-0.000379407362125217,4.41594234696178));
#57054=CARTESIAN_POINT('',(3.42660065607856,4.87367679877478E-13,4.415875));
#57055=CARTESIAN_POINT('Ctrl Pts',(14.6766006560786,-0.000383732061438387,
4.41581798673635));
#57056=CARTESIAN_POINT('Ctrl Pts',(14.6805161967443,-0.0344897130604965,
4.41612948839573));
#57057=CARTESIAN_POINT('Ctrl Pts',(14.7003370160976,-0.206786574235377,
4.39667515056147));
#57058=CARTESIAN_POINT('Ctrl Pts',(14.7360631141386,-0.466025611307368,
4.15724297904063));
#57059=CARTESIAN_POINT('Ctrl Pts',(14.7837789502014,-0.38430721152129,3.69305832471834));
#57060=CARTESIAN_POINT('Ctrl Pts',(14.8314947862642,0.0503264139313189,
3.51074293371195));
#57061=CARTESIAN_POINT('Ctrl Pts',(14.8792106223271,0.438744519099385,3.77771983486548));
#57062=CARTESIAN_POINT('Ctrl Pts',(14.9269264583899,0.42425678142631,4.24882003188202));
#57063=CARTESIAN_POINT('Ctrl Pts',(14.9593898029737,0.149335702075518,4.41387566524124));
#57064=CARTESIAN_POINT('Ctrl Pts',(14.97594786887,0.00576578747519492,4.41654856180149));
#57065=CARTESIAN_POINT('Ctrl Pts',(14.9766006560786,0.000104941934236227,
4.41652945172572));
#57066=CARTESIAN_POINT('Ctrl Pts',(14.7733993439214,-0.000379407362125234,
4.41594234696178));
#57067=CARTESIAN_POINT('Ctrl Pts',(14.7768460764287,-0.0303789312965351,
4.41622104989506));
#57068=CARTESIAN_POINT('Ctrl Pts',(14.7961980876235,-0.198506931257387,
4.39955296987463));
#57069=CARTESIAN_POINT('Ctrl Pts',(14.831455377506,-0.461192356972643,4.17090007232882));
#57070=CARTESIAN_POINT('Ctrl Pts',(14.8791712135689,-0.393180492164677,
3.7045100248179));
#57071=CARTESIAN_POINT('Ctrl Pts',(14.9268870496317,0.0358950684576197,
3.50947296821438));
#57072=CARTESIAN_POINT('Ctrl Pts',(14.9746028856945,0.432007635398663,3.76489443262817));
#57073=CARTESIAN_POINT('Ctrl Pts',(15.0223187217574,0.431400943461215,4.23621695712364));
#57074=CARTESIAN_POINT('Ctrl Pts',(15.0552508744997,0.157562060208247,4.41179740605063));
#57075=CARTESIAN_POINT('Ctrl Pts',(15.0722777485543,0.00990499767517082,
4.41652354042182));
#57076=CARTESIAN_POINT('Ctrl Pts',(15.0733993439214,0.000175165248676341,
4.41647198785975));
#57077=CARTESIAN_POINT('Origin',(3.42660065607856,0.,4.));
#57078=CARTESIAN_POINT('',(14.3766006560786,7.63317591858645E-5,4.41519896243726));
#57079=CARTESIAN_POINT('',(14.4733993439214,9.02664646690309E-6,4.41518644689786));
#57080=CARTESIAN_POINT('',(3.42660065607856,4.87367679877478E-13,4.415875));
#57081=CARTESIAN_POINT('Ctrl Pts',(14.3766006560786,7.63317591858798E-5,
4.41519896243726));
#57082=CARTESIAN_POINT('Ctrl Pts',(14.3850845246186,-0.0740996743586071,
4.41507773880187));
#57083=CARTESIAN_POINT('Ctrl Pts',(14.4094736718463,-0.287504468978829,
4.360651101065));
#57084=CARTESIAN_POINT('Ctrl Pts',(14.4497680977616,-0.491476396904638,
4.01887262932433));
#57085=CARTESIAN_POINT('Ctrl Pts',(14.4974839338244,-0.281685449746218,
3.59681451879656));
#57086=CARTESIAN_POINT('Ctrl Pts',(14.5451997698872,0.186781580201919,3.54500783946397));
#57087=CARTESIAN_POINT('Ctrl Pts',(14.59291560595,0.483724211046603,3.91102746210588));
#57088=CARTESIAN_POINT('Ctrl Pts',(14.6367159013472,0.348540265561382,4.32201186060262));
#57089=CARTESIAN_POINT('Ctrl Pts',(14.6646109180567,0.104051852208848,4.41486414061182));
#57090=CARTESIAN_POINT('Ctrl Pts',(14.6766006560786,-0.000383732061438387,
4.41581798673635));
#57091=CARTESIAN_POINT('Ctrl Pts',(14.4733993439214,9.0266464668684E-6,
4.41518644689786));
#57092=CARTESIAN_POINT('Ctrl Pts',(14.481414404303,-0.0700733710850898,
4.41517292627706));
#57093=CARTESIAN_POINT('Ctrl Pts',(14.5053347433722,-0.279247125311621,
4.3650573561381));
#57094=CARTESIAN_POINT('Ctrl Pts',(14.545160361129,-0.490707361486496,4.03333931965322));
#57095=CARTESIAN_POINT('Ctrl Pts',(14.5928761971918,-0.293437803431633,
3.60528557111603));
#57096=CARTESIAN_POINT('Ctrl Pts',(14.6405920332547,0.173300204635467,3.53970415608515));
#57097=CARTESIAN_POINT('Ctrl Pts',(14.6883078693175,0.480893968219416,3.89681949708321));
#57098=CARTESIAN_POINT('Ctrl Pts',(14.7325769728731,0.356556173733762,4.31604662460621));
#57099=CARTESIAN_POINT('Ctrl Pts',(14.760940797741,0.10805675748006,4.41493494840171));
#57100=CARTESIAN_POINT('Ctrl Pts',(14.7733993439214,-0.000379407362125234,
4.41594234696178));
#57101=CARTESIAN_POINT('Origin',(3.42660065607856,0.,4.));
#57102=CARTESIAN_POINT('',(14.0766006560786,0.000355193352615291,4.41609897421413));
#57103=CARTESIAN_POINT('',(14.1733993439214,0.000376051973931104,4.41597558743442));
#57104=CARTESIAN_POINT('',(3.42660065607856,4.87367679877478E-13,4.415875));
#57105=CARTESIAN_POINT('Ctrl Pts',(14.0766006560786,0.000355193352615277,
4.41609897421413));
#57106=CARTESIAN_POINT('Ctrl Pts',(14.0896528524929,-0.113137957382804,
4.41506966208575));
#57107=CARTESIAN_POINT('Ctrl Pts',(14.1186103275949,-0.366637448157006,
4.30821039815648));
#57108=CARTESIAN_POINT('Ctrl Pts',(14.1634730813845,-0.476711717661702,
3.87895801102093));
#57109=CARTESIAN_POINT('Ctrl Pts',(14.2111889174473,-0.156014541823709,
3.53356170012368));
#57110=CARTESIAN_POINT('Ctrl Pts',(14.2589047535102,0.307953188363286,3.61650285707861));
#57111=CARTESIAN_POINT('Ctrl Pts',(14.306620589573,0.4891227672074,4.05161534124029));
#57112=CARTESIAN_POINT('Ctrl Pts',(14.3458525570958,0.268773633406098,4.37039329245586));
#57113=CARTESIAN_POINT('Ctrl Pts',(14.369179245931,0.0649630708582953,4.4153050049005));
#57114=CARTESIAN_POINT('Ctrl Pts',(14.3766006560786,7.63317591858798E-5,
4.41519896243726));
#57115=CARTESIAN_POINT('Ctrl Pts',(14.1733993439214,0.000376051973931098,
4.41597558743442));
#57116=CARTESIAN_POINT('Ctrl Pts',(14.1859827321773,-0.109124255432428,
4.41495896305428));
#57117=CARTESIAN_POINT('Ctrl Pts',(14.2144713991208,-0.358682910161539,
4.31442504752535));
#57118=CARTESIAN_POINT('Ctrl Pts',(14.258865344752,-0.480069828122688,3.8930505494253));
#57119=CARTESIAN_POINT('Ctrl Pts',(14.3065811808148,-0.169684322438749,
3.53835895376334));
#57120=CARTESIAN_POINT('Ctrl Pts',(14.3542970168777,0.296524907469595,3.60759943412104));
#57121=CARTESIAN_POINT('Ctrl Pts',(14.4020128529405,0.49043075222644,4.0371873919842));
#57122=CARTESIAN_POINT('Ctrl Pts',(14.4417136286217,0.277046036654804,4.36620192284859));
#57123=CARTESIAN_POINT('Ctrl Pts',(14.4655091256154,0.0689998253659925,
4.41519975692232));
#57124=CARTESIAN_POINT('Ctrl Pts',(14.4733993439214,9.0266464668684E-6,
4.41518644689786));
#57125=CARTESIAN_POINT('Origin',(3.42660065607856,0.,4.));
#57126=CARTESIAN_POINT('',(13.7766006560786,-0.000253139125078747,4.41636688691614));
#57127=CARTESIAN_POINT('',(13.8733993439214,-0.000192710833643805,4.4164526008213));
#57128=CARTESIAN_POINT('',(3.42660065607856,4.87367679877478E-13,4.415875));
#57129=CARTESIAN_POINT('Ctrl Pts',(13.7766006560786,-0.000253139125078718,
4.41636688691614));
#57130=CARTESIAN_POINT('Ctrl Pts',(13.7783159016796,-0.0151427949580853,
4.41647347977994));
#57131=CARTESIAN_POINT('Ctrl Pts',(13.7959364259683,-0.167994124135391,
4.40898222403799));
#57132=CARTESIAN_POINT('Ctrl Pts',(13.8294622289446,-0.439909757638992,
4.21996506537626));
#57133=CARTESIAN_POINT('Ctrl Pts',(13.8771780650075,-0.422939705734467,
3.74894775411238));
#57134=CARTESIAN_POINT('Ctrl Pts',(13.9248939010703,-0.0175776142901187,
3.50847558318244));
#57135=CARTESIAN_POINT('Ctrl Pts',(13.9726097371332,0.403926270823208,3.71937784729135));
#57136=CARTESIAN_POINT('Ctrl Pts',(14.020325573196,0.454498446235019,4.18797975215946));
#57137=CARTESIAN_POINT('Ctrl Pts',(14.0549892128445,0.188032430710383,4.40299531219535));
#57138=CARTESIAN_POINT('Ctrl Pts',(14.0737475738053,0.0251636842930195,
4.41632397176197));
#57139=CARTESIAN_POINT('Ctrl Pts',(14.0766006560786,0.000355193352615277,
4.41609897421413));
#57140=CARTESIAN_POINT('Ctrl Pts',(13.8733993439214,-0.000192710833643682,
4.4164526008213));
#57141=CARTESIAN_POINT('Ctrl Pts',(13.874645781364,-0.0110068809386406,
4.41651469495978));
#57142=CARTESIAN_POINT('Ctrl Pts',(13.8917974974943,-0.15975450351916,4.41122255187585));
#57143=CARTESIAN_POINT('Ctrl Pts',(13.9248544923121,-0.433240552373761,
4.23282579030437));
#57144=CARTESIAN_POINT('Ctrl Pts',(13.9725703283749,-0.430150181893835,
3.76151300691929));
#57145=CARTESIAN_POINT('Ctrl Pts',(14.0202861644378,-0.032046280669499,
3.50920649887429));
#57146=CARTESIAN_POINT('Ctrl Pts',(14.0680020005006,0.39548621318905,3.70760321474174));
#57147=CARTESIAN_POINT('Ctrl Pts',(14.1157178365634,0.459837632138507,4.1745123976147));
#57148=CARTESIAN_POINT('Ctrl Pts',(14.1508502843704,0.196303200904851,4.40029544879449));
#57149=CARTESIAN_POINT('Ctrl Pts',(14.1700774534897,0.0292830534939708,
4.41624396624722));
#57150=CARTESIAN_POINT('Ctrl Pts',(14.1733993439214,0.000376051973931098,
4.41597558743442));
#57151=CARTESIAN_POINT('Origin',(3.42660065607856,0.,4.));
#57152=CARTESIAN_POINT('',(13.4766006560786,-0.000226204729293368,4.4153088088013));
#57153=CARTESIAN_POINT('',(13.5733993439214,-0.000277574767750837,4.41538411867388));
#57154=CARTESIAN_POINT('',(3.42660065607856,4.87367679877478E-13,4.415875));
#57155=CARTESIAN_POINT('Ctrl Pts',(13.4766006560786,-0.000226204729293314,
4.4153088088013));
#57156=CARTESIAN_POINT('Ctrl Pts',(13.482884229554,-0.0551283395969922,
4.41557894444213));
#57157=CARTESIAN_POINT('Ctrl Pts',(13.505073081717,-0.248664136397309,4.37988069596112));
#57158=CARTESIAN_POINT('Ctrl Pts',(13.5431672125676,-0.484186345555107,
4.08642226350871));
#57159=CARTESIAN_POINT('Ctrl Pts',(13.5908830486304,-0.334560300710407,
3.63948005597396));
#57160=CARTESIAN_POINT('Ctrl Pts',(13.6385988846933,0.122297616148583,3.52360886035071));
#57161=CARTESIAN_POINT('Ctrl Pts',(13.6863147207561,0.466847750307624,3.8452149784873));
#57162=CARTESIAN_POINT('Ctrl Pts',(13.7323153112179,0.38570983934117,4.29229218593957));
#57163=CARTESIAN_POINT('Ctrl Pts',(13.762410622992,0.122927301498021,4.41548505619568));
#57164=CARTESIAN_POINT('Ctrl Pts',(13.7766006560786,-0.000253139125078718,
4.41636688691614));
#57165=CARTESIAN_POINT('Ctrl Pts',(13.5733993439214,-0.000277574767750817,
4.41538411867388));
#57166=CARTESIAN_POINT('Ctrl Pts',(13.5792141092383,-0.0510604653080308,
4.41569425641003));
#57167=CARTESIAN_POINT('Ctrl Pts',(13.6009341532429,-0.240371663949131,
4.38351498152559));
#57168=CARTESIAN_POINT('Ctrl Pts',(13.6385594759351,-0.481431012491488,
4.10064494554323));
#57169=CARTESIAN_POINT('Ctrl Pts',(13.6862753119979,-0.345033139360895,
3.64948986092447));
#57170=CARTESIAN_POINT('Ctrl Pts',(13.7339911480608,0.108213974662067,3.52021363031051));
#57171=CARTESIAN_POINT('Ctrl Pts',(13.7817069841236,0.462086530666827,3.83153260544464));
#57172=CARTESIAN_POINT('Ctrl Pts',(13.8281763827438,0.393458703070077,4.28538422885222));
#57173=CARTESIAN_POINT('Ctrl Pts',(13.8587405026764,0.126988323162951,4.4157223370415));
#57174=CARTESIAN_POINT('Ctrl Pts',(13.8733993439214,-0.000192710833643682,
4.4164526008213));
#57175=CARTESIAN_POINT('Origin',(3.42660065607856,0.,4.));
#57176=CARTESIAN_POINT('',(13.1766006560786,0.000342007958933446,4.41553758638116));
#57177=CARTESIAN_POINT('',(13.2733993439214,0.000305371599794934,4.41543889539504));
#57178=CARTESIAN_POINT('',(3.42660065607856,4.87367679877478E-13,4.415875));
#57179=CARTESIAN_POINT('Ctrl Pts',(13.1766006560786,0.000342007958933428,
4.41553758638117));
#57180=CARTESIAN_POINT('Ctrl Pts',(13.1874525574283,-0.0943443719380771,
4.41480703635833));
#57181=CARTESIAN_POINT('Ctrl Pts',(13.2142097374657,-0.328913583769224,
4.33568767983454));
#57182=CARTESIAN_POINT('Ctrl Pts',(13.2568721961906,-0.488843983144383,
3.94580788806928));
#57183=CARTESIAN_POINT('Ctrl Pts',(13.3045880322534,-0.218805220893238,
3.55951220202843));
#57184=CARTESIAN_POINT('Ctrl Pts',(13.3523038683163,0.252165742455243,3.57772323864086));
#57185=CARTESIAN_POINT('Ctrl Pts',(13.4000197043791,0.491569024438394,3.98371752277252));
#57186=CARTESIAN_POINT('Ctrl Pts',(13.4414519669665,0.307476227900318,4.34923088347422));
#57187=CARTESIAN_POINT('Ctrl Pts',(13.4669789508664,0.0838425436168888,
4.41489516431802));
#57188=CARTESIAN_POINT('Ctrl Pts',(13.4766006560786,-0.000226204729293314,
4.4153088088013));
#57189=CARTESIAN_POINT('Ctrl Pts',(13.2733993439214,0.000305371599794949,
4.41543889539504));
#57190=CARTESIAN_POINT('Ctrl Pts',(13.2837824371127,-0.0903447040275099,
4.41482455235666));
#57191=CARTESIAN_POINT('Ctrl Pts',(13.3100708089916,-0.320767143545349,
4.3409984814332));
#57192=CARTESIAN_POINT('Ctrl Pts',(13.352264459558,-0.490227979701372,3.96022874442655));
#57193=CARTESIAN_POINT('Ctrl Pts',(13.3999802956209,-0.23168347330409,3.56614749850931));
#57194=CARTESIAN_POINT('Ctrl Pts',(13.4476961316837,0.239619531536799,3.57047968038978));
#57195=CARTESIAN_POINT('Ctrl Pts',(13.4954119677466,0.490876233547033,3.96924698078795));
#57196=CARTESIAN_POINT('Ctrl Pts',(13.5373130384925,0.315668023336251,4.34421900798688));
#57197=CARTESIAN_POINT('Ctrl Pts',(13.5633088305507,0.0878472949503496,
4.41484592860038));
#57198=CARTESIAN_POINT('Ctrl Pts',(13.5733993439214,-0.000277574767750817,
4.41538411867388));
#57199=CARTESIAN_POINT('Origin',(3.42660065607856,0.,4.));
#57200=CARTESIAN_POINT('',(12.8766006560786,7.85109994957766E-5,4.41654344863055));
#57201=CARTESIAN_POINT('',(12.9733993439214,0.000150764780949702,4.41649545414489));
#57202=CARTESIAN_POINT('',(3.42660065607856,4.87367679877478E-13,4.415875));
#57203=CARTESIAN_POINT('Ctrl Pts',(12.8766006560786,7.85109994958138E-5,
4.41654344863055));
#57204=CARTESIAN_POINT('Ctrl Pts',(12.8920208853026,-0.133630732206743,
4.41619751255639));
#57205=CARTESIAN_POINT('Ctrl Pts',(12.9233463932143,-0.405888408666218,
4.27372356364211));
#57206=CARTESIAN_POINT('Ctrl Pts',(12.9705771798136,-0.453501555338242,
3.80962782724943));
#57207=CARTESIAN_POINT('Ctrl Pts',(13.0182930158764,-0.0851462219395619,
3.51558762841831));
#57208=CARTESIAN_POINT('Ctrl Pts',(13.0660088519392,0.361400197209248,3.66639076405307));
#57209=CARTESIAN_POINT('Ctrl Pts',(13.1137246880021,0.476067254403989,4.1235523942958));
#57210=CARTESIAN_POINT('Ctrl Pts',(13.1505886227152,0.226902767145371,4.38908671404106));
#57211=CARTESIAN_POINT('Ctrl Pts',(13.1715472787407,0.0444343739838573,
4.41587777975472));
#57212=CARTESIAN_POINT('Ctrl Pts',(13.1766006560786,0.000342007958933428,
4.41553758638117));
#57213=CARTESIAN_POINT('Ctrl Pts',(12.9733993439214,0.000150764780949724,
4.4164954541449));
#57214=CARTESIAN_POINT('Ctrl Pts',(12.988350764987,-0.12953330947047,4.41589144324702));
#57215=CARTESIAN_POINT('Ctrl Pts',(13.0192074647402,-0.39825874617628,4.28096832590395));
#57216=CARTESIAN_POINT('Ctrl Pts',(13.065969443181,-0.458911634846768,3.82306685936703));
#57217=CARTESIAN_POINT('Ctrl Pts',(13.1136852792439,-0.0993761143989603,
3.51830547777773));
#57218=CARTESIAN_POINT('Ctrl Pts',(13.1614011153067,0.351418020999476,3.65589158776806));
#57219=CARTESIAN_POINT('Ctrl Pts',(13.2091169513695,0.479499580452807,4.10947774749948));
#57220=CARTESIAN_POINT('Ctrl Pts',(13.2464496942411,0.235195791588524,4.38570395495548));
#57221=CARTESIAN_POINT('Ctrl Pts',(13.2678771584251,0.0485170676377186,
4.41576563003508));
#57222=CARTESIAN_POINT('Ctrl Pts',(13.2733993439214,0.000305371599794949,
4.41543889539504));
#57223=CARTESIAN_POINT('Origin',(3.42660065607856,0.,4.));
#57224=CARTESIAN_POINT('',(12.5766006560786,-0.000382134531266273,4.41577416496379));
#57225=CARTESIAN_POINT('',(12.6733993439214,-0.000382453243898073,4.41589767499446));
#57226=CARTESIAN_POINT('',(3.42660065607856,4.87367679877478E-13,4.415875));
#57227=CARTESIAN_POINT('Ctrl Pts',(12.5766006560786,-0.000382134531266193,
4.41577416496379));
#57228=CARTESIAN_POINT('Ctrl Pts',(12.5806839344893,-0.0359587315295452,
4.41609477791077));
#57229=CARTESIAN_POINT('Ctrl Pts',(12.6006724915877,-0.209750441210566,
4.39561070447123));
#57230=CARTESIAN_POINT('Ctrl Pts',(12.6365663273737,-0.4676569254097,4.15232276575852));
#57231=CARTESIAN_POINT('Ctrl Pts',(12.6842821634365,-0.381050985679211,
3.68902512775968));
#57232=CARTESIAN_POINT('Ctrl Pts',(12.7319979994994,0.0554799374235607,
3.5113004999026));
#57233=CARTESIAN_POINT('Ctrl Pts',(12.7797138355622,0.441062780321708,3.78235614259331));
#57234=CARTESIAN_POINT('Ctrl Pts',(12.8274296716251,0.421610885427219,4.2532774884218));
#57235=CARTESIAN_POINT('Ctrl Pts',(12.8597252784638,0.146394963767536,4.4145887178469));
#57236=CARTESIAN_POINT('Ctrl Pts',(12.876115606615,0.00428438860018927,
4.4165543301878));
#57237=CARTESIAN_POINT('Ctrl Pts',(12.8766006560786,7.85109994958138E-5,
4.41654344863055));
#57238=CARTESIAN_POINT('Ctrl Pts',(12.6733993439214,-0.000382453243898042,
4.41589767499447));
#57239=CARTESIAN_POINT('Ctrl Pts',(12.6770138141737,-0.0318505807336982,
4.4161892599907));
#57240=CARTESIAN_POINT('Ctrl Pts',(12.6965335631136,-0.201468625965512,
4.39853963407534));
#57241=CARTESIAN_POINT('Ctrl Pts',(12.7319585907412,-0.462967872677167,
4.16603003860975));
#57242=CARTESIAN_POINT('Ctrl Pts',(12.779674426804,-0.390044463885,3.70038267566003));
#57243=CARTESIAN_POINT('Ctrl Pts',(12.8273902628668,0.0410627776982723,
3.50987851185683));
#57244=CARTESIAN_POINT('Ctrl Pts',(12.8751060989297,0.434461438689172,3.76946045210395));
#57245=CARTESIAN_POINT('Ctrl Pts',(12.9228219349925,0.42888747548329,4.24075040649094));
#57246=CARTESIAN_POINT('Ctrl Pts',(12.9555863499897,0.154617472482897,4.41255553662561));
#57247=CARTESIAN_POINT('Ctrl Pts',(12.9724454862994,0.00842423538524961,
4.41653398830136));
#57248=CARTESIAN_POINT('Ctrl Pts',(12.9733993439214,0.000150764780949724,
4.4164954541449));
#57249=CARTESIAN_POINT('Origin',(3.42660065607856,0.,4.));
#57250=CARTESIAN_POINT('',(12.2766006560786,9.99581421417901E-5,4.41520820259509));
#57251=CARTESIAN_POINT('',(12.3733993439214,3.32456539758885E-5,4.41518865831861));
#57252=CARTESIAN_POINT('',(3.42660065607856,4.87367679877478E-13,4.415875));
#57253=CARTESIAN_POINT('Ctrl Pts',(12.2766006560786,9.99581421418094E-5,
4.41520820259509));
#57254=CARTESIAN_POINT('Ctrl Pts',(12.2852522623637,-0.0755384113923865,
4.41504611816934));
#57255=CARTESIAN_POINT('Ctrl Pts',(12.3098091473364,-0.290455378639464,
4.35903266527152));
#57256=CARTESIAN_POINT('Ctrl Pts',(12.3502713109967,-0.49164800158875,4.0136918729824));
#57257=CARTESIAN_POINT('Ctrl Pts',(12.3979871470595,-0.277420602272412,
3.59386820576715));
#57258=CARTESIAN_POINT('Ctrl Pts',(12.4457029831224,0.191566404775332,3.54700161433684));
#57259=CARTESIAN_POINT('Ctrl Pts',(12.4934188191852,0.484635034689867,3.91613041073711));
#57260=CARTESIAN_POINT('Ctrl Pts',(12.5370513768373,0.345661459897227,4.32409890635003));
#57261=CARTESIAN_POINT('Ctrl Pts',(12.5647786558017,0.102620036091023,4.41484591908716));
#57262=CARTESIAN_POINT('Ctrl Pts',(12.5766006560786,-0.000382134531266193,
4.41577416496379));
#57263=CARTESIAN_POINT('Ctrl Pts',(12.3733993439214,3.32456539758746E-5,
4.41518865831861));
#57264=CARTESIAN_POINT('Ctrl Pts',(12.381582142048,-0.071514873974996,4.41513780400291));
#57265=CARTESIAN_POINT('Ctrl Pts',(12.4056702188623,-0.282203129244181,
4.36350051499509));
#57266=CARTESIAN_POINT('Ctrl Pts',(12.4456635743641,-0.491031474462283,
4.0281658647901));
#57267=CARTESIAN_POINT('Ctrl Pts',(12.493379410427,-0.289261580343189,3.60221492864948));
#57268=CARTESIAN_POINT('Ctrl Pts',(12.5410952464898,0.178141673866572,3.54155614424011));
#57269=CARTESIAN_POINT('Ctrl Pts',(12.5888110825527,0.481954687902679,3.90189340664049));
#57270=CARTESIAN_POINT('Ctrl Pts',(12.6329124483632,0.353693368040787,4.31820342736526));
#57271=CARTESIAN_POINT('Ctrl Pts',(12.6611085354861,0.106623193447456,4.41490615616012));
#57272=CARTESIAN_POINT('Ctrl Pts',(12.6733993439214,-0.000382453243898042,
4.41589767499447));
#57273=CARTESIAN_POINT('Origin',(3.42660065607856,0.,4.));
#57274=CARTESIAN_POINT('',(11.9766006560786,0.000344603143201134,4.41614202049347));
#57275=CARTESIAN_POINT('',(12.0733993439214,0.00037008249145147,4.41602009379307));
#57276=CARTESIAN_POINT('',(3.42660065607856,4.87367679877478E-13,4.415875));
#57277=CARTESIAN_POINT('Ctrl Pts',(11.9766006560786,0.000344603143201134,
4.41614202049347));
#57278=CARTESIAN_POINT('Ctrl Pts',(11.989820590238,-0.114576335025177,4.41511745277426));
#57279=CARTESIAN_POINT('Ctrl Pts',(12.018945803085,-0.369470719226983,4.30593844396252));
#57280=CARTESIAN_POINT('Ctrl Pts',(12.0639762946196,-0.475409571231627,
3.87394063131468));
#57281=CARTESIAN_POINT('Ctrl Pts',(12.1116921306825,-0.151090047408964,
3.53194335553704));
#57282=CARTESIAN_POINT('Ctrl Pts',(12.1594079667453,0.311977791768556,3.61976969834691));
#57283=CARTESIAN_POINT('Ctrl Pts',(12.2071238028081,0.488551624369653,4.05676737776005));
#57284=CARTESIAN_POINT('Ctrl Pts',(12.2461880325859,0.265811525316043,4.37185240566124));
#57285=CARTESIAN_POINT('Ctrl Pts',(12.269346983676,0.0635166157645696,4.41534409728183));
#57286=CARTESIAN_POINT('Ctrl Pts',(12.2766006560786,9.99581421418094E-5,
4.41520820259509));
#57287=CARTESIAN_POINT('Ctrl Pts',(12.0733993439214,0.000370082491451453,
4.41602009379308));
#57288=CARTESIAN_POINT('Ctrl Pts',(12.0861504699224,-0.110559366248508,
4.41499479059613));
#57289=CARTESIAN_POINT('Ctrl Pts',(12.1148068746109,-0.361534897467509,
4.3122242613332));
#57290=CARTESIAN_POINT('Ctrl Pts',(12.1593685579871,-0.478916017555994,
3.88799699566402));
#57291=CARTESIAN_POINT('Ctrl Pts',(12.2070843940499,-0.164809627468288,
3.53659627586117));
#57292=CARTESIAN_POINT('Ctrl Pts',(12.2548002301128,0.300643979445627,3.61074632631782));
#57293=CARTESIAN_POINT('Ctrl Pts',(12.3025160661756,0.490011594032383,4.04235401475446));
#57294=CARTESIAN_POINT('Ctrl Pts',(12.3420491041118,0.274087380788525,4.36772087084377));
#57295=CARTESIAN_POINT('Ctrl Pts',(12.3656768633604,0.0675564760281007,
4.41523665186048));
#57296=CARTESIAN_POINT('Ctrl Pts',(12.3733993439214,3.32456539758746E-5,
4.41518865831861));
#57297=CARTESIAN_POINT('Origin',(3.42660065607856,0.,4.));
#57298=CARTESIAN_POINT('',(11.6766006560786,-0.000272404999166542,4.41633191892761));
#57299=CARTESIAN_POINT('',(11.7733993439214,-0.000215373091504267,4.41642415578018));
#57300=CARTESIAN_POINT('',(3.42660065607856,4.87367679877478E-13,4.415875));
#57301=CARTESIAN_POINT('Ctrl Pts',(11.6766006560786,-0.000272404999166455,
4.41633191892761));
#57302=CARTESIAN_POINT('Ctrl Pts',(11.6784836394247,-0.0166217551361539,
4.41645573239506));
#57303=CARTESIAN_POINT('Ctrl Pts',(11.6962719014584,-0.170944672110958,
4.40814899119985));
#57304=CARTESIAN_POINT('Ctrl Pts',(11.7299654421798,-0.44220355512924,4.21531660568344));
#57305=CARTESIAN_POINT('Ctrl Pts',(11.7776812782426,-0.420270357404582,
3.74450430230823));
#57306=CARTESIAN_POINT('Ctrl Pts',(11.8253971143054,-0.0123964237846327,
3.50831762943));
#57307=CARTESIAN_POINT('Ctrl Pts',(11.8731129503683,0.406861336540243,3.72365044295193));
#57308=CARTESIAN_POINT('Ctrl Pts',(11.9208287864311,0.452492071153857,4.1927593068956));
#57309=CARTESIAN_POINT('Ctrl Pts',(11.9553246883346,0.185075114683736,4.40392780377));
#57310=CARTESIAN_POINT('Ctrl Pts',(11.9739153115504,0.0236883133891,4.41635013933017));
#57311=CARTESIAN_POINT('Ctrl Pts',(11.9766006560786,0.000344603143201134,
4.41614202049347));
#57312=CARTESIAN_POINT('Ctrl Pts',(11.7733993439214,-0.000215373091504231,
4.41642415578018));
#57313=CARTESIAN_POINT('Ctrl Pts',(11.7748135191091,-0.0124870613922979,
4.41650138834433));
#57314=CARTESIAN_POINT('Ctrl Pts',(11.7921329729843,-0.162701432614141,
4.41043584391465));
#57315=CARTESIAN_POINT('Ctrl Pts',(11.8253577055472,-0.435670260442099,
4.22824690363353));
#57316=CARTESIAN_POINT('Ctrl Pts',(11.8730735416101,-0.427612859293677,
3.75699286549843));
#57317=CARTESIAN_POINT('Ctrl Pts',(11.9207893776729,-0.0268719897862959,
3.50889601812151));
#57318=CARTESIAN_POINT('Ctrl Pts',(11.9685052137357,0.398545841420554,3.71178751390968));
#57319=CARTESIAN_POINT('Ctrl Pts',(12.0162210497986,0.457972894034889,4.17934897039372));
#57320=CARTESIAN_POINT('Ctrl Pts',(12.0511857598605,0.193343073938706,4.40127740506484));
#57321=CARTESIAN_POINT('Ctrl Pts',(12.0702451912347,0.0278098881012828,
4.41627371553856));
#57322=CARTESIAN_POINT('Ctrl Pts',(12.0733993439214,0.000370082491451453,
4.41602009379308));
#57323=CARTESIAN_POINT('Origin',(3.42660065607856,0.,4.));
#57324=CARTESIAN_POINT('',(11.3766006560786,-0.000206048103233091,4.41528588740701));
#57325=CARTESIAN_POINT('',(11.4733993439214,-0.000260100423148973,4.41535533657191));
#57326=CARTESIAN_POINT('',(3.42660065607856,4.87367679877478E-13,4.415875));
#57327=CARTESIAN_POINT('Ctrl Pts',(11.3766006560786,-0.000206048103232999,
4.41528588740701));
#57328=CARTESIAN_POINT('Ctrl Pts',(11.383051967299,-0.0565815589273492,
4.41553770218085));
#57329=CARTESIAN_POINT('Ctrl Pts',(11.4054085572071,-0.251630532720247,
4.37854193442951));
#57330=CARTESIAN_POINT('Ctrl Pts',(11.4436704258028,-0.485070265991237,
4.08131458604192));
#57331=CARTESIAN_POINT('Ctrl Pts',(11.4913862618656,-0.330742172127369,
3.63597412121053));
#57332=CARTESIAN_POINT('Ctrl Pts',(11.5391020979284,0.127311547523522,3.52492422212962));
#57333=CARTESIAN_POINT('Ctrl Pts',(11.5868179339912,0.468453114143607,3.85014371984754));
#57334=CARTESIAN_POINT('Ctrl Pts',(11.632650786708,0.382920955827079,4.29471395365306));
#57335=CARTESIAN_POINT('Ctrl Pts',(11.6625783607371,0.121478760105588,4.41540989855421));
#57336=CARTESIAN_POINT('Ctrl Pts',(11.6766006560786,-0.000272404999166455,
4.41633191892761));
#57337=CARTESIAN_POINT('Ctrl Pts',(11.4733993439214,-0.000260100423148869,
4.41535533657191));
#57338=CARTESIAN_POINT('Ctrl Pts',(11.4793818469834,-0.0525169974224216,
4.41565306322741));
#57339=CARTESIAN_POINT('Ctrl Pts',(11.501269628733,-0.243338890257842,4.3822327073369));
#57340=CARTESIAN_POINT('Ctrl Pts',(11.5390626891702,-0.482464979911041,
4.09556551685319));
#57341=CARTESIAN_POINT('Ctrl Pts',(11.586778525233,-0.341319923258817,3.64587299617429));
#57342=CARTESIAN_POINT('Ctrl Pts',(11.6344943612959,0.113264470804062,3.5213807520529));
#57343=CARTESIAN_POINT('Ctrl Pts',(11.6822101973587,0.463836358529674,3.83641192782507));
#57344=CARTESIAN_POINT('Ctrl Pts',(11.7285118582339,0.390694138047139,4.28787953265104));
#57345=CARTESIAN_POINT('Ctrl Pts',(11.7589082404215,0.125533053862222,4.41563275094549));
#57346=CARTESIAN_POINT('Ctrl Pts',(11.7733993439214,-0.000215373091504231,
4.41642415578018));
#57347=CARTESIAN_POINT('Origin',(3.42660065607856,0.,4.));
#57348=CARTESIAN_POINT('',(11.0766006560786,0.000352537510456688,4.41557576695298));
#57349=CARTESIAN_POINT('',(11.1733993439214,0.000319650745578964,4.41547275084625));
#57350=CARTESIAN_POINT('',(3.42660065607856,4.87367679877478E-13,4.415875));
#57351=CARTESIAN_POINT('Ctrl Pts',(11.0766006560786,0.000352537510456667,
4.41557576695298));
#57352=CARTESIAN_POINT('Ctrl Pts',(11.0876202951733,-0.0957751134661499,
4.41480617263661));
#57353=CARTESIAN_POINT('Ctrl Pts',(11.1145452129557,-0.331820540820521,
4.33374203885914));
#57354=CARTESIAN_POINT('Ctrl Pts',(11.1573754094257,-0.488245699001722,
3.94065893278431));
#57355=CARTESIAN_POINT('Ctrl Pts',(11.2050912454886,-0.214150733603143,
3.55723066033293));
#57356=CARTESIAN_POINT('Ctrl Pts',(11.2528070815514,0.256602145595791,3.58040428537983));
#57357=CARTESIAN_POINT('Ctrl Pts',(11.3005229176142,0.491713326162588,3.98889911147238));
#57358=CARTESIAN_POINT('Ctrl Pts',(11.3417874424566,0.304539430122629,4.35098016691413));
#57359=CARTESIAN_POINT('Ctrl Pts',(11.3671466886114,0.0824085130402235,
4.41491686960609));
#57360=CARTESIAN_POINT('Ctrl Pts',(11.3766006560786,-0.000206048103232999,
4.41528588740701));
#57361=CARTESIAN_POINT('Ctrl Pts',(11.1733993439214,0.000319650745578978,
4.41547275084625));
#57362=CARTESIAN_POINT('Ctrl Pts',(11.1839501748577,-0.0917759901056567,
4.4148158243975));
#57363=CARTESIAN_POINT('Ctrl Pts',(11.2104062844816,-0.32368545017211,4.33911969104981));
#57364=CARTESIAN_POINT('Ctrl Pts',(11.2527676727932,-0.489781601228288,
3.95506440219344));
#57365=CARTESIAN_POINT('Ctrl Pts',(11.300483508856,-0.227098200695192,3.56372986339542));
#57366=CARTESIAN_POINT('Ctrl Pts',(11.3481993449188,0.244132971891272,3.57302890392028));
#57367=CARTESIAN_POINT('Ctrl Pts',(11.3959151809817,0.491173079921361,3.97442207176994));
#57368=CARTESIAN_POINT('Ctrl Pts',(11.4376485139825,0.312739912806573,4.34603313379779));
#57369=CARTESIAN_POINT('Ctrl Pts',(11.4634765682958,0.0864149014017155,
4.41486151738456));
#57370=CARTESIAN_POINT('Ctrl Pts',(11.4733993439214,-0.000260100423148869,
4.41535533657191));
#57371=CARTESIAN_POINT('Origin',(3.42660065607856,0.,4.));
#57372=CARTESIAN_POINT('',(10.7766006560786,5.16128798610187E-5,4.41655360457584));
#57373=CARTESIAN_POINT('',(10.8733993439214,0.000125523266313186,4.41651574507477));
#57374=CARTESIAN_POINT('',(3.42660065607856,4.87367679877478E-13,4.415875));
#57375=CARTESIAN_POINT('Ctrl Pts',(10.7766006560786,5.16128798610299E-5,
4.41655360457584));
#57376=CARTESIAN_POINT('Ctrl Pts',(10.7921886230477,-0.135103241057852,
4.41631783152902));
#57377=CARTESIAN_POINT('Ctrl Pts',(10.8236818687044,-0.408598944994929,
4.27108057505162));
#57378=CARTESIAN_POINT('Ctrl Pts',(10.8710803930487,-0.451470021714238,
3.80485891169382));
#57379=CARTESIAN_POINT('Ctrl Pts',(10.9187962291115,-0.080036233235122,
3.51471716883706));
#57380=CARTESIAN_POINT('Ctrl Pts',(10.9665120651743,0.364896059739551,3.6702181168734));
#57381=CARTESIAN_POINT('Ctrl Pts',(11.0142279012372,0.47473868640782,4.1285628425314));
#57382=CARTESIAN_POINT('Ctrl Pts',(11.0509240982053,0.223935965514619,4.3902602363912));
#57383=CARTESIAN_POINT('Ctrl Pts',(11.0717150164857,0.0429714521173939,
4.4159169723618));
#57384=CARTESIAN_POINT('Ctrl Pts',(11.0766006560786,0.000352537510456667,
4.41557576695298));
#57385=CARTESIAN_POINT('Ctrl Pts',(10.8733993439214,0.000125523266313226,
4.41651574507477));
#57386=CARTESIAN_POINT('Ctrl Pts',(10.888518502732,-0.130996444363694,4.41599591363288));
#57387=CARTESIAN_POINT('Ctrl Pts',(10.9195429402303,-0.400997532511054,
4.27840016053723));
#57388=CARTESIAN_POINT('Ctrl Pts',(10.9664726564161,-0.45702143577077,3.81824018018824));
#57389=CARTESIAN_POINT('Ctrl Pts',(11.014188492479,-0.0942939790271268,
3.51728489730359));
#57390=CARTESIAN_POINT('Ctrl Pts',(11.0619043285418,0.355025089556487,3.65961432075161));
#57391=CARTESIAN_POINT('Ctrl Pts',(11.1096201646047,0.478319155637209,4.11452515096033));
#57392=CARTESIAN_POINT('Ctrl Pts',(11.1467851697312,0.23222845252417,4.38693182090163));
#57393=CARTESIAN_POINT('Ctrl Pts',(11.1680448961701,0.0470573247768451,
4.41580613485813));
#57394=CARTESIAN_POINT('Ctrl Pts',(11.1733993439214,0.000319650745578978,
4.41547275084625));
#57395=CARTESIAN_POINT('Origin',(3.42660065607856,0.,4.));
#57396=CARTESIAN_POINT('',(10.4766006560786,-0.000378910032885682,4.4157309619862));
#57397=CARTESIAN_POINT('',(10.5733993439214,-0.000383826598418624,4.41585315377736));
#57398=CARTESIAN_POINT('',(3.42660065607856,4.87367679877478E-13,4.415875));
#57399=CARTESIAN_POINT('Ctrl Pts',(10.4766006560786,-0.000378910032885704,
4.4157309619862));
#57400=CARTESIAN_POINT('Ctrl Pts',(10.4808516722344,-0.0374267536145521,
4.41605913507464));
#57401=CARTESIAN_POINT('Ctrl Pts',(10.5010079670778,-0.212714974368116,
4.3945277200383));
#57402=CARTESIAN_POINT('Ctrl Pts',(10.5370695406088,-0.469236294399976,
4.14738563318641));
#57403=CARTESIAN_POINT('Ctrl Pts',(10.5847853766716,-0.377752434501872,
3.68502647241413));
#57404=CARTESIAN_POINT('Ctrl Pts',(10.6325012127345,0.0606272984676223,
3.51191234851464));
#57405=CARTESIAN_POINT('Ctrl Pts',(10.6802170487973,0.443332050383407,3.78701662516801));
#57406=CARTESIAN_POINT('Ctrl Pts',(10.7279328848602,0.418918158891686,4.25770681210006));
#57407=CARTESIAN_POINT('Ctrl Pts',(10.7600607539539,0.143455624352724,4.41528584951654));
#57408=CARTESIAN_POINT('Ctrl Pts',(10.7762833443601,0.00280285164340033,
4.41655840401831));
#57409=CARTESIAN_POINT('Ctrl Pts',(10.7766006560786,5.16128798610299E-5,
4.41655360457584));
#57410=CARTESIAN_POINT('Ctrl Pts',(10.5733993439214,-0.000383826598418617,
4.41585315377736));
#57411=CARTESIAN_POINT('Ctrl Pts',(10.5771815519187,-0.0333213161677604,
4.41615637378185));
#57412=CARTESIAN_POINT('Ctrl Pts',(10.5968690386037,-0.20443114816448,4.39750812937281));
#57413=CARTESIAN_POINT('Ctrl Pts',(10.6324618039763,-0.464691964107356,
4.16114156306187));
#57414=CARTESIAN_POINT('Ctrl Pts',(10.6801776400391,-0.386865111317189,
3.69628860657276));
#57415=CARTESIAN_POINT('Ctrl Pts',(10.7278934761019,0.0462259258804368,
3.51033849586834));
#57416=CARTESIAN_POINT('Ctrl Pts',(10.7756093121648,0.436866984064762,3.77405207881873));
#57417=CARTESIAN_POINT('Ctrl Pts',(10.8233251482276,0.426326368719826,4.24525711444552));
#57418=CARTESIAN_POINT('Ctrl Pts',(10.8559218254798,0.151674250044741,4.4132974389186));
#57419=CARTESIAN_POINT('Ctrl Pts',(10.8726132240444,0.00694320316194716,
4.41654277368359));
#57420=CARTESIAN_POINT('Ctrl Pts',(10.8733993439214,0.000125523266313226,
4.41651574507477));
#57421=CARTESIAN_POINT('Origin',(3.42660065607856,0.,4.));
#57422=CARTESIAN_POINT('',(10.1766006560786,0.000123197149224082,4.41521991402453));
#57423=CARTESIAN_POINT('',(10.2733993439214,5.7336166378985E-5,4.41519339896199));
#57424=CARTESIAN_POINT('',(3.42660065607856,4.87367679877478E-13,4.415875));
#57425=CARTESIAN_POINT('Ctrl Pts',(10.1766006560786,0.000123197149224097,
4.41521991402453));
#57426=CARTESIAN_POINT('Ctrl Pts',(10.1854200001087,-0.0769762270984491,
4.41501595190525));
#57427=CARTESIAN_POINT('Ctrl Pts',(10.2101446228264,-0.293404201931947,
4.35739193013711));
#57428=CARTESIAN_POINT('Ctrl Pts',(10.2507745242318,-0.491764996345908,
4.00850959581219));
#57429=CARTESIAN_POINT('Ctrl Pts',(10.2984903602946,-0.273124940234581,
3.59096700393021));
#57430=CARTESIAN_POINT('Ctrl Pts',(10.3462061963575,0.196329951061554,3.54904570612073));
#57431=CARTESIAN_POINT('Ctrl Pts',(10.3939220324203,0.485492027373267,3.92124267520431));
#57432=CARTESIAN_POINT('Ctrl Pts',(10.4373868523273,0.34277731801193,4.32616121393696));
#57433=CARTESIAN_POINT('Ctrl Pts',(10.4649463935468,0.101188639822117,4.41483126760997));
#57434=CARTESIAN_POINT('Ctrl Pts',(10.4766006560786,-0.000378910032885704,
4.4157309619862));
#57435=CARTESIAN_POINT('Ctrl Pts',(10.2733993439214,5.73361663789851E-5,
4.41519339896199));
#57436=CARTESIAN_POINT('Ctrl Pts',(10.2817498797931,-0.0729553575157724,
4.41510384014646));
#57437=CARTESIAN_POINT('Ctrl Pts',(10.3060056943524,-0.285157432566911,
4.36192175935665));
#57438=CARTESIAN_POINT('Ctrl Pts',(10.3461667875993,-0.491301045992024,
4.02298928139638));
#57439=CARTESIAN_POINT('Ctrl Pts',(10.3938826236621,-0.285053227451061,
3.599188470261));
#57440=CARTESIAN_POINT('Ctrl Pts',(10.4415984597249,0.182963355965895,3.54345905416307));
#57441=CARTESIAN_POINT('Ctrl Pts',(10.4893142957878,0.482961874346273,3.9069782134126));
#57442=CARTESIAN_POINT('Ctrl Pts',(10.5332479238533,0.35082465130295,4.32033516829581));
#57443=CARTESIAN_POINT('Ctrl Pts',(10.5612762732311,0.105190355120073,4.41488124595214));
#57444=CARTESIAN_POINT('Ctrl Pts',(10.5733993439214,-0.000383826598418617,
4.41585315377736));
#57445=CARTESIAN_POINT('Origin',(3.42660065607856,0.,4.));
#57446=CARTESIAN_POINT('',(9.87660065607859,0.000332404019580576,4.41618417038907));
#57447=CARTESIAN_POINT('',(9.9733993439214,0.000362444897862246,4.41606425076498));
#57448=CARTESIAN_POINT('',(3.42660065607856,4.87367679877478E-13,4.415875));
#57449=CARTESIAN_POINT('Ctrl Pts',(9.87660065607859,0.000332404019580564,
4.41618417038907));
#57450=CARTESIAN_POINT('Ctrl Pts',(9.88998832798303,-0.116016130490024,
4.41516972706101));
#57451=CARTESIAN_POINT('Ctrl Pts',(9.91928127857509,-0.372296869871387,
4.30364082544554));
#57452=CARTESIAN_POINT('Ctrl Pts',(9.96447950785476,-0.474054618562381,
3.8689372536849));
#57453=CARTESIAN_POINT('Ctrl Pts',(10.0121953439176,-0.146148770628728,
3.53037700046135));
#57454=CARTESIAN_POINT('Ctrl Pts',(10.0599111799804,0.315967742161179,3.62307877379278));
#57455=CARTESIAN_POINT('Ctrl Pts',(10.1076270160433,0.487926215535836,4.06191310882887));
#57456=CARTESIAN_POINT('Ctrl Pts',(10.146523508076,0.262848409674369,4.37329037489646));
#57457=CARTESIAN_POINT('Ctrl Pts',(10.1695147214211,0.062069015396409,4.41538378814543));
#57458=CARTESIAN_POINT('Ctrl Pts',(10.1766006560786,0.000123197149224097,
4.41521991402453));
#57459=CARTESIAN_POINT('Ctrl Pts',(9.9733993439214,0.000362444897862267,
4.41606425076498));
#57460=CARTESIAN_POINT('Ctrl Pts',(9.9863182076674,-0.111995531308361,4.41503480155798));
#57461=CARTESIAN_POINT('Ctrl Pts',(10.015142350101,-0.364380386131072,4.30999810797653));
#57462=CARTESIAN_POINT('Ctrl Pts',(10.0598717712222,-0.477709011270712,
3.88295588266498));
#57463=CARTESIAN_POINT('Ctrl Pts',(10.1075876072851,-0.159916626226494,
3.53488507064564));
#57464=CARTESIAN_POINT('Ctrl Pts',(10.1553034433479,0.304729657315094,3.61393645496551));
#57465=CARTESIAN_POINT('Ctrl Pts',(10.2030192794107,0.489538007675758,4.04751593304174));
#57466=CARTESIAN_POINT('Ctrl Pts',(10.2423845796019,0.271127379494919,4.3692182851415));
#57467=CARTESIAN_POINT('Ctrl Pts',(10.2658446011055,0.0661120339180705,
4.41527442296197));
#57468=CARTESIAN_POINT('Ctrl Pts',(10.2733993439214,5.73361663789851E-5,
4.41519339896199));
#57469=CARTESIAN_POINT('Origin',(3.42660065607856,0.,4.));
#57470=CARTESIAN_POINT('',(9.57660065607859,-0.000290304052950346,4.41629504206998));
#57471=CARTESIAN_POINT('',(9.6733993439214,-0.000236899196693507,4.41639317328699));
#57472=CARTESIAN_POINT('',(3.42660065607856,4.87367679877478E-13,4.415875));
#57473=CARTESIAN_POINT('Ctrl Pts',(9.57660065607859,-0.000290304052950335,
4.41629504206998));
#57474=CARTESIAN_POINT('Ctrl Pts',(9.57865137716975,-0.0181001948149981,
4.41643644713422));
#57475=CARTESIAN_POINT('Ctrl Pts',(9.59660737694851,-0.173896467062472,
4.40729888742394));
#57476=CARTESIAN_POINT('Ctrl Pts',(9.63046865541489,-0.444448234747017,
4.21064422964382));
#57477=CARTESIAN_POINT('Ctrl Pts',(9.67818449147773,-0.41755432743774,3.74008922975375));
#57478=CARTESIAN_POINT('Ctrl Pts',(9.72590032754057,-0.00721385634321597,
3.50821428942208));
#57479=CARTESIAN_POINT('Ctrl Pts',(9.77361616360341,0.40975121003073,3.72795373420991));
#57480=CARTESIAN_POINT('Ctrl Pts',(9.82133199966624,0.450435435400681,4.19751745084266));
#57481=CARTESIAN_POINT('Ctrl Pts',(9.85566016382464,0.182118884769847,4.40484283743537));
#57482=CARTESIAN_POINT('Ctrl Pts',(9.87408304929542,0.0222122246324328,
4.41637494063069));
#57483=CARTESIAN_POINT('Ctrl Pts',(9.87660065607859,0.000332404019580564,
4.41618417038907));
#57484=CARTESIAN_POINT('Ctrl Pts',(9.6733993439214,-0.00023689919669354,
4.41639317328699));
#57485=CARTESIAN_POINT('Ctrl Pts',(9.67498125685411,-0.0139668454918635,
4.4164864708936));
#57486=CARTESIAN_POINT('Ctrl Pts',(9.69246844847443,-0.165649677201134,
4.40963259460397));
#57487=CARTESIAN_POINT('Ctrl Pts',(9.72586091878235,-0.438051576325333,
4.22364266437974));
#57488=CARTESIAN_POINT('Ctrl Pts',(9.77357675484519,-0.425028039486299,
3.75249971615691));
#57489=CARTESIAN_POINT('Ctrl Pts',(9.82129259090803,-0.0216947140899849,
3.50864008686857));
#57490=CARTESIAN_POINT('Ctrl Pts',(9.86900842697087,0.401561201071248,3.7160038263529));
#57491=CARTESIAN_POINT('Ctrl Pts',(9.91672426303371,0.456057286475463,4.18416562194019));
#57492=CARTESIAN_POINT('Ctrl Pts',(9.95152123535055,0.190383912560376,4.40224154849284));
#57493=CARTESIAN_POINT('Ctrl Pts',(9.97041292897978,0.0263359008882403,
4.4163022254471));
#57494=CARTESIAN_POINT('Ctrl Pts',(9.9733993439214,0.000362444897862267,
4.41606425076498));
#57495=CARTESIAN_POINT('Origin',(3.42660065607856,0.,4.));
#57496=CARTESIAN_POINT('',(9.27660065607858,-0.000185084181660103,4.41526520375254));
#57497=CARTESIAN_POINT('',(9.37339934392141,-0.000241596553487405,4.41532857883968));
#57498=CARTESIAN_POINT('',(3.42660065607856,4.87367679877478E-13,4.415875));
#57499=CARTESIAN_POINT('Ctrl Pts',(9.27660065607858,-0.000185084181660189,
4.41526520375254));
#57500=CARTESIAN_POINT('Ctrl Pts',(9.28321970504406,-0.0580335922681754,
4.4154966095816));
#57501=CARTESIAN_POINT('Ctrl Pts',(9.30574403269715,-0.254596444523232,
4.37718269734299));
#57502=CARTESIAN_POINT('Ctrl Pts',(9.34417363903789,-0.485900307124067,
4.07619787653679));
#57503=CARTESIAN_POINT('Ctrl Pts',(9.39188947510068,-0.326887306273347,
3.63250862071426));
#57504=CARTESIAN_POINT('Ctrl Pts',(9.43960531116356,0.13231133773591,3.52629235307153));
#57505=CARTESIAN_POINT('Ctrl Pts',(9.48732114722637,0.470006444430667,3.85508910653225));
#57506=CARTESIAN_POINT('Ctrl Pts',(9.53298626219807,0.380123833963086,4.29710958399465));
#57507=CARTESIAN_POINT('Ctrl Pts',(9.56274609848214,0.120032327051623,4.41533971732329));
#57508=CARTESIAN_POINT('Ctrl Pts',(9.57660065607859,-0.000290304052950335,
4.41629504206998));
#57509=CARTESIAN_POINT('Ctrl Pts',(9.3733993439214,-0.000241596553487357,
4.41532857883968));
#57510=CARTESIAN_POINT('Ctrl Pts',(9.37954958472843,-0.0539723465869793,
4.41561177485228));
#57511=CARTESIAN_POINT('Ctrl Pts',(9.40160510422307,-0.246305905820531,
4.3809303471886));
#57512=CARTESIAN_POINT('Ctrl Pts',(9.43956590240532,-0.483445357410111,
4.09047547319903));
#57513=CARTESIAN_POINT('Ctrl Pts',(9.48728173846818,-0.337568794959357,
3.64229546617122));
#57514=CARTESIAN_POINT('Ctrl Pts',(9.53499757453099,0.118302386066128,3.5226010365501));
#57515=CARTESIAN_POINT('Ctrl Pts',(9.58271341059386,0.465534665650901,3.84130942079228));
#57516=CARTESIAN_POINT('Ctrl Pts',(9.62884733372396,0.387920650713885,4.29034844530944));
#57517=CARTESIAN_POINT('Ctrl Pts',(9.65907597816649,0.124080336294106,4.41554841393524));
#57518=CARTESIAN_POINT('Ctrl Pts',(9.6733993439214,-0.00023689919669354,
4.41639317328699));
#57519=CARTESIAN_POINT('Origin',(3.42660065607856,0.,4.));
#57520=CARTESIAN_POINT('',(8.97660065607858,0.000361621133123973,4.41561526113518));
#57521=CARTESIAN_POINT('',(9.0733993439214,0.00033264130393823,4.41550825894961));
#57522=CARTESIAN_POINT('',(3.42660065607856,4.87367679877478E-13,4.415875));
#57523=CARTESIAN_POINT('Ctrl Pts',(8.97660065607858,0.000361621133123963,
4.41561526113518));
#57524=CARTESIAN_POINT('Ctrl Pts',(8.98778803291839,-0.097205817696177,
4.41480833810253));
#57525=CARTESIAN_POINT('Ctrl Pts',(9.01488068844582,-0.334723089553266,
4.33177224018802));
#57526=CARTESIAN_POINT('Ctrl Pts',(9.05787862266083,-0.487593182843731,
3.93551656882348));
#57527=CARTESIAN_POINT('Ctrl Pts',(9.10559445872368,-0.209472459465777,
3.55499829935456));
#57528=CARTESIAN_POINT('Ctrl Pts',(9.15331029478651,0.261010046587687,3.58313193881964));
#57529=CARTESIAN_POINT('Ctrl Pts',(9.20102613084934,0.491803010703882,3.99408193320625));
#57530=CARTESIAN_POINT('Ctrl Pts',(9.24212291794672,0.301599829163518,4.35270650246492));
#57531=CARTESIAN_POINT('Ctrl Pts',(9.26731442635645,0.0809737859182142,
4.41494055172187));
#57532=CARTESIAN_POINT('Ctrl Pts',(9.27660065607858,-0.000185084181660189,
4.41526520375254));
#57533=CARTESIAN_POINT('Ctrl Pts',(9.0733993439214,0.000332641303938268,
4.41550825894961));
#57534=CARTESIAN_POINT('Ctrl Pts',(9.08411791260276,-0.093207009794584,
4.4148098083896));
#57535=CARTESIAN_POINT('Ctrl Pts',(9.11074175997173,-0.326599857706223,
4.33721709571948));
#57536=CARTESIAN_POINT('Ctrl Pts',(9.1532708860283,-0.489280820139143,3.94990505119329));
#57537=CARTESIAN_POINT('Ctrl Pts',(9.20098672209113,-0.222487703095825,
3.56136068709803));
#57538=CARTESIAN_POINT('Ctrl Pts',(9.24870255815399,0.248619295113741,3.57562555337399));
#57539=CARTESIAN_POINT('Ctrl Pts',(9.29641839421681,0.49141536912078,3.97960000382683));
#57540=CARTESIAN_POINT('Ctrl Pts',(9.33798398947263,0.309808547095179,4.34782394055348));
#57541=CARTESIAN_POINT('Ctrl Pts',(9.36364430604082,0.0849819773478622,
4.41487939515448));
#57542=CARTESIAN_POINT('Ctrl Pts',(9.3733993439214,-0.000241596553487357,
4.41532857883968));
#57543=CARTESIAN_POINT('Origin',(3.42660065607856,0.,4.));
#57544=CARTESIAN_POINT('',(8.67660065607859,2.43999233753954E-5,4.41655967853978));
#57545=CARTESIAN_POINT('',(8.77339934392141,9.9565801791445E-5,4.41653262406943));
#57546=CARTESIAN_POINT('',(3.42660065607856,4.87367679877478E-13,4.415875));
#57547=CARTESIAN_POINT('Ctrl Pts',(8.67660065607859,2.43999233753836E-5,
4.41655967853978));
#57548=CARTESIAN_POINT('Ctrl Pts',(8.69235636079272,-0.136579453435425,
4.41644398151286));
#57549=CARTESIAN_POINT('Ctrl Pts',(8.72401734419445,-0.411298873006737,
4.26841067400337));
#57550=CARTESIAN_POINT('Ctrl Pts',(8.7715836062838,-0.449388340942622,3.80011167148426));
#57551=CARTESIAN_POINT('Ctrl Pts',(8.81929944234665,-0.0749173544856965,
3.51390061216986));
#57552=CARTESIAN_POINT('Ctrl Pts',(8.86701527840948,0.368351391347115,3.67408210030036));
#57553=CARTESIAN_POINT('Ctrl Pts',(8.91473111447233,0.473357386691186,4.13355901061654));
#57554=CARTESIAN_POINT('Ctrl Pts',(8.95125957369535,0.220969504140389,4.39141457480799));
#57555=CARTESIAN_POINT('Ctrl Pts',(8.97188275423077,0.0415074238114615,
4.41595555392421));
#57556=CARTESIAN_POINT('Ctrl Pts',(8.97660065607858,0.000361621133123963,
4.41561526113518));
#57557=CARTESIAN_POINT('Ctrl Pts',(8.77339934392141,9.95658017914599E-5,
4.41653262406943));
#57558=CARTESIAN_POINT('Ctrl Pts',(8.78868624047708,-0.132462770989084,
4.416105976883));
#57559=CARTESIAN_POINT('Ctrl Pts',(8.81987841572037,-0.403726445587972,
4.27580529254432));
#57560=CARTESIAN_POINT('Ctrl Pts',(8.86697586965126,-0.455080472922433,
3.81343369002772));
#57561=CARTESIAN_POINT('Ctrl Pts',(8.91469170571412,-0.0892013699275644,
3.51631793453238));
#57562=CARTESIAN_POINT('Ctrl Pts',(8.96240754177693,0.358592723611288,3.66337486216116));
#57563=CARTESIAN_POINT('Ctrl Pts',(9.0101233778398,0.477085601399612,4.11955983351088));
#57564=CARTESIAN_POINT('Ctrl Pts',(9.04712064522126,0.229261233371815,4.38814011953822));
#57565=CARTESIAN_POINT('Ctrl Pts',(9.06821263391514,0.0455964315317218,
4.41584623882512));
#57566=CARTESIAN_POINT('Ctrl Pts',(9.0733993439214,0.000332641303938268,
4.41550825894961));
#57567=CARTESIAN_POINT('Origin',(3.42660065607856,0.,4.));
#57568=CARTESIAN_POINT('',(8.37660065607859,-0.000374086211409503,4.41568853448753));
#57569=CARTESIAN_POINT('',(8.47339934392141,-0.000383538171196851,4.41580895574666));
#57570=CARTESIAN_POINT('',(3.42660065607856,4.87367679877478E-13,4.415875));
#57571=CARTESIAN_POINT('Ctrl Pts',(8.37660065607859,-0.000374086211409545,
4.41568853448753));
#57572=CARTESIAN_POINT('Ctrl Pts',(8.38101940997943,-0.0388937529272332,
4.41602262289185));
#57573=CARTESIAN_POINT('Ctrl Pts',(8.40134344256788,-0.215680110827853,
4.3934260635833));
#57574=CARTESIAN_POINT('Ctrl Pts',(8.43757275384394,-0.470763542849379,
4.14243212971755));
#57575=CARTESIAN_POINT('Ctrl Pts',(8.48528858990678,-0.37441192437669,3.68106280283335));
#57576=CARTESIAN_POINT('Ctrl Pts',(8.53300442596962,0.0657679253190804,
3.51257841158684));
#57577=CARTESIAN_POINT('Ctrl Pts',(8.58072026203246,0.445552077224736,3.79170076492532));
#57578=CARTESIAN_POINT('Ctrl Pts',(8.62843609809529,0.41617890091499,4.26210751092856));
#57579=CARTESIAN_POINT('Ctrl Pts',(8.66039622944401,0.140517691799823,4.41596716726027));
#57580=CARTESIAN_POINT('Ctrl Pts',(8.6764510821051,0.00132122424898086,
4.41656077688887));
#57581=CARTESIAN_POINT('Ctrl Pts',(8.67660065607859,2.43999233753836E-5,
4.41655967853978));
#57582=CARTESIAN_POINT('Ctrl Pts',(8.47339934392141,-0.000383538171196768,
4.41580895574666));
#57583=CARTESIAN_POINT('Ctrl Pts',(8.47734928966379,-0.0347911067166248,
4.41612244784963));
#57584=CARTESIAN_POINT('Ctrl Pts',(8.4972045140938,-0.207394442561863,4.39645832432586));
#57585=CARTESIAN_POINT('Ctrl Pts',(8.5329650172114,-0.466364439759318,4.15623518867385));
#57586=CARTESIAN_POINT('Ctrl Pts',(8.58068085327425,-0.383642787608637,
3.69222827230584));
#57587=CARTESIAN_POINT('Ctrl Pts',(8.62839668933707,0.0513839395061145,
3.51085286915611));
#57588=CARTESIAN_POINT('Ctrl Pts',(8.67611252539993,0.439224004328866,3.77866880275638));
#57589=CARTESIAN_POINT('Ctrl Pts',(8.72382836146275,0.42371790764641,4.24973658040369));
#57590=CARTESIAN_POINT('Ctrl Pts',(8.75625730096992,0.148732406864234,4.41402322426773));
#57591=CARTESIAN_POINT('Ctrl Pts',(8.77278096178947,0.00546194790078228,
4.41654988270631));
#57592=CARTESIAN_POINT('Ctrl Pts',(8.77339934392141,9.95658017914599E-5,
4.41653262406943));
#57593=CARTESIAN_POINT('Origin',(3.42660065607856,0.,4.));
#57594=CARTESIAN_POINT('',(8.07660065607859,0.000145957947245773,4.41523406184916));
#57595=CARTESIAN_POINT('',(8.1733993439214,8.12049300508987E-5,4.41520065480005));
#57596=CARTESIAN_POINT('',(3.42660065607856,4.87367679877478E-13,4.415875));
#57597=CARTESIAN_POINT('Ctrl Pts',(8.07660065607858,0.00014595794724577,
4.41523406184916));
#57598=CARTESIAN_POINT('Ctrl Pts',(8.08558773785375,-0.0784131624224431,
4.41498734772332));
#57599=CARTESIAN_POINT('Ctrl Pts',(8.11048009831652,-0.296350794919178,
4.35572875890285));
#57600=CARTESIAN_POINT('Ctrl Pts',(8.15127773746691,-0.491827368180951,
4.00332637343646));
#57601=CARTESIAN_POINT('Ctrl Pts',(8.19899357352975,-0.268798940774433,
3.58811123553743));
#57602=CARTESIAN_POINT('Ctrl Pts',(8.24670940959259,0.201071689948468,3.55113988776764));
#57603=CARTESIAN_POINT('Ctrl Pts',(8.29442524565542,0.486295093906121,3.92636368766143));
#57604=CARTESIAN_POINT('Ctrl Pts',(8.33772232781743,0.339888039743562,4.32819890206972));
#57605=CARTESIAN_POINT('Ctrl Pts',(8.36511413129181,0.0997575609540166,
4.41482007364463));
#57606=CARTESIAN_POINT('Ctrl Pts',(8.37660065607859,-0.000374086211409545,
4.41568853448753));
#57607=CARTESIAN_POINT('Ctrl Pts',(8.1733993439214,8.12049300509751E-5,
4.41520065480005));
#57608=CARTESIAN_POINT('Ctrl Pts',(8.18191761753811,-0.0743948540356096,
4.41507113968239));
#57609=CARTESIAN_POINT('Ctrl Pts',(8.20634116984244,-0.288109900049694,
4.36032095112539));
#57610=CARTESIAN_POINT('Ctrl Pts',(8.24667000083438,-0.491516046133,4.01781014446235));
#57611=CARTESIAN_POINT('Ctrl Pts',(8.29438583689722,-0.280813212199106,
3.59620653211525));
#57612=CARTESIAN_POINT('Ctrl Pts',(8.34210167296004,0.187764715363875,3.54541267448783));
#57613=CARTESIAN_POINT('Ctrl Pts',(8.38981750902289,0.483915415676709,3.91207335260334));
#57614=CARTESIAN_POINT('Ctrl Pts',(8.43358339934334,0.347950231939931,4.32244196179047));
#57615=CARTESIAN_POINT('Ctrl Pts',(8.46144401097618,0.1037581297464,4.41486010664565));
#57616=CARTESIAN_POINT('Ctrl Pts',(8.47339934392141,-0.000383538171196768,
4.41580895574666));
#57617=CARTESIAN_POINT('Origin',(3.42660065607856,0.,4.));
#57618=CARTESIAN_POINT('',(7.77660065607858,0.000318631424802313,4.41622521972442));
#57619=CARTESIAN_POINT('',(7.8733993439214,0.000353153796088606,4.4161078667978));
#57620=CARTESIAN_POINT('',(3.42660065607856,4.87367679877478E-13,4.415875));
#57621=CARTESIAN_POINT('Ctrl Pts',(7.77660065607859,0.000318631424802297,
4.41622521972442));
#57622=CARTESIAN_POINT('Ctrl Pts',(7.79015606572807,-0.117457481003694,
4.41522659035305));
#57623=CARTESIAN_POINT('Ctrl Pts',(7.81961675406517,-0.375115671948731,
4.30131743988157));
#57624=CARTESIAN_POINT('Ctrl Pts',(7.86498272108989,-0.472647010158531,
3.86394843388276));
#57625=CARTESIAN_POINT('Ctrl Pts',(7.91269855715272,-0.141191260335066,
3.52886280888004));
#57626=CARTESIAN_POINT('Ctrl Pts',(7.96041439321556,0.31992259635559,3.62642971585976));
#57627=CARTESIAN_POINT('Ctrl Pts',(8.0081302292784,0.48724661017382,4.0670519628834));
#57628=CARTESIAN_POINT('Ctrl Pts',(8.04685898356608,0.259884401562094,4.37470733986759));
#57629=CARTESIAN_POINT('Ctrl Pts',(8.06968245916614,0.0606202562326388,
4.41542398077349));
#57630=CARTESIAN_POINT('Ctrl Pts',(8.07660065607858,0.00014595794724577,
4.41523406184916));
#57631=CARTESIAN_POINT('Ctrl Pts',(7.8733993439214,0.000353153796088627,
4.4161078667978));
#57632=CARTESIAN_POINT('Ctrl Pts',(7.88648594541244,-0.113432877329791,
4.41507910421771));
#57633=CARTESIAN_POINT('Ctrl Pts',(7.9154778255911,-0.367219156371593,4.30774647947464));
#57634=CARTESIAN_POINT('Ctrl Pts',(7.96037498445733,-0.476448943335793,
3.87792777037096));
#57635=CARTESIAN_POINT('Ctrl Pts',(8.0080908205202,-0.1550058622045,3.53322552818936));
#57636=CARTESIAN_POINT('Ctrl Pts',(8.05580665658301,0.308781487260178,3.61716946571973));
#57637=CARTESIAN_POINT('Ctrl Pts',(8.10352249264587,0.489010045760349,4.0526725734847));
#57638=CARTESIAN_POINT('Ctrl Pts',(8.14272005509199,0.26816615642074,4.37069430501912));
#57639=CARTESIAN_POINT('Ctrl Pts',(8.1660123388505,0.064666477720629,4.4153129696744));
#57640=CARTESIAN_POINT('Ctrl Pts',(8.1733993439214,8.12049300509751E-5,
4.41520065480005));
#57641=CARTESIAN_POINT('Origin',(3.42660065607856,0.,4.));
#57642=CARTESIAN_POINT('',(7.47660065607859,-0.000306770237538029,4.41625647512786));
#57643=CARTESIAN_POINT('',(7.5733993439214,-0.000257198714157858,4.41635988094829));
#57644=CARTESIAN_POINT('',(3.42660065607856,4.87367679877478E-13,4.415875));
#57645=CARTESIAN_POINT('Ctrl Pts',(7.47660065607859,-0.00030677023753798,
4.41625647512786));
#57646=CARTESIAN_POINT('Ctrl Pts',(7.47881911491479,-0.0195780710793754,
4.41641565502598));
#57647=CARTESIAN_POINT('Ctrl Pts',(7.4969428524386,-0.176849480241104,4.4064317922735));
#57648=CARTESIAN_POINT('Ctrl Pts',(7.53097186865002,-0.44664354691983,4.20594845626764));
#57649=CARTESIAN_POINT('Ctrl Pts',(7.57868770471286,-0.414791917646955,
3.73570302684109));
#57650=CARTESIAN_POINT('Ctrl Pts',(7.62640354077569,-0.00203048755240202,
3.50816557464413));
#57651=CARTESIAN_POINT('Ctrl Pts',(7.67411937683853,0.412595570264971,3.73228724307244));
#57652=CARTESIAN_POINT('Ctrl Pts',(7.72183521290137,0.448328767436039,4.20225365549051));
#57653=CARTESIAN_POINT('Ctrl Pts',(7.75599563931472,0.179163779268806,4.40574053813273));
#57654=CARTESIAN_POINT('Ctrl Pts',(7.77425078704046,0.0207354574140521,
4.41639833498254));
#57655=CARTESIAN_POINT('Ctrl Pts',(7.77660065607859,0.000318631424802297,
4.41622521972442));
#57656=CARTESIAN_POINT('Ctrl Pts',(7.5733993439214,-0.000257198714157839,
4.41635988094829));
#57657=CARTESIAN_POINT('Ctrl Pts',(7.57514899459915,-0.0154461882200338,
4.41646996636401));
#57658=CARTESIAN_POINT('Ctrl Pts',(7.59280392396451,-0.168599214901356,
4.40881268721627));
#57659=CARTESIAN_POINT('Ctrl Pts',(7.62636413201748,-0.440384235482588,
4.21901358396786));
#57660=CARTESIAN_POINT('Ctrl Pts',(7.67407996808031,-0.422396009600076,
3.7480340579683));
#57661=CARTESIAN_POINT('Ctrl Pts',(7.72179580414317,-0.0165150286377962,
3.50843873354525));
#57662=CARTESIAN_POINT('Ctrl Pts',(7.76951164020598,0.404531957204003,3.72025168374225));
#57663=CARTESIAN_POINT('Ctrl Pts',(7.81722747626884,0.454091022239626,4.18896181724392));
#57664=CARTESIAN_POINT('Ctrl Pts',(7.85185671084063,0.187425762196077,4.40318800700955));
#57665=CARTESIAN_POINT('Ctrl Pts',(7.87058066672482,0.02486112795907,4.41632944836175));
#57666=CARTESIAN_POINT('Ctrl Pts',(7.8733993439214,0.000353153796088627,
4.4161078667978));
#57667=CARTESIAN_POINT('Origin',(3.42660065607856,0.,4.));
#57668=CARTESIAN_POINT('',(7.17660065607858,-0.000163391746992416,4.4152468210878));
#57669=CARTESIAN_POINT('',(7.2733993439214,-0.000222139526412562,4.4153039283715));
#57670=CARTESIAN_POINT('',(3.42660065607856,4.87367679877478E-13,4.415875));
#57671=CARTESIAN_POINT('Ctrl Pts',(7.17660065607859,-0.000163391746992363,
4.4152468210878));
#57672=CARTESIAN_POINT('Ctrl Pts',(7.18338744278911,-0.0594844418834033,
4.41545575762517));
#57673=CARTESIAN_POINT('Ctrl Pts',(7.20607950818724,-0.257561782965025,
4.37580284351512));
#57674=CARTESIAN_POINT('Ctrl Pts',(7.24467685227299,-0.486676365692783,
4.07107270446015));
#57675=CARTESIAN_POINT('Ctrl Pts',(7.29239268833582,-0.322996137187983,
3.62908393881966));
#57676=CARTESIAN_POINT('Ctrl Pts',(7.34010852439867,0.137296434535941,3.52771310152703));
#57677=CARTESIAN_POINT('Ctrl Pts',(7.3878243604615,0.471507566988788,3.86005058906394));
#57678=CARTESIAN_POINT('Ctrl Pts',(7.43332173768814,0.377318713751663,4.29947917201381));
#57679=CARTESIAN_POINT('Ctrl Pts',(7.46291383622717,0.118587850938607,4.41527441201542));
#57680=CARTESIAN_POINT('Ctrl Pts',(7.47660065607859,-0.00030677023753798,
4.41625647512786));
#57681=CARTESIAN_POINT('Ctrl Pts',(7.2733993439214,-0.000222139526412493,
4.4153039283715));
#57682=CARTESIAN_POINT('Ctrl Pts',(7.27971732247348,-0.0554265094472961,
4.41557047734173));
#57683=CARTESIAN_POINT('Ctrl Pts',(7.30194057971316,-0.249272617462211,
4.37960776139715));
#57684=CARTESIAN_POINT('Ctrl Pts',(7.34006911564044,-0.484372034479295,
4.08537538031203));
#57685=CARTESIAN_POINT('Ctrl Pts',(7.3877849517033,-0.333780171974684,3.63875766810317));
#57686=CARTESIAN_POINT('Ctrl Pts',(7.43550078776612,0.123327161313159,3.52387434835784));
#57687=CARTESIAN_POINT('Ctrl Pts',(7.48321662382897,0.467181263150904,3.84622454030349));
#57688=CARTESIAN_POINT('Ctrl Pts',(7.52918280921405,0.385138488472668,4.29279105563264));
#57689=CARTESIAN_POINT('Ctrl Pts',(7.55924371591154,0.122630008444172,4.41546922990911));
#57690=CARTESIAN_POINT('Ctrl Pts',(7.5733993439214,-0.000257198714157839,
4.41635988094829));
#57691=CARTESIAN_POINT('Origin',(3.42660065607856,0.,4.));
#57692=CARTESIAN_POINT('',(6.87660065607859,0.000369753976522709,4.4156559906262));
#57693=CARTESIAN_POINT('',(6.9733993439214,0.000344359613660638,4.41554532105972));
#57694=CARTESIAN_POINT('',(3.42660065607856,4.87367679877478E-13,4.415875));
#57695=CARTESIAN_POINT('Ctrl Pts',(6.87660065607859,0.000369753976522759,
4.4156559906262));
#57696=CARTESIAN_POINT('Ctrl Pts',(6.88795577066343,-0.0986361616094132,
4.41481368816743));
#57697=CARTESIAN_POINT('Ctrl Pts',(6.91521616393589,-0.337621850525623,
4.32977807754403));
#57698=CARTESIAN_POINT('Ctrl Pts',(6.95838183589596,-0.486886005735063,
3.93038141845316));
#57699=CARTESIAN_POINT('Ctrl Pts',(7.0060976719588,-0.204771183672361,3.55281534000283));
#57700=CARTESIAN_POINT('Ctrl Pts',(7.05381350802163,0.265389096458903,3.58590591031157));
#57701=CARTESIAN_POINT('Ctrl Pts',(7.10152934408448,0.491837993618785,3.99926540470374));
#57702=CARTESIAN_POINT('Ctrl Pts',(7.14245839343679,0.298657604039877,4.35441002681052));
#57703=CARTESIAN_POINT('Ctrl Pts',(7.16748216410149,0.0795383202432945,
4.41496610118));
#57704=CARTESIAN_POINT('Ctrl Pts',(7.17660065607859,-0.000163391746992363,
4.4152468210878));
#57705=CARTESIAN_POINT('Ctrl Pts',(6.9733993439214,0.00034435961366068,
4.41554532105972));
#57706=CARTESIAN_POINT('Ctrl Pts',(6.9842856503478,-0.0946377878655052,
4.41480662962373));
#57707=CARTESIAN_POINT('Ctrl Pts',(7.0110772354618,-0.329510302625179,4.33529054280597));
#57708=CARTESIAN_POINT('Ctrl Pts',(7.05377409926342,-0.488725618924084,
3.94475128051735));
#57709=CARTESIAN_POINT('Ctrl Pts',(7.10148993532626,-0.21785253135038,3.55904022429238));
#57710=CARTESIAN_POINT('Ctrl Pts',(7.14920577138909,0.253078023397415,3.57826934481931));
#57711=CARTESIAN_POINT('Ctrl Pts',(7.19692160745195,0.491603063369337,3.98478019943955));
#57712=CARTESIAN_POINT('Ctrl Pts',(7.2383194649627,0.306874094293292,4.34959156107453));
#57713=CARTESIAN_POINT('Ctrl Pts',(7.26381204378586,0.0835484619188193,
4.41489945011039));
#57714=CARTESIAN_POINT('Ctrl Pts',(7.2733993439214,-0.000222139526412493,
4.4153039283715));
#57715=CARTESIAN_POINT('Origin',(3.42660065607856,0.,4.));
#57716=CARTESIAN_POINT('',(6.57660065607858,1.8302248101926E-5,4.41656360501758));
#57717=CARTESIAN_POINT('',(6.6733993439214,7.63499956435865E-5,4.4165465803965));
#57718=CARTESIAN_POINT('',(3.42660065607856,4.87367679877478E-13,4.415875));
#57719=CARTESIAN_POINT('Ctrl Pts',(6.57660065607858,1.83022481018748E-5,
4.41656360501758));
#57720=CARTESIAN_POINT('Ctrl Pts',(6.57661881985014,-0.000139156870309867,
4.41656362372179));
#57721=CARTESIAN_POINT('Ctrl Pts',(6.59254226230931,-0.138177237712184,
4.41649399470799));
#57722=CARTESIAN_POINT('Ctrl Pts',(6.62437098345609,-0.41404349770976,4.26553045144514));
#57723=CARTESIAN_POINT('Ctrl Pts',(6.67208681951894,-0.447234019333667,
3.79538894860702));
#57724=CARTESIAN_POINT('Ctrl Pts',(6.71980265558177,-0.0698021891909718,
3.51313682319347));
#57725=CARTESIAN_POINT('Ctrl Pts',(6.76751849164461,0.371772181936036,3.67798293440124));
#57726=CARTESIAN_POINT('Ctrl Pts',(6.81523432770745,0.471920133146607,4.13853999974893));
#57727=CARTESIAN_POINT('Ctrl Pts',(6.85159504918544,0.21800401543618,4.39254992240466));
#57728=CARTESIAN_POINT('Ctrl Pts',(6.87205049197582,0.0400429038769189,
4.41599351380864));
#57729=CARTESIAN_POINT('Ctrl Pts',(6.87660065607859,0.000369753976522759,
4.4156559906262));
#57730=CARTESIAN_POINT('Ctrl Pts',(6.6733993439214,7.63499956435956E-5,
4.4165465803965));
#57731=CARTESIAN_POINT('Ctrl Pts',(6.68885397822212,-0.133927014866661,
4.41622291450327));
#57732=CARTESIAN_POINT('Ctrl Pts',(6.72021389121046,-0.406451392834186,
4.27318229388465));
#57733=CARTESIAN_POINT('Ctrl Pts',(6.76747908288639,-0.453085647428837,
3.80864864857145));
#57734=CARTESIAN_POINT('Ctrl Pts',(6.81519491894923,-0.0841006081168706,
3.51540431248109));
#57735=CARTESIAN_POINT('Ctrl Pts',(6.86291075501207,0.362121456530253,3.66717299786736));
#57736=CARTESIAN_POINT('Ctrl Pts',(6.91062659107491,0.475798562415156,4.124581128109));
#57737=CARTESIAN_POINT('Ctrl Pts',(6.94745612071136,0.226294304474162,4.38932900794447));
#57738=CARTESIAN_POINT('Ctrl Pts',(6.96838037166019,0.0441344886838037,
4.41588588393584));
#57739=CARTESIAN_POINT('Ctrl Pts',(6.9733993439214,0.00034435961366068,
4.41554532105972));
#57740=CARTESIAN_POINT('Origin',(3.42660065607856,0.,4.));
#57741=CARTESIAN_POINT('',(6.27660065607859,-8.94903747701068E-6,4.41582842213685));
#57742=CARTESIAN_POINT('',(6.3733993439214,-0.000441664590319634,4.4157663968931));
#57743=CARTESIAN_POINT('',(3.42660065607856,4.87367679877478E-13,4.415875));
#57744=CARTESIAN_POINT('Ctrl Pts',(6.27660065607859,-8.94903747701223E-6,
4.41582842213685));
#57745=CARTESIAN_POINT('Ctrl Pts',(6.28118714772447,-0.0399801639742102,
4.41579747358059));
#57746=CARTESIAN_POINT('Ctrl Pts',(6.29372627871415,-0.149263049162913,
4.40013952362907));
#57747=CARTESIAN_POINT('Ctrl Pts',(6.31421804904765,-0.307151379675736,
4.3060270879454));
#57748=CARTESIAN_POINT('Ctrl Pts',(6.33807596707907,-0.416657206472865,
4.12081787696614));
#57749=CARTESIAN_POINT('Ctrl Pts',(6.36193388511048,-0.422829889105799,
3.9075587958503));
#57750=CARTESIAN_POINT('Ctrl Pts',(6.39374444248571,-0.296437506874183,
3.64987069373525));
#57751=CARTESIAN_POINT('Ctrl Pts',(6.43350763920474,0.0703302468340302,
3.51324810367198));
#57752=CARTESIAN_POINT('Ctrl Pts',(6.48122347526758,0.448014600657906,3.7964368525222));
#57753=CARTESIAN_POINT('Ctrl Pts',(6.52892114755886,0.413253290380966,4.26628466471864));
#57754=CARTESIAN_POINT('Ctrl Pts',(6.56071354116253,0.137741412285014,4.41654724519979));
#57755=CARTESIAN_POINT('Ctrl Pts',(6.57660065607858,1.83022481018748E-5,
4.41656360501758));
#57756=CARTESIAN_POINT('Ctrl Pts',(6.3733993439214,-0.000441664590319611,
4.4157663968931));
#57757=CARTESIAN_POINT('Ctrl Pts',(6.37751702740883,-0.0362476131304844,
4.41610293027605));
#57758=CARTESIAN_POINT('Ctrl Pts',(6.39753998958387,-0.210006484715375,
4.39546152579387));
#57759=CARTESIAN_POINT('Ctrl Pts',(6.43346823044653,-0.468271923807345,
4.15124960425567));
#57760=CARTESIAN_POINT('Ctrl Pts',(6.48118406650937,-0.380227249479543,
3.6882349865083));
#57761=CARTESIAN_POINT('Ctrl Pts',(6.52889990257221,0.0564566449812287,
3.51140415777354));
#57762=CARTESIAN_POINT('Ctrl Pts',(6.57661573863504,0.441574375138847,3.78331933667001));
#57763=CARTESIAN_POINT('Ctrl Pts',(6.62433157469789,0.421040068198854,4.25418342072721));
#57764=CARTESIAN_POINT('Ctrl Pts',(6.65659277646,0.145792717270209,4.41473316952435));
#57765=CARTESIAN_POINT('Ctrl Pts',(6.6729486995345,0.00398377756883227,
4.41655601822694));
#57766=CARTESIAN_POINT('Ctrl Pts',(6.6733993439214,7.63499956435956E-5,
4.4165465803965));
#57767=CARTESIAN_POINT('Origin',(3.42660065607856,0.,4.));
#57768=CARTESIAN_POINT('',(5.97660065607859,-9.19412645702589E-6,4.41589218083175));
#57769=CARTESIAN_POINT('',(6.0733993439214,-6.65563173402051E-6,4.41590255337155));
#57770=CARTESIAN_POINT('',(3.42660065607856,4.87367679877478E-13,4.415875));
#57771=CARTESIAN_POINT('Ctrl Pts',(5.97660065607858,-9.19412645705893E-6,
4.41589218083175));
#57772=CARTESIAN_POINT('Ctrl Pts',(5.97780283625498,-0.0104787976275591,
4.4159022685469));
#57773=CARTESIAN_POINT('Ctrl Pts',(5.98695765577519,-0.0902010538040918,
4.41295272969856));
#57774=CARTESIAN_POINT('Ctrl Pts',(6.0040651146392,-0.23587461323539,4.36380751861078));
#57775=CARTESIAN_POINT('Ctrl Pts',(6.02792303267061,-0.381351759249696,
4.20630938167977));
#57776=CARTESIAN_POINT('Ctrl Pts',(6.05178095070204,-0.433578399193506,
3.9983625870902));
#57777=CARTESIAN_POINT('Ctrl Pts',(6.07563886873346,-0.379782579589031,
3.79081692866841));
#57778=CARTESIAN_POINT('Ctrl Pts',(6.09949678676487,-0.233120953551068,
3.63442082419035));
#57779=CARTESIAN_POINT('Ctrl Pts',(6.12335470479629,-0.0294522997972467,
3.5674214393556));
#57780=CARTESIAN_POINT('Ctrl Pts',(6.14721262282771,0.181413325723775,3.60619428643423));
#57781=CARTESIAN_POINT('Ctrl Pts',(6.17107054085913,0.347927737305898,3.74127281623538));
#57782=CARTESIAN_POINT('Ctrl Pts',(6.19492845889055,0.429346806292137,3.93959933010928));
#57783=CARTESIAN_POINT('Ctrl Pts',(6.21878637692197,0.405811992579865,4.15272917617017));
#57784=CARTESIAN_POINT('Ctrl Pts',(6.24264429495339,0.282982581651336,4.32844890303245));
#57785=CARTESIAN_POINT('Ctrl Pts',(6.26191572133893,0.127967070080381,4.40561019629887));
#57786=CARTESIAN_POINT('Ctrl Pts',(6.27323450838066,0.029326984292613,4.415851136102));
#57787=CARTESIAN_POINT('Ctrl Pts',(6.27660065607859,-8.94903747701223E-6,
4.41582842213685));
#57788=CARTESIAN_POINT('Ctrl Pts',(6.0733993439214,-6.65563173397714E-6,
4.41590255337156));
#57789=CARTESIAN_POINT('Ctrl Pts',(6.07413271593935,-0.00639299139291402,
4.41590724351385));
#57790=CARTESIAN_POINT('Ctrl Pts',(6.0828187273011,-0.0820297780542147,
4.41420140028919));
#57791=CARTESIAN_POINT('Ctrl Pts',(6.09945737800665,-0.2250554921608,4.3705991908187));
#57792=CARTESIAN_POINT('Ctrl Pts',(6.12331529603809,-0.375113923638194,
4.21744656883549));
#57793=CARTESIAN_POINT('Ctrl Pts',(6.1471732140695,-0.433431396087355,4.01114207710762));
#57794=CARTESIAN_POINT('Ctrl Pts',(6.17103113210093,-0.385792139046387,
3.80207577201042));
#57795=CARTESIAN_POINT('Ctrl Pts',(6.19488905013233,-0.243761337718234,
3.64147770828707));
#57796=CARTESIAN_POINT('Ctrl Pts',(6.21874696816376,-0.042227823444436,
3.56841523311022));
#57797=CARTESIAN_POINT('Ctrl Pts',(6.24260488619517,0.16982704650124,3.60113783246665));
#57798=CARTESIAN_POINT('Ctrl Pts',(6.2664628042266,0.339985970990829,3.73091992247201));
#57799=CARTESIAN_POINT('Ctrl Pts',(6.29032072225801,0.427700638223926,3.92738904240251));
#57800=CARTESIAN_POINT('Ctrl Pts',(6.31417864028943,0.409561128158778,4.13996490148311));
#57801=CARTESIAN_POINT('Ctrl Pts',(6.34187151417723,0.27471212230801,4.35031587281991));
#57802=CARTESIAN_POINT('Ctrl Pts',(6.36161174872122,0.102059178040878,4.41480301073152));
#57803=CARTESIAN_POINT('Ctrl Pts',(6.3733993439214,-0.000441664590319611,
4.4157663968931));
#57804=CARTESIAN_POINT('Origin',(3.42660065607856,0.,4.));
#57805=CARTESIAN_POINT('',(5.67660065607858,1.06631253201556E-5,4.41586554077139));
#57806=CARTESIAN_POINT('',(5.7733993439214,9.17748676071416E-6,4.4158542849441));
#57807=CARTESIAN_POINT('',(3.42660065607856,4.87367679877478E-13,4.415875));
#57808=CARTESIAN_POINT('Ctrl Pts',(5.67660065607858,1.06631253201268E-5,
4.41586554077139));
#57809=CARTESIAN_POINT('Ctrl Pts',(5.68237116412931,-0.050253077703417,
4.41581669384736));
#57810=CARTESIAN_POINT('Ctrl Pts',(5.69609431152383,-0.169828933264711,
4.3941204493343));
#57811=CARTESIAN_POINT('Ctrl Pts',(5.71777009826218,-0.329222253834466,
4.28214440376531));
#57812=CARTESIAN_POINT('Ctrl Pts',(5.74162801629359,-0.424158110434281,
4.08990358344764));
#57813=CARTESIAN_POINT('Ctrl Pts',(5.76548593432501,-0.415375755386326,
3.8756788878607));
#57814=CARTESIAN_POINT('Ctrl Pts',(5.78934385235642,-0.305022713182347,
3.69185409099321));
#57815=CARTESIAN_POINT('Ctrl Pts',(5.81320177038785,-0.120083309624962,
3.58337936191985));
#57816=CARTESIAN_POINT('Ctrl Pts',(5.83705968841926,0.0942197354074567,
3.57677972866706));
#57817=CARTESIAN_POINT('Ctrl Pts',(5.86091760645069,0.285483486244351,3.673668977605));
#57818=CARTESIAN_POINT('Ctrl Pts',(5.8847755244821,0.406938752801468,3.85035505520226));
#57819=CARTESIAN_POINT('Ctrl Pts',(5.90863344251353,0.428886400972996,4.06363338935351));
#57820=CARTESIAN_POINT('Ctrl Pts',(5.93249136054494,0.345959657594393,4.261351642888));
#57821=CARTESIAN_POINT('Ctrl Pts',(5.95514709839996,0.186877681905787,4.38841966610496));
#57822=CARTESIAN_POINT('Ctrl Pts',(5.96985019691118,0.0587795235055939,
4.41583553648629));
#57823=CARTESIAN_POINT('Ctrl Pts',(5.97660065607858,-9.19412645705893E-6,
4.41589218083175));
#57824=CARTESIAN_POINT('Ctrl Pts',(5.7733993439214,9.17748676073846E-6,
4.4158542849441));
#57825=CARTESIAN_POINT('Ctrl Pts',(5.77870104381367,-0.0461746181927863,
4.41581721944429));
#57826=CARTESIAN_POINT('Ctrl Pts',(5.79195538304975,-0.161664917198308,
4.3966319946429));
#57827=CARTESIAN_POINT('Ctrl Pts',(5.81316236162963,-0.320769768688322,
4.29171820750724));
#57828=CARTESIAN_POINT('Ctrl Pts',(5.83702027966105,-0.421326288178809,
4.10235681181338));
#57829=CARTESIAN_POINT('Ctrl Pts',(5.86087819769247,-0.418857046020503,
3.88796639709818));
#57830=CARTESIAN_POINT('Ctrl Pts',(5.88473611572389,-0.313965860818636,
3.70097123187977));
#57831=CARTESIAN_POINT('Ctrl Pts',(5.90859403375531,-0.132301443679057,
3.58709678011166));
#57832=CARTESIAN_POINT('Ctrl Pts',(5.93245195178673,0.0817142298265842,
3.57418834816524));
#57833=CARTESIAN_POINT('Ctrl Pts',(5.95630986981814,0.275748643515392,3.66540258613358));
#57834=CARTESIAN_POINT('Ctrl Pts',(5.98016778784957,0.402354822815078,3.83843477537114));
#57835=CARTESIAN_POINT('Ctrl Pts',(6.00402570588098,0.430574627524036,4.05097449853386));
#57836=CARTESIAN_POINT('Ctrl Pts',(6.02788362391241,0.353506566116634,4.25104874587108));
#57837=CARTESIAN_POINT('Ctrl Pts',(6.05100816992587,0.195023852357142,4.38547315270063));
#57838=CARTESIAN_POINT('Ctrl Pts',(6.06618007659554,0.06286002589468,4.4158563839102));
#57839=CARTESIAN_POINT('Ctrl Pts',(6.0733993439214,-6.65563173397714E-6,
4.41590255337156));
#57840=CARTESIAN_POINT('Origin',(3.42660065607856,0.,4.));
#57841=CARTESIAN_POINT('',(5.37660065607858,-1.01751121954902E-5,4.41586038335289));
#57842=CARTESIAN_POINT('',(5.4733993439214,-1.09014992595302E-5,4.41587264340464));
#57843=CARTESIAN_POINT('',(3.42660065607856,4.87367679877478E-13,4.415875));
#57844=CARTESIAN_POINT('Ctrl Pts',(5.37660065607859,-1.01751121954468E-5,
4.41586038335289));
#57845=CARTESIAN_POINT('Ctrl Pts',(5.37898685265982,-0.0207957689391596,
4.41587928195339));
#57846=CARTESIAN_POINT('Ctrl Pts',(5.38932568858487,-0.110842971866809,
4.40924760552439));
#57847=CARTESIAN_POINT('Ctrl Pts',(5.40761716385372,-0.26226226804932,4.34526983614494));
#57848=CARTESIAN_POINT('Ctrl Pts',(5.43147508188515,-0.395631058815178,
4.17739453851434));
#57849=CARTESIAN_POINT('Ctrl Pts',(5.45533299991656,-0.432257278927009,
3.96614144408682));
#57850=CARTESIAN_POINT('Ctrl Pts',(5.47919091794798,-0.363184819889405,
3.76316768886851));
#57851=CARTESIAN_POINT('Ctrl Pts',(5.5030488359794,-0.205303779432806,3.61810588490468));
#57852=CARTESIAN_POINT('Ctrl Pts',(5.52690675401082,0.00277962745745752,
3.56642759466814));
#57853=CARTESIAN_POINT('Ctrl Pts',(5.55076467204224,0.210183339719457,3.62076956781107));
#57854=CARTESIAN_POINT('Ctrl Pts',(5.57462259007365,0.36619150013966,3.76784371165257));
#57855=CARTESIAN_POINT('Ctrl Pts',(5.59848050810508,0.432655863921731,3.97168639180759));
#57856=CARTESIAN_POINT('Ctrl Pts',(5.62233842613649,0.393324083661671,4.18245252040861));
#57857=CARTESIAN_POINT('Ctrl Pts',(5.64619634416792,0.257813851021257,4.34860403787086));
#57858=CARTESIAN_POINT('Ctrl Pts',(5.66428375414861,0.107285005985459,4.40994309575933));
#57859=CARTESIAN_POINT('Ctrl Pts',(5.6744185247855,0.0190180158238588,4.41588401235146));
#57860=CARTESIAN_POINT('Ctrl Pts',(5.67660065607858,1.06631253201268E-5,
4.41586554077139));
#57861=CARTESIAN_POINT('Ctrl Pts',(5.4733993439214,-1.0901499259525E-5,
4.41587264340464));
#57862=CARTESIAN_POINT('Ctrl Pts',(5.47531673234419,-0.0167114040746605,
4.41588973972128));
#57863=CARTESIAN_POINT('Ctrl Pts',(5.48518676011079,-0.102669266038577,
4.41080986982701));
#57864=CARTESIAN_POINT('Ctrl Pts',(5.50300942722118,-0.251979671819092,
4.35284416104532));
#57865=CARTESIAN_POINT('Ctrl Pts',(5.52686734525261,-0.390234841353927,
4.18896964197264));
#57866=CARTESIAN_POINT('Ctrl Pts',(5.55072526328402,-0.433066962396004,
3.97888689800548));
#57867=CARTESIAN_POINT('Ctrl Pts',(5.57458318131544,-0.370002414621403,
3.77396688259));
#57868=CARTESIAN_POINT('Ctrl Pts',(5.59844109934686,-0.21646219781534,3.62431812139094));
#57869=CARTESIAN_POINT('Ctrl Pts',(5.62229901737828,-0.00999107731853999,
3.56653381289738));
#57870=CARTESIAN_POINT('Ctrl Pts',(5.64615693540971,0.198923133709572,3.61474379450078));
#57871=CARTESIAN_POINT('Ctrl Pts',(5.67001485344111,0.359195220034686,3.75715941257656));
#57872=CARTESIAN_POINT('Ctrl Pts',(5.69387277147254,0.431634290692432,3.95895616900985));
#57873=CARTESIAN_POINT('Ctrl Pts',(5.71773068950395,0.398527019959163,4.1707892603438));
#57874=CARTESIAN_POINT('Ctrl Pts',(5.74158860753538,0.267969036875697,4.34085972491723));
#57875=CARTESIAN_POINT('Ctrl Pts',(5.76014482567452,0.115458993192439,4.40830959117706));
#57876=CARTESIAN_POINT('Ctrl Pts',(5.77074840446986,0.0231018550196917,
4.41587281831976));
#57877=CARTESIAN_POINT('Ctrl Pts',(5.7733993439214,9.17748676073846E-6,
4.4158542849441));
#57878=CARTESIAN_POINT('Origin',(3.42660065607856,0.,4.));
#57879=CARTESIAN_POINT('',(5.07660065607859,8.10857529294212E-6,4.41589722116852));
#57880=CARTESIAN_POINT('',(5.1733993439214,1.02299162792543E-5,4.4158851107878));
#57881=CARTESIAN_POINT('',(3.42660065607856,4.87367679877478E-13,4.415875));
#57882=CARTESIAN_POINT('Ctrl Pts',(5.07660065607858,8.10857529294148E-6,
4.41589722116852));
#57883=CARTESIAN_POINT('Ctrl Pts',(5.08355518053415,-0.060555656273516,
4.41584370653314));
#57884=CARTESIAN_POINT('Ctrl Pts',(5.09846234433351,-0.190424342306974,
4.38715451669839));
#57885=CARTESIAN_POINT('Ctrl Pts',(5.1213221474767,-0.349282119693095,4.256894448863));
#57886=CARTESIAN_POINT('Ctrl Pts',(5.1451800655081,-0.4296670234643,4.05812921762123));
#57887=CARTESIAN_POINT('Ctrl Pts',(5.16903798353954,-0.404986636103755,
3.84514980926298));
#57888=CARTESIAN_POINT('Ctrl Pts',(5.19289590157095,-0.281275984601366,
3.67003549057442));
#57889=CARTESIAN_POINT('Ctrl Pts',(5.21675381960238,-0.0887856930599551,
3.5756064824932));
#57890=CARTESIAN_POINT('Ctrl Pts',(5.24061173763379,0.125415118908336,3.58495324968971));
#57891=CARTESIAN_POINT('Ctrl Pts',(5.26446965566521,0.308948518064291,3.69579025298356));
#57892=CARTESIAN_POINT('Ctrl Pts',(5.28832757369662,0.416935588964862,3.88101482593007));
#57893=CARTESIAN_POINT('Ctrl Pts',(5.31218549172805,0.422970551266107,4.09533451502773));
#57894=CARTESIAN_POINT('Ctrl Pts',(5.33604340975946,0.325577692296299,4.28634231834109));
#57895=CARTESIAN_POINT('Ctrl Pts',(5.35751513120965,0.166275769440666,4.39523064161658));
#57896=CARTESIAN_POINT('Ctrl Pts',(5.37103421331602,0.0484777907299229,
4.41581629730449));
#57897=CARTESIAN_POINT('Ctrl Pts',(5.37660065607859,-1.01751121954468E-5,
4.41586038335289));
#57898=CARTESIAN_POINT('Ctrl Pts',(5.1733993439214,1.02299162792474E-5,
4.4158851107878));
#57899=CARTESIAN_POINT('Ctrl Pts',(5.17988506021851,-0.0564756498766958,
4.41582730150705));
#57900=CARTESIAN_POINT('Ctrl Pts',(5.19432341585943,-0.182274442988225,
4.39002065289559));
#57901=CARTESIAN_POINT('Ctrl Pts',(5.21671441084416,-0.341564590845109,
4.26707000444592));
#57902=CARTESIAN_POINT('Ctrl Pts',(5.24057232887557,-0.427768622694993,
4.07075847957352));
#57903=CARTESIAN_POINT('Ctrl Pts',(5.264430246907,-0.409371574112622,3.85714457902312));
#57904=CARTESIAN_POINT('Ctrl Pts',(5.2882881649384,-0.290872024601924,3.6784627202051));
#57905=CARTESIAN_POINT('Ctrl Pts',(5.31214608296984,-0.101246341881189,
3.57840548479658));
#57906=CARTESIAN_POINT('Ctrl Pts',(5.33600400100125,0.113136829324483,3.58143959235932));
#57907=CARTESIAN_POINT('Ctrl Pts',(5.35986191903268,0.299854963974951,3.68682312094679));
#57908=CARTESIAN_POINT('Ctrl Pts',(5.38371983706408,0.413250392048343,3.8687869272297));
#57909=CARTESIAN_POINT('Ctrl Pts',(5.40757775509551,0.425594842551202,4.08283590397723));
#57910=CARTESIAN_POINT('Ctrl Pts',(5.43143567312693,0.333869761079625,4.27662924579771));
#57911=CARTESIAN_POINT('Ctrl Pts',(5.45337620273556,0.174437273907163,4.39264091290779));
#57912=CARTESIAN_POINT('Ctrl Pts',(5.46736409300038,0.0525562895569378,
4.41581883033293));
#57913=CARTESIAN_POINT('Ctrl Pts',(5.4733993439214,-1.0901499259525E-5,
4.41587264340464));
#57914=CARTESIAN_POINT('Origin',(3.42660065607856,0.,4.));
#57915=CARTESIAN_POINT('',(4.77660065607858,-3.27394476109793E-6,4.41584059078716));
#57916=CARTESIAN_POINT('',(4.8733993439214,-6.67049670156904E-6,4.4158459349409));
#57917=CARTESIAN_POINT('',(3.42660065607856,4.87367679877478E-13,4.415875));
#57918=CARTESIAN_POINT('Ctrl Pts',(4.77660065607858,-3.27394476113199E-6,
4.41584059078717));
#57919=CARTESIAN_POINT('Ctrl Pts',(4.78017086906467,-0.0311067951354469,
4.4158491206715));
#57920=CARTESIAN_POINT('Ctrl Pts',(4.79169372139456,-0.131487321212171,
4.40473555835468));
#57921=CARTESIAN_POINT('Ctrl Pts',(4.81116921306824,-0.287199161490599,
4.32482210305491));
#57922=CARTESIAN_POINT('Ctrl Pts',(4.83502713109967,-0.407721671464292,
4.14749845969467));
#57923=CARTESIAN_POINT('Ctrl Pts',(4.85888504913109,-0.42854512664958,3.93410742516172));
#57924=CARTESIAN_POINT('Ctrl Pts',(4.8827429671625,-0.344577625034195,3.73682892005441));
#57925=CARTESIAN_POINT('Ctrl Pts',(4.90660088519393,-0.176351507991885,
3.60390291263011));
#57926=CARTESIAN_POINT('Ctrl Pts',(4.93045880322534,0.0349973564730633,
3.56783343253575));
#57927=CARTESIAN_POINT('Ctrl Pts',(4.95431672125677,0.237788413971502,3.63744045016736));
#57928=CARTESIAN_POINT('Ctrl Pts',(4.97817463928818,0.382433727027559,3.79570315365689));
#57929=CARTESIAN_POINT('Ctrl Pts',(5.0020325573196,0.433563576539811,4.00392200101168));
#57930=CARTESIAN_POINT('Ctrl Pts',(5.02589047535102,0.378675321553375,4.21118181228595));
#57931=CARTESIAN_POINT('Ctrl Pts',(5.04974839338244,0.231190635538481,4.36680191797922));
#57932=CARTESIAN_POINT('Ctrl Pts',(5.0666517869583,0.086644022961884,4.4135113916189));
#57933=CARTESIAN_POINT('Ctrl Pts',(5.07560254119034,0.00870023350343714,
4.41590490160082));
#57934=CARTESIAN_POINT('Ctrl Pts',(5.07660065607858,8.10857529294148E-6,
4.41589722116852));
#57935=CARTESIAN_POINT('Ctrl Pts',(4.8733993439214,-6.67049670157252E-6,
4.41584593494091));
#57936=CARTESIAN_POINT('Ctrl Pts',(4.87650074874903,-0.0270249643080214,
4.41586127519519));
#57937=CARTESIAN_POINT('Ctrl Pts',(4.88755479292047,-0.123313358466266,
4.40662010077424));
#57938=CARTESIAN_POINT('Ctrl Pts',(4.90656147643571,-0.277507970732168,
4.33313973520738));
#57939=CARTESIAN_POINT('Ctrl Pts',(4.93041939446713,-0.403200703213916,
4.15944262266324));
#57940=CARTESIAN_POINT('Ctrl Pts',(4.95427731249855,-0.430299880793222,
3.94675744574809));
#57941=CARTESIAN_POINT('Ctrl Pts',(4.97813523052996,-0.352179016385168,
3.7470915236456));
#57942=CARTESIAN_POINT('Ctrl Pts',(5.00199314856139,-0.187940789307144,
3.60926861310034));
#57943=CARTESIAN_POINT('Ctrl Pts',(5.0258510665928,0.0222540801607904,3.56699016996131));
#57944=CARTESIAN_POINT('Ctrl Pts',(5.04970898462423,0.227007220840439,3.63059442521772));
#57945=CARTESIAN_POINT('Ctrl Pts',(5.07356690265564,0.376250912472057,3.7845284059142));
#57946=CARTESIAN_POINT('Ctrl Pts',(5.09742482068706,0.433491007135177,3.99115106069306));
#57947=CARTESIAN_POINT('Ctrl Pts',(5.12128273871848,0.384730742495793,4.19993752217271));
#57948=CARTESIAN_POINT('Ctrl Pts',(5.1451406567499,0.241893331461176,4.35983381329239));
#57949=CARTESIAN_POINT('Ctrl Pts',(5.16251285848421,0.0948160588051851,
4.41219316122439));
#57950=CARTESIAN_POINT('Ctrl Pts',(5.17193242087471,0.0127860645481494,
4.41589818594594));
#57951=CARTESIAN_POINT('Ctrl Pts',(5.1733993439214,1.02299162792474E-5,
4.4158851107878));
#57952=CARTESIAN_POINT('Origin',(3.42660065607856,0.,4.));
#57953=CARTESIAN_POINT('',(4.47660065607858,-1.72413508574122E-6,4.41591032029986));
#57954=CARTESIAN_POINT('',(4.5733993439214,2.6062779713001E-6,4.4159095790646));
#57955=CARTESIAN_POINT('',(3.42660065607856,4.87367679877478E-13,4.415875));
#57956=CARTESIAN_POINT('Ctrl Pts',(4.47660065607858,-1.72413508575881E-6,
4.41591032029986));
#57957=CARTESIAN_POINT('Ctrl Pts',(4.47678655759518,-0.00162050728124812,
4.41591069657345));
#57958=CARTESIAN_POINT('Ctrl Pts',(4.48492509845559,-0.0724886630755744,
4.4155056303295));
#57959=CARTESIAN_POINT('Ctrl Pts',(4.5010162786598,-0.212178818846594,4.37811758201071));
#57960=CARTESIAN_POINT('Ctrl Pts',(4.52487419669122,-0.367409789343613,
4.23022337776645));
#57961=CARTESIAN_POINT('Ctrl Pts',(4.54873211472264,-0.432799058467291,
4.02603328640456));
#57962=CARTESIAN_POINT('Ctrl Pts',(4.57259003275406,-0.392357168499796,
3.8154773474345));
#57963=CARTESIAN_POINT('Ctrl Pts',(4.59644795078547,-0.255973263285106,
3.65004222328625));
#57964=CARTESIAN_POINT('Ctrl Pts',(4.6203058688169,-0.0569969226013119,
3.57018130821703));
#57965=CARTESIAN_POINT('Ctrl Pts',(4.64416378684831,0.155916718210686,3.59542277130738));
#57966=CARTESIAN_POINT('Ctrl Pts',(4.66802170487973,0.330704474340828,3.71959438727947));
#57967=CARTESIAN_POINT('Ctrl Pts',(4.69187962291115,0.424625978282027,3.91233281365517));
#57968=CARTESIAN_POINT('Ctrl Pts',(4.71573754094257,0.41471486395576,4.1265082550995));
#57969=CARTESIAN_POINT('Ctrl Pts',(4.73959545897399,0.303394668785218,4.30974898215573));
#57970=CARTESIAN_POINT('Ctrl Pts',(4.75988316401932,0.145646585585232,4.40116103141851));
#57971=CARTESIAN_POINT('Ctrl Pts',(4.77221822972086,0.0381762104768988,
4.41583012037823));
#57972=CARTESIAN_POINT('Ctrl Pts',(4.77660065607858,-3.27394476113199E-6,
4.41584059078717));
#57973=CARTESIAN_POINT('Ctrl Pts',(4.5733993439214,2.60627797130011E-6,
4.4159095790646));
#57974=CARTESIAN_POINT('Ctrl Pts',(4.58106907662335,-0.0667838229435618,
4.4158868274511));
#57975=CARTESIAN_POINT('Ctrl Pts',(4.59669144866912,-0.202842099803805,
4.38250385602613));
#57976=CARTESIAN_POINT('Ctrl Pts',(4.62026646005868,-0.360469908510665,
4.24094439618412));
#57977=CARTESIAN_POINT('Ctrl Pts',(4.6441243780901,-0.431844582779732,4.03876871570463));
#57978=CARTESIAN_POINT('Ctrl Pts',(4.66798229612152,-0.397621493350665,
3.82711302819544));
#57979=CARTESIAN_POINT('Ctrl Pts',(4.69184021415294,-0.266169117804412,
3.65773291463971));
#57980=CARTESIAN_POINT('Ctrl Pts',(4.71569813218436,-0.0696311426542753,
3.57204642662242));
#57981=CARTESIAN_POINT('Ctrl Pts',(4.73955605021577,0.143933543589337,3.59100624451743));
#57982=CARTESIAN_POINT('Ctrl Pts',(4.76341396824719,0.322302557754209,3.70997617639404));
#57983=CARTESIAN_POINT('Ctrl Pts',(4.78727188627862,0.421859817202848,3.8998648332327));
#57984=CARTESIAN_POINT('Ctrl Pts',(4.81112980431003,0.41826086011465,4.11423926597311));
#57985=CARTESIAN_POINT('Ctrl Pts',(4.83498772234146,0.312385729531365,4.30067908636799));
#57986=CARTESIAN_POINT('Ctrl Pts',(4.85574423554524,0.15381688120809,4.39891624198015));
#57987=CARTESIAN_POINT('Ctrl Pts',(4.86854810940522,0.04225549351942,4.41582193963064));
#57988=CARTESIAN_POINT('Ctrl Pts',(4.8733993439214,-6.67049670157252E-6,
4.41584593494091));
#57989=CARTESIAN_POINT('Origin',(3.42660065607856,0.,4.));
#57990=CARTESIAN_POINT('',(4.17660065607858,5.88453344125852E-6,4.41584444980552));
#57991=CARTESIAN_POINT('',(4.2733993439214,2.51014653358805E-6,4.41583996132385));
#57992=CARTESIAN_POINT('',(3.42660065607856,4.87367679877478E-13,4.415875));
#57993=CARTESIAN_POINT('Ctrl Pts',(4.17660065607858,5.88453344126799E-6,
4.41584444980552));
#57994=CARTESIAN_POINT('Ctrl Pts',(4.18135488546951,-0.0414115481342504,
4.41582334930757));
#57995=CARTESIAN_POINT('Ctrl Pts',(4.19406175420423,-0.152126265423154,
4.3993918905015));
#57996=CARTESIAN_POINT('Ctrl Pts',(4.21472126228278,-0.310547447266788,
4.30257739619942));
#57997=CARTESIAN_POINT('Ctrl Pts',(4.23857918031418,-0.417556725585918,
4.11678647978038));
#57998=CARTESIAN_POINT('Ctrl Pts',(4.26243709834561,-0.422462345057068,
3.90243789311793));
#57999=CARTESIAN_POINT('Ctrl Pts',(4.28629501637703,-0.324064236326554,
3.71194600226016));
#58000=CARTESIAN_POINT('Ctrl Pts',(4.31015293440845,-0.146423688323203,
3.59189110566319));
#58001=CARTESIAN_POINT('Ctrl Pts',(4.33401085243986,0.0670214896752265,
3.5716299793216));
#58002=CARTESIAN_POINT('Ctrl Pts',(4.35786877047129,0.264078061498623,3.65611697628114));
#58003=CARTESIAN_POINT('Ctrl Pts',(4.38172668850271,0.396560367883193,3.82469274783887));
#58004=CARTESIAN_POINT('Ctrl Pts',(4.40558460653412,0.432072854850341,4.03613591352675));
#58005=CARTESIAN_POINT('Ctrl Pts',(4.42944252456555,0.361931763288092,4.23874286631049));
#58006=CARTESIAN_POINT('Ctrl Pts',(4.45311454108036,0.204524647174786,4.38184685695289));
#58007=CARTESIAN_POINT('Ctrl Pts',(4.46883391825138,0.0676290543833733,
4.4158946000499));
#58008=CARTESIAN_POINT('Ctrl Pts',(4.47660065607858,-1.72413508575881E-6,
4.41591032029986));
#58009=CARTESIAN_POINT('Ctrl Pts',(4.2733993439214,2.51014653359152E-6,
4.41583996132385));
#58010=CARTESIAN_POINT('Ctrl Pts',(4.27768476515387,-0.0373320337329404,
4.41583213221101));
#58011=CARTESIAN_POINT('Ctrl Pts',(4.28992282573015,-0.143955736965383,
4.40160880992953));
#58012=CARTESIAN_POINT('Ctrl Pts',(4.31011352565024,-0.301501118270308,
4.3115924136571));
#58013=CARTESIAN_POINT('Ctrl Pts',(4.33397144368164,-0.413936097932681,
4.12903358037428));
#58014=CARTESIAN_POINT('Ctrl Pts',(4.35782936171308,-0.425152419412173,
3.91492252699502));
#58015=CARTESIAN_POINT('Ctrl Pts',(4.38168727974448,-0.332407397051365,
3.72161523052345));
#58016=CARTESIAN_POINT('Ctrl Pts',(4.40554519777592,-0.158379709595794,
3.5963805946708));
#58017=CARTESIAN_POINT('Ctrl Pts',(4.42940311580732,0.0543761300157755,
3.56984189703405));
#58018=CARTESIAN_POINT('Ctrl Pts',(4.45326103383876,0.25383552520097,3.64848857324589));
#58019=CARTESIAN_POINT('Ctrl Pts',(4.47711895187016,0.39122521984844,3.81308936806525));
#58020=CARTESIAN_POINT('Ctrl Pts',(4.50097686990159,0.432949691632991,4.02339490384879));
#58021=CARTESIAN_POINT('Ctrl Pts',(4.524834787933,0.368806170420464,4.22797974831721));
#58022=CARTESIAN_POINT('Ctrl Pts',(4.54869270596443,0.214479494504121,4.37681733431002));
#58023=CARTESIAN_POINT('Ctrl Pts',(4.56488089129389,0.0741790848482271,
4.4152866170047));
#58024=CARTESIAN_POINT('Ctrl Pts',(4.57311643727954,0.0024660981813593,
4.41591041828323));
#58025=CARTESIAN_POINT('Ctrl Pts',(4.5733993439214,2.60627797130011E-6,
4.4159095790646));
#58026=CARTESIAN_POINT('Origin',(4.,0.,4.));
#58027=CARTESIAN_POINT('',(4.,-7.34788079488412E-17,4.6));
#58028=CARTESIAN_POINT('Origin',(4.,0.,4.));
#58029=CARTESIAN_POINT('',(4.,-0.219892372742957,4.3529863453938));
#58030=CARTESIAN_POINT('Ctrl Pts',(4.,-0.219914231356238,4.35301468169996));
#58031=CARTESIAN_POINT('Ctrl Pts',(4.,-0.219843051329574,4.3531167999744));
#58032=CARTESIAN_POINT('Ctrl Pts',(4.,-0.219771822781512,4.35321888245988));
#58033=CARTESIAN_POINT('Ctrl Pts',(4.,-0.21970054575756,4.3533209291203));
#58034=CARTESIAN_POINT('Ctrl Pts',(4.,-0.207925336055227,4.3701793886806));
#58035=CARTESIAN_POINT('Ctrl Pts',(4.,-0.194831304039315,4.38605734350833));
#58036=CARTESIAN_POINT('Ctrl Pts',(4.,-0.18064579384139,4.40088380688851));
#58037=CARTESIAN_POINT('Ctrl Pts',(4.,-0.168975273508986,4.41308164397169));
#58038=CARTESIAN_POINT('Ctrl Pts',(4.,-0.156565051628872,4.42456888924957));
#58039=CARTESIAN_POINT('Ctrl Pts',(4.,-0.143515931303371,4.43531683418355));
#58040=CARTESIAN_POINT('Ctrl Pts',(4.,-0.133182439541062,4.44382804395605));
#58041=CARTESIAN_POINT('Ctrl Pts',(4.,-0.122447811630206,4.45187590303098));
#58042=CARTESIAN_POINT('Ctrl Pts',(4.,-0.111352162047151,4.45944712768208));
#58043=CARTESIAN_POINT('Ctrl Pts',(4.,-0.105068105051177,4.46373511522897));
#58044=CARTESIAN_POINT('Ctrl Pts',(4.,-0.0986661212125077,4.46787107983396));
#58045=CARTESIAN_POINT('Ctrl Pts',(4.,-0.0921733602714696,4.47184061613108));
#58046=CARTESIAN_POINT('Ctrl Pts',(4.,-0.0718171345235072,4.48428598070136));
#58047=CARTESIAN_POINT('Ctrl Pts',(4.,-0.0505350523745213,4.49512244469223));
#58048=CARTESIAN_POINT('Ctrl Pts',(4.,-0.0285775088988711,4.50429938857761));
#58049=CARTESIAN_POINT('Ctrl Pts',(4.,-0.00645956782426854,4.51354336909515));
#58050=CARTESIAN_POINT('Ctrl Pts',(4.,0.0163444141029789,4.52110543571878));
#58051=CARTESIAN_POINT('Ctrl Pts',(4.,0.0396343143342583,4.52702898180467));
#58052=CARTESIAN_POINT('Ctrl Pts',(4.,0.0479455316904685,4.52914285427945));
#58053=CARTESIAN_POINT('Ctrl Pts',(4.,0.0563191235587283,4.53104786585874));
#58054=CARTESIAN_POINT('Ctrl Pts',(4.,0.0647475081636451,4.53274519105122));
#58055=CARTESIAN_POINT('Ctrl Pts',(4.,0.0709442475001029,4.53399310299165));
#58056=CARTESIAN_POINT('Ctrl Pts',(4.,0.0771669940275102,4.53512789739638));
#58057=CARTESIAN_POINT('Ctrl Pts',(4.,0.0834037601527001,4.53614909266968));
#58058=CARTESIAN_POINT('Ctrl Pts',(4.,0.108500755516298,4.54025842313435));
#58059=CARTESIAN_POINT('Ctrl Pts',(4.,0.133859781029961,4.54253781872753));
#58060=CARTESIAN_POINT('Ctrl Pts',(3.99999999999999,0.159256593756596,4.54305292380224));
#58061=CARTESIAN_POINT('Ctrl Pts',(3.99999999999999,0.185497795908202,4.5435851550133));
#58062=CARTESIAN_POINT('Ctrl Pts',(3.99999999999998,0.211780221987087,4.54223483664603));
#58063=CARTESIAN_POINT('Ctrl Pts',(3.99999999999998,0.237902321580844,4.5390442708621));
#58064=CARTESIAN_POINT('Ctrl Pts',(3.99999999999998,0.243507595489062,4.53835964001621));
#58065=CARTESIAN_POINT('Ctrl Pts',(3.99999999999998,0.249105619801251,4.53759013757336));
#58066=CARTESIAN_POINT('Ctrl Pts',(3.99999999999998,0.254694598474614,4.53673594206822));
#58067=CARTESIAN_POINT('',(4.,-0.219892372743086,3.64701365460628));
#58068=CARTESIAN_POINT('Ctrl Pts',(4.,0.254721014554616,3.46322028700966));
#58069=CARTESIAN_POINT('Ctrl Pts',(4.,0.254552373521139,3.46319452321125));
#58070=CARTESIAN_POINT('Ctrl Pts',(4.,0.254383724765285,3.46316883668624));
#58071=CARTESIAN_POINT('Ctrl Pts',(4.,0.254215068323085,3.46314322746093));
#58072=CARTESIAN_POINT('Ctrl Pts',(4.,0.228435861761457,3.4592288468388));
#58073=CARTESIAN_POINT('Ctrl Pts',(4.,0.202474691352968,3.45711700011808));
#58074=CARTESIAN_POINT('Ctrl Pts',(4.,0.176517231963435,3.45683380906617));
#58075=CARTESIAN_POINT('Ctrl Pts',(4.,0.151199179447316,3.45655759382427));
#58076=CARTESIAN_POINT('Ctrl Pts',(4.,0.125883695414598,3.45802192769867));
#58077=CARTESIAN_POINT('Ctrl Pts',(4.,0.1007794950383,3.46128259448669));
#58078=CARTESIAN_POINT('Ctrl Pts',(4.,0.0854593772715275,3.46327245269535));
#58079=CARTESIAN_POINT('Ctrl Pts',(4.,0.0702187270328167,3.46593187194604));
#58080=CARTESIAN_POINT('Ctrl Pts',(4.,0.0551140352340102,3.4692772918897));
#58081=CARTESIAN_POINT('Ctrl Pts',(4.,0.0468842919617017,3.47110003330284));
#58082=CARTESIAN_POINT('Ctrl Pts',(4.,0.0386923719445779,3.47312744960567));
#58083=CARTESIAN_POINT('Ctrl Pts',(4.,0.0305707631998946,3.47535548770785));
#58084=CARTESIAN_POINT('Ctrl Pts',(4.,0.0102648423897012,3.48092610391051));
#58085=CARTESIAN_POINT('Ctrl Pts',(4.,-0.00963556638195036,3.48775588581666));
#58086=CARTESIAN_POINT('Ctrl Pts',(4.,-0.0289965775380143,3.49587186612014));
#58087=CARTESIAN_POINT('Ctrl Pts',(4.,-0.047965755796229,3.50382359322137));
#58088=CARTESIAN_POINT('Ctrl Pts',(4.,-0.0664174073931304,3.51301096346156));
#58089=CARTESIAN_POINT('Ctrl Pts',(4.,-0.0841982143338667,3.52340033683134));
#58090=CARTESIAN_POINT('Ctrl Pts',(4.,-0.0930898199841631,3.5285957259532));
#58091=CARTESIAN_POINT('Ctrl Pts',(4.,-0.101813128894432,3.53409169793663));
#58092=CARTESIAN_POINT('Ctrl Pts',(4.,-0.110345561972859,3.53988353361915));
#58093=CARTESIAN_POINT('Ctrl Pts',(4.,-0.11586100642067,3.5436274303089));
#58094=CARTESIAN_POINT('Ctrl Pts',(4.,-0.121288652521606,3.54748953413154));
#58095=CARTESIAN_POINT('Ctrl Pts',(4.,-0.126621987542688,3.55146681430013));
#58096=CARTESIAN_POINT('Ctrl Pts',(4.,-0.143297831161627,3.56390265451229));
#58097=CARTESIAN_POINT('Ctrl Pts',(4.,-0.159061930875806,3.57746928852925));
#58098=CARTESIAN_POINT('Ctrl Pts',(4.,-0.173743808224101,3.59211536896244));
#58099=CARTESIAN_POINT('Ctrl Pts',(4.,-0.187864697165731,3.60620182877415));
#58100=CARTESIAN_POINT('Ctrl Pts',(4.,-0.200984288190684,3.62128798311348));
#58101=CARTESIAN_POINT('Ctrl Pts',(4.,-0.212904831975564,3.63731335989365));
#58102=CARTESIAN_POINT('Ctrl Pts',(4.,-0.21528245268753,3.64050971304978));
#58103=CARTESIAN_POINT('Ctrl Pts',(4.,-0.217612227418936,3.64374335030505));
#58104=CARTESIAN_POINT('Ctrl Pts',(4.,-0.219892372743211,3.64701365460636));
#58105=CARTESIAN_POINT('Origin',(4.,0.,4.));
#58106=CARTESIAN_POINT('Origin',(2.,0.,4.));
#58107=CARTESIAN_POINT('',(2.,-7.34788079488412E-17,4.6));
#58108=CARTESIAN_POINT('',(2.,-7.34788079488412E-17,4.6));
#58109=CARTESIAN_POINT('Origin',(2.,0.,4.));
#58110=CARTESIAN_POINT('Origin',(2.,0.,4.));
#58111=CARTESIAN_POINT('Ctrl Pts',(3.95224475517895,0.178288362465424,4.37571967666652));
#58112=CARTESIAN_POINT('Ctrl Pts',(3.96019739452275,0.115708609995841,4.40541533085819));
#58113=CARTESIAN_POINT('Ctrl Pts',(3.97610267321037,-0.0245105356436035,
4.43290545314371));
#58114=CARTESIAN_POINT('Ctrl Pts',(3.99996059124178,-0.228962993402626,
4.36819499612132));
#58115=CARTESIAN_POINT('Ctrl Pts',(4.0238185092732,-0.377374743411151,4.21349068386271));
#58116=CARTESIAN_POINT('Ctrl Pts',(4.04767642730463,-0.433534992178268,
4.00656196868444));
#58117=CARTESIAN_POINT('Ctrl Pts',(4.07153434533603,-0.383670022685343,
3.79803920418254));
#58118=CARTESIAN_POINT('Ctrl Pts',(4.09539226336747,-0.239994733226421,
3.63889579340969));
#58119=CARTESIAN_POINT('Ctrl Pts',(4.11925018139887,-0.0376302499649443,
3.56805514133307));
#58120=CARTESIAN_POINT('Ctrl Pts',(4.1431080994303,0.173933765839147,3.60283521426327));
#58121=CARTESIAN_POINT('Ctrl Pts',(4.16696601746172,0.342967344134064,3.73473372141871));
#58122=CARTESIAN_POINT('Ctrl Pts',(4.19082393549313,0.428135478754777,3.93149662217858));
#58123=CARTESIAN_POINT('Ctrl Pts',(4.21468185352456,0.40861313688017,4.1450106963618));
#58124=CARTESIAN_POINT('Ctrl Pts',(4.23853977155597,0.289173588337559,4.32306558264197));
#58125=CARTESIAN_POINT('Ctrl Pts',(4.2623976895874,0.0990233075312312,4.42212219878201));
#58126=CARTESIAN_POINT('Ctrl Pts',(4.28625560761881,-0.115340915390822,
4.41795840454656));
#58127=CARTESIAN_POINT('Ctrl Pts',(4.31011352565024,-0.301501118270308,
4.3115924136571));
#58128=CARTESIAN_POINT('Ctrl Pts',(4.33397144368164,-0.413936097932681,
4.12903358037428));
#58129=CARTESIAN_POINT('Ctrl Pts',(4.35782936171308,-0.425152419412173,
3.91492252699502));
#58130=CARTESIAN_POINT('Ctrl Pts',(4.38168727974448,-0.332407397051365,
3.72161523052345));
#58131=CARTESIAN_POINT('Ctrl Pts',(4.40554519777592,-0.158379709595794,
3.5963805946708));
#58132=CARTESIAN_POINT('Ctrl Pts',(4.42940311580732,0.0543761300157755,
3.56984189703405));
#58133=CARTESIAN_POINT('Ctrl Pts',(4.45326103383876,0.25383552520097,3.64848857324589));
#58134=CARTESIAN_POINT('Ctrl Pts',(4.47711895187016,0.39122521984844,3.81308936806525));
#58135=CARTESIAN_POINT('Ctrl Pts',(4.50097686990159,0.432949691632991,4.02339490384879));
#58136=CARTESIAN_POINT('Ctrl Pts',(4.524834787933,0.368806170420464,4.22797974831721));
#58137=CARTESIAN_POINT('Ctrl Pts',(4.54869270596443,0.214479494504121,4.37681733431002));
#58138=CARTESIAN_POINT('Ctrl Pts',(4.57255062399584,0.00770673985495463,
4.4335128177492));
#58139=CARTESIAN_POINT('Ctrl Pts',(4.59640854202726,-0.200950522604244,
4.38420260860549));
#58140=CARTESIAN_POINT('Ctrl Pts',(4.62026646005868,-0.360469908510665,
4.24094439618412));
#58141=CARTESIAN_POINT('Ctrl Pts',(4.6441243780901,-0.431844582779732,4.03876871570463));
#58142=CARTESIAN_POINT('Ctrl Pts',(4.66798229612152,-0.397621493350665,
3.82711302819544));
#58143=CARTESIAN_POINT('Ctrl Pts',(4.69184021415294,-0.266169117804412,
3.65773291463971));
#58144=CARTESIAN_POINT('Ctrl Pts',(4.71569813218436,-0.0696311426542753,
3.57204642662242));
#58145=CARTESIAN_POINT('Ctrl Pts',(4.73955605021577,0.143933543589337,3.59100624451743));
#58146=CARTESIAN_POINT('Ctrl Pts',(4.76341396824719,0.322302557754209,3.70997617639404));
#58147=CARTESIAN_POINT('Ctrl Pts',(4.78727188627862,0.421859817202848,3.8998648332327));
#58148=CARTESIAN_POINT('Ctrl Pts',(4.81112980431003,0.41826086011465,4.11423926597311));
#58149=CARTESIAN_POINT('Ctrl Pts',(4.83498772234146,0.312385729531365,4.30067908636799));
#58150=CARTESIAN_POINT('Ctrl Pts',(4.85884564037287,0.130123778861223,4.41359467981201));
#58151=CARTESIAN_POINT('Ctrl Pts',(4.88270355840429,-0.0839569802410516,
4.42537510794913));
#58152=CARTESIAN_POINT('Ctrl Pts',(4.90656147643571,-0.277507970732168,
4.33313973520738));
#58153=CARTESIAN_POINT('Ctrl Pts',(4.93041939446713,-0.403200703213916,
4.15944262266324));
#58154=CARTESIAN_POINT('Ctrl Pts',(4.95427731249855,-0.430299880793222,
3.94675744574809));
#58155=CARTESIAN_POINT('Ctrl Pts',(4.97813523052996,-0.352179016385168,
3.7470915236456));
#58156=CARTESIAN_POINT('Ctrl Pts',(5.00199314856139,-0.187940789307144,
3.60926861310034));
#58157=CARTESIAN_POINT('Ctrl Pts',(5.0258510665928,0.0222540801607904,3.56699016996131));
#58158=CARTESIAN_POINT('Ctrl Pts',(5.04970898462423,0.227007220840439,3.63059442521772));
#58159=CARTESIAN_POINT('Ctrl Pts',(5.07356690265564,0.376250912472057,3.7845284059142));
#58160=CARTESIAN_POINT('Ctrl Pts',(5.09742482068706,0.433491007135177,3.99115106069306));
#58161=CARTESIAN_POINT('Ctrl Pts',(5.12128273871848,0.384730742495793,4.19993752217271));
#58162=CARTESIAN_POINT('Ctrl Pts',(5.1451406567499,0.241893331461176,4.35983381329239));
#58163=CARTESIAN_POINT('Ctrl Pts',(5.16899857478132,0.0399064118422473,
4.43174093538579));
#58164=CARTESIAN_POINT('Ctrl Pts',(5.19285649281273,-0.171838712500945,
4.39807563839043));
#58165=CARTESIAN_POINT('Ctrl Pts',(5.21671441084416,-0.341564590845109,
4.26707000444592));
#58166=CARTESIAN_POINT('Ctrl Pts',(5.24057232887557,-0.427768622694993,
4.07075847957352));
#58167=CARTESIAN_POINT('Ctrl Pts',(5.264430246907,-0.409371574112622,3.85714457902312));
#58168=CARTESIAN_POINT('Ctrl Pts',(5.2882881649384,-0.290872024601924,3.6784627202051));
#58169=CARTESIAN_POINT('Ctrl Pts',(5.31214608296984,-0.101246341881189,
3.57840548479658));
#58170=CARTESIAN_POINT('Ctrl Pts',(5.33600400100125,0.113136829324483,3.58143959235932));
#58171=CARTESIAN_POINT('Ctrl Pts',(5.35986191903268,0.299854963974951,3.68682312094679));
#58172=CARTESIAN_POINT('Ctrl Pts',(5.38371983706408,0.413250392048343,3.8687869272297));
#58173=CARTESIAN_POINT('Ctrl Pts',(5.40757775509551,0.425594842551202,4.08283590397723));
#58174=CARTESIAN_POINT('Ctrl Pts',(5.43143567312693,0.333869761079625,4.27662924579771));
#58175=CARTESIAN_POINT('Ctrl Pts',(5.45529359115834,0.160504428594232,4.4027792017911));
#58176=CARTESIAN_POINT('Ctrl Pts',(5.47915150918977,-0.0521086087350157,
4.43043867146175));
#58177=CARTESIAN_POINT('Ctrl Pts',(5.50300942722118,-0.251979671819092,
4.35284416104532));
#58178=CARTESIAN_POINT('Ctrl Pts',(5.52686734525261,-0.390234841353927,
4.18896964197264));
#58179=CARTESIAN_POINT('Ctrl Pts',(5.55072526328402,-0.433066962396004,
3.97888689800548));
#58180=CARTESIAN_POINT('Ctrl Pts',(5.57458318131544,-0.370002414621403,
3.77396688259));
#58181=CARTESIAN_POINT('Ctrl Pts',(5.59844109934686,-0.21646219781534,3.62431812139094));
#58182=CARTESIAN_POINT('Ctrl Pts',(5.62229901737828,-0.00999107731853999,
3.56653381289738));
#58183=CARTESIAN_POINT('Ctrl Pts',(5.64615693540971,0.198923133709572,3.61474379450078));
#58184=CARTESIAN_POINT('Ctrl Pts',(5.67001485344111,0.359195220034686,3.75715941257656));
#58185=CARTESIAN_POINT('Ctrl Pts',(5.69387277147254,0.431634290692432,3.95895616900985));
#58186=CARTESIAN_POINT('Ctrl Pts',(5.71773068950395,0.398527019959163,4.1707892603438));
#58187=CARTESIAN_POINT('Ctrl Pts',(5.74158860753538,0.267969036875697,4.34085972491723));
#58188=CARTESIAN_POINT('Ctrl Pts',(5.76544652556679,0.0718853255354575,
4.42758070267197));
#58189=CARTESIAN_POINT('Ctrl Pts',(5.78930444359821,-0.141776307127955,
4.40974655013133));
#58190=CARTESIAN_POINT('Ctrl Pts',(5.81316236162963,-0.320769768688322,
4.29171820750724));
#58191=CARTESIAN_POINT('Ctrl Pts',(5.83702027966105,-0.421326288178809,
4.10235681181338));
#58192=CARTESIAN_POINT('Ctrl Pts',(5.86087819769247,-0.418857046020503,
3.88796639709818));
#58193=CARTESIAN_POINT('Ctrl Pts',(5.88473611572389,-0.313965860818636,
3.70097123187977));
#58194=CARTESIAN_POINT('Ctrl Pts',(5.90859403375531,-0.132301443679057,
3.58709678011166));
#58195=CARTESIAN_POINT('Ctrl Pts',(5.93245195178673,0.0817142298265842,
3.57418834816524));
#58196=CARTESIAN_POINT('Ctrl Pts',(5.95630986981814,0.275748643515392,3.66540258613358));
#58197=CARTESIAN_POINT('Ctrl Pts',(5.98016778784957,0.402354822815078,3.83843477537114));
#58198=CARTESIAN_POINT('Ctrl Pts',(6.00402570588098,0.430574627524036,4.05097449853386));
#58199=CARTESIAN_POINT('Ctrl Pts',(6.02788362391241,0.353506566116634,4.25104874587108));
#58200=CARTESIAN_POINT('Ctrl Pts',(6.05174154194382,0.189997730437525,4.38973628930191));
#58201=CARTESIAN_POINT('Ctrl Pts',(6.07559945997525,-0.0199730113800777,
4.43311976162365));
#58202=CARTESIAN_POINT('Ctrl Pts',(6.09945737800665,-0.2250554921608,4.3705991908187));
#58203=CARTESIAN_POINT('Ctrl Pts',(6.12331529603809,-0.375113923638194,
4.21744656883549));
#58204=CARTESIAN_POINT('Ctrl Pts',(6.1471732140695,-0.433431396087355,4.01114207710762));
#58205=CARTESIAN_POINT('Ctrl Pts',(6.17103113210093,-0.385792139046387,
3.80207577201042));
#58206=CARTESIAN_POINT('Ctrl Pts',(6.19488905013233,-0.243761337718234,
3.64147770828707));
#58207=CARTESIAN_POINT('Ctrl Pts',(6.21874696816376,-0.042227823444436,
3.56841523311022));
#58208=CARTESIAN_POINT('Ctrl Pts',(6.24260488619517,0.16982704650124,3.60113783246665));
#58209=CARTESIAN_POINT('Ctrl Pts',(6.2664628042266,0.339985970990829,3.73091992247201));
#58210=CARTESIAN_POINT('Ctrl Pts',(6.29032072225801,0.427700638223926,3.92738904240251));
#58211=CARTESIAN_POINT('Ctrl Pts',(6.31417864028943,0.409561128158778,4.13996490148311));
#58212=CARTESIAN_POINT('Ctrl Pts',(6.34598919766466,0.254661277208374,4.38159318714805));
#58213=CARTESIAN_POINT('Ctrl Pts',(6.38575239438369,-0.125272905304917,
4.47558432627151));
#58214=CARTESIAN_POINT('Ctrl Pts',(6.43346823044653,-0.468271923807345,
4.15124960425567));
#58215=CARTESIAN_POINT('Ctrl Pts',(6.48118406650937,-0.380227249479543,
3.6882349865083));
#58216=CARTESIAN_POINT('Ctrl Pts',(6.52889990257221,0.0564566449812287,
3.51140415777354));
#58217=CARTESIAN_POINT('Ctrl Pts',(6.57661573863504,0.441574375138847,3.78331933667001));
#58218=CARTESIAN_POINT('Ctrl Pts',(6.62433157469789,0.421040068198854,4.25418342072721));
#58219=CARTESIAN_POINT('Ctrl Pts',(6.67204741076071,0.0139362792425842,
4.49164405688148));
#58220=CARTESIAN_POINT('Ctrl Pts',(6.71976324682356,-0.406006764042365,
4.27761133505345));
#58221=CARTESIAN_POINT('Ctrl Pts',(6.76747908288639,-0.453085647428837,
3.80864864857145));
#58222=CARTESIAN_POINT('Ctrl Pts',(6.81519491894923,-0.0841006081168706,
3.51540431248109));
#58223=CARTESIAN_POINT('Ctrl Pts',(6.86291075501207,0.362121456530253,3.66717299786736));
#58224=CARTESIAN_POINT('Ctrl Pts',(6.91062659107491,0.475798562415156,4.124581128109));
#58225=CARTESIAN_POINT('Ctrl Pts',(6.95834242713775,0.152544250279933,4.46758486877347));
#58226=CARTESIAN_POINT('Ctrl Pts',(7.00605826320058,-0.310794706562241,
4.38119802990972));
#58227=CARTESIAN_POINT('Ctrl Pts',(7.05377409926342,-0.488725618924084,
3.94475128051735));
#58228=CARTESIAN_POINT('Ctrl Pts',(7.10148993532626,-0.21785253135038,3.55904022429238));
#58229=CARTESIAN_POINT('Ctrl Pts',(7.14920577138909,0.253078023397415,3.57826934481931));
#58230=CARTESIAN_POINT('Ctrl Pts',(7.19692160745195,0.491603063369337,3.98478019943955));
#58231=CARTESIAN_POINT('Ctrl Pts',(7.24463744351477,0.278681483980911,4.40526763942622));
#58232=CARTESIAN_POINT('Ctrl Pts',(7.29235327957762,-0.190157610347023,
4.45359156587464));
#58233=CARTESIAN_POINT('Ctrl Pts',(7.34006911564044,-0.484372034479295,
4.08537538031203));
#58234=CARTESIAN_POINT('Ctrl Pts',(7.3877849517033,-0.333780171974684,3.63875766810317));
#58235=CARTESIAN_POINT('Ctrl Pts',(7.43550078776612,0.123327161313159,3.52387434835784));
#58236=CARTESIAN_POINT('Ctrl Pts',(7.48321662382897,0.467181263150904,3.84622454030349));
#58237=CARTESIAN_POINT('Ctrl Pts',(7.5309324598918,0.382015623368301,4.30978910321172));
#58238=CARTESIAN_POINT('Ctrl Pts',(7.57864829595465,-0.0539608418635878,
4.4888695658253));
#58239=CARTESIAN_POINT('Ctrl Pts',(7.62636413201748,-0.440384235482588,
4.21901358396786));
#58240=CARTESIAN_POINT('Ctrl Pts',(7.67407996808031,-0.422396009600076,
3.7480340579683));
#58241=CARTESIAN_POINT('Ctrl Pts',(7.72179580414317,-0.0165150286377962,
3.50843873354525));
#58242=CARTESIAN_POINT('Ctrl Pts',(7.76951164020598,0.404531957204003,3.72025168374225));
#58243=CARTESIAN_POINT('Ctrl Pts',(7.81722747626884,0.454091022239626,4.18896181724392));
#58244=CARTESIAN_POINT('Ctrl Pts',(7.86494331233166,0.0866513144543145,
4.48414540641706));
#58245=CARTESIAN_POINT('Ctrl Pts',(7.91265914839452,-0.360361628691054,
4.33473081934393));
#58246=CARTESIAN_POINT('Ctrl Pts',(7.96037498445733,-0.476448943335793,
3.87792777037096));
#58247=CARTESIAN_POINT('Ctrl Pts',(8.0080908205202,-0.1550058622045,3.53322552818936));
#58248=CARTESIAN_POINT('Ctrl Pts',(8.05580665658301,0.308781487260178,3.61716946571973));
#58249=CARTESIAN_POINT('Ctrl Pts',(8.10352249264587,0.489010045760349,4.0526725734847));
#58250=CARTESIAN_POINT('Ctrl Pts',(8.1512383287087,0.220173154851853,4.43980564654689));
#58251=CARTESIAN_POINT('Ctrl Pts',(8.19895416477154,-0.250852131956433,
4.4230584271054));
#58252=CARTESIAN_POINT('Ctrl Pts',(8.24667000083438,-0.491516046133,4.01781014446235));
#58253=CARTESIAN_POINT('Ctrl Pts',(8.29438583689722,-0.280813212199106,
3.59620653211525));
#58254=CARTESIAN_POINT('Ctrl Pts',(8.34210167296004,0.187764715363875,3.54541267448783));
#58255=CARTESIAN_POINT('Ctrl Pts',(8.38981750902289,0.483915415676709,3.91207335260334));
#58256=CARTESIAN_POINT('Ctrl Pts',(8.43753334508573,0.335679143777854,4.35947842394856));
#58257=CARTESIAN_POINT('Ctrl Pts',(8.48524918114857,-0.120816450939738,
4.4767689272953));
#58258=CARTESIAN_POINT('Ctrl Pts',(8.5329650172114,-0.466364439759318,4.15623518867385));
#58259=CARTESIAN_POINT('Ctrl Pts',(8.58068085327425,-0.383642787608637,
3.69222827230584));
#58260=CARTESIAN_POINT('Ctrl Pts',(8.62839668933707,0.0513839395061145,
3.51085286915611));
#58261=CARTESIAN_POINT('Ctrl Pts',(8.67611252539993,0.439224004328866,3.77866880275638));
#58262=CARTESIAN_POINT('Ctrl Pts',(8.72382836146275,0.42371790764641,4.24973658040369));
#58263=CARTESIAN_POINT('Ctrl Pts',(8.7715441975256,0.0191051366342138,4.49146741357506));
#58264=CARTESIAN_POINT('Ctrl Pts',(8.81926003358843,-0.403052175319494,
4.28187615866228));
#58265=CARTESIAN_POINT('Ctrl Pts',(8.86697586965126,-0.455080472922433,
3.81343369002772));
#58266=CARTESIAN_POINT('Ctrl Pts',(8.91469170571412,-0.0892013699275644,
3.51631793453238));
#58267=CARTESIAN_POINT('Ctrl Pts',(8.96240754177693,0.358592723611288,3.66337486216116));
#58268=CARTESIAN_POINT('Ctrl Pts',(9.0101233778398,0.477085601399612,4.11955983351088));
#58269=CARTESIAN_POINT('Ctrl Pts',(9.05783921390261,0.157463430517111,4.46595117008304));
#58270=CARTESIAN_POINT('Ctrl Pts',(9.10555504996547,-0.306759831495564,
4.38445237758765));
#58271=CARTESIAN_POINT('Ctrl Pts',(9.1532708860283,-0.489280820139143,3.94990505119329));
#58272=CARTESIAN_POINT('Ctrl Pts',(9.20098672209113,-0.222487703095825,
3.56136068709803));
#58273=CARTESIAN_POINT('Ctrl Pts',(9.24870255815399,0.248619295113741,3.57562555337399));
#58274=CARTESIAN_POINT('Ctrl Pts',(9.29641839421681,0.49141536912078,3.97960000382683));
#58275=CARTESIAN_POINT('Ctrl Pts',(9.34413423027966,0.282937148266828,4.40230808465976));
#58276=CARTESIAN_POINT('Ctrl Pts',(9.39185006634249,-0.185366609388173,
4.45557046104408));
#58277=CARTESIAN_POINT('Ctrl Pts',(9.43956590240532,-0.483445357410111,
4.09047547319903));
#58278=CARTESIAN_POINT('Ctrl Pts',(9.48728173846818,-0.337568794959357,
3.64229546617122));
#58279=CARTESIAN_POINT('Ctrl Pts',(9.53499757453099,0.118302386066128,3.5226010365501));
#58280=CARTESIAN_POINT('Ctrl Pts',(9.58271341059386,0.465534665650901,3.84130942079228));
#58281=CARTESIAN_POINT('Ctrl Pts',(9.63042924665667,0.385259298596883,4.30574580568933));
#58282=CARTESIAN_POINT('Ctrl Pts',(9.67814508271952,-0.0488056103349303,
4.48941111271794));
#58283=CARTESIAN_POINT('Ctrl Pts',(9.72586091878235,-0.438051576325333,
4.22364266437974));
#58284=CARTESIAN_POINT('Ctrl Pts',(9.77357675484519,-0.425028039486299,
3.75249971615691));
#58285=CARTESIAN_POINT('Ctrl Pts',(9.82129259090803,-0.0216947140899849,
3.50864008686857));
#58286=CARTESIAN_POINT('Ctrl Pts',(9.86900842697087,0.401561201071248,3.7160038263529));
#58287=CARTESIAN_POINT('Ctrl Pts',(9.91672426303371,0.456057286475463,4.18416562194019));
#58288=CARTESIAN_POINT('Ctrl Pts',(9.96444009909655,0.0917489483659128,
4.48320529314746));
#58289=CARTESIAN_POINT('Ctrl Pts',(10.0121559351594,-0.356813860767086,
4.3385101085883));
#58290=CARTESIAN_POINT('Ctrl Pts',(10.0598717712222,-0.477709011270712,
3.88295588266498));
#58291=CARTESIAN_POINT('Ctrl Pts',(10.1075876072851,-0.159916626226494,
3.53488507064564));
#58292=CARTESIAN_POINT('Ctrl Pts',(10.1553034433479,0.304729657315094,3.61393645496551));
#58293=CARTESIAN_POINT('Ctrl Pts',(10.2030192794107,0.489538007675758,4.04751593304174));
#58294=CARTESIAN_POINT('Ctrl Pts',(10.2507351154736,0.224796073077312,4.43746079867915));
#58295=CARTESIAN_POINT('Ctrl Pts',(10.2984509515364,-0.246379554360218,
4.42567868168988));
#58296=CARTESIAN_POINT('Ctrl Pts',(10.3461667875993,-0.491301045992024,
4.02298928139638));
#58297=CARTESIAN_POINT('Ctrl Pts',(10.3938826236621,-0.285053227451061,
3.599188470261));
#58298=CARTESIAN_POINT('Ctrl Pts',(10.4415984597249,0.182963355965895,3.54345905416307));
#58299=CARTESIAN_POINT('Ctrl Pts',(10.4893142957878,0.482961874346273,3.9069782134126));
#58300=CARTESIAN_POINT('Ctrl Pts',(10.5370301318506,0.339449072190825,4.35592071060949));
#58301=CARTESIAN_POINT('Ctrl Pts',(10.5847459679134,-0.115785036052801,
4.47801574270962));
#58302=CARTESIAN_POINT('Ctrl Pts',(10.6324618039763,-0.464691964107356,
4.16114156306187));
#58303=CARTESIAN_POINT('Ctrl Pts',(10.6801776400391,-0.386865111317189,
3.69628860657276));
#58304=CARTESIAN_POINT('Ctrl Pts',(10.7278934761019,0.0462259258804368,
3.51033849586834));
#58305=CARTESIAN_POINT('Ctrl Pts',(10.7756093121648,0.436866984064762,3.77405207881873));
#58306=CARTESIAN_POINT('Ctrl Pts',(10.8233251482276,0.426326368719826,4.24525711444552));
#58307=CARTESIAN_POINT('Ctrl Pts',(10.8710409842905,0.0242836891050981,
4.49123876811122));
#58308=CARTESIAN_POINT('Ctrl Pts',(10.9187568203533,-0.400059075867425,
4.28610830234036));
#58309=CARTESIAN_POINT('Ctrl Pts',(10.9664726564161,-0.45702143577077,3.81824018018824));
#58310=CARTESIAN_POINT('Ctrl Pts',(11.014188492479,-0.0942939790271268,
3.51728489730359));
#58311=CARTESIAN_POINT('Ctrl Pts',(11.0619043285418,0.355025089556487,3.65961432075161));
#58312=CARTESIAN_POINT('Ctrl Pts',(11.1096201646047,0.478319155637209,4.11452515096033));
#58313=CARTESIAN_POINT('Ctrl Pts',(11.1573360006675,0.16236538121005,4.46426577284621));
#58314=CARTESIAN_POINT('Ctrl Pts',(11.2050518367304,-0.302691021094817,
4.38766399188028));
#58315=CARTESIAN_POINT('Ctrl Pts',(11.2527676727932,-0.489781601228288,
3.95506440219344));
#58316=CARTESIAN_POINT('Ctrl Pts',(11.300483508856,-0.227098200695192,3.56372986339542));
#58317=CARTESIAN_POINT('Ctrl Pts',(11.3481993449188,0.244132971891272,3.57302890392028));
#58318=CARTESIAN_POINT('Ctrl Pts',(11.3959151809817,0.491173079921361,3.97442207176994));
#58319=CARTESIAN_POINT('Ctrl Pts',(11.4436310170445,0.287161390990383,4.39930384468027));
#58320=CARTESIAN_POINT('Ctrl Pts',(11.4913468531074,-0.180555021833016,
4.45749875294131));
#58321=CARTESIAN_POINT('Ctrl Pts',(11.5390626891702,-0.482464979911041,
4.09556551685319));
#58322=CARTESIAN_POINT('Ctrl Pts',(11.586778525233,-0.341319923258817,3.64587299617429));
#58323=CARTESIAN_POINT('Ctrl Pts',(11.6344943612959,0.113264470804062,3.5213807520529));
#58324=CARTESIAN_POINT('Ctrl Pts',(11.6822101973587,0.463836358529674,3.83641192782507));
#58325=CARTESIAN_POINT('Ctrl Pts',(11.7299260334216,0.38846018117773,4.30166854740152));
#58326=CARTESIAN_POINT('Ctrl Pts',(11.7776418694844,-0.0436449577779122,
4.48989829813191));
#58327=CARTESIAN_POINT('Ctrl Pts',(11.8253577055472,-0.435670260442099,
4.22824690363353));
#58328=CARTESIAN_POINT('Ctrl Pts',(11.8730735416101,-0.427612859293677,
3.75699286549843));
#58329=CARTESIAN_POINT('Ctrl Pts',(11.9207893776729,-0.0268719897862959,
3.50889601812151));
#58330=CARTESIAN_POINT('Ctrl Pts',(11.9685052137357,0.398545841420554,3.71178751390968));
#58331=CARTESIAN_POINT('Ctrl Pts',(12.0162210497986,0.457972894034889,4.17934897039372));
#58332=CARTESIAN_POINT('Ctrl Pts',(12.0639368858614,0.0968363912382316,
4.48221150772657));
#58333=CARTESIAN_POINT('Ctrl Pts',(12.1116527219243,-0.353226459651896,
4.34225179773635));
#58334=CARTESIAN_POINT('Ctrl Pts',(12.1593685579871,-0.478916017555994,
3.88799699566402));
#58335=CARTESIAN_POINT('Ctrl Pts',(12.2070843940499,-0.164809627468288,
3.53659627586117));
#58336=CARTESIAN_POINT('Ctrl Pts',(12.2548002301128,0.300643979445627,3.61074632631782));
#58337=CARTESIAN_POINT('Ctrl Pts',(12.3025160661756,0.490011594032383,4.04235401475446));
#58338=CARTESIAN_POINT('Ctrl Pts',(12.3502319022385,0.229394022021679,4.43506735974179));
#58339=CARTESIAN_POINT('Ctrl Pts',(12.3979477383013,-0.241879610092261,
4.42825165390643));
#58340=CARTESIAN_POINT('Ctrl Pts',(12.4456635743641,-0.491031474462283,
4.0281658647901));
#58341=CARTESIAN_POINT('Ctrl Pts',(12.493379410427,-0.289261580343189,3.60221492864948));
#58342=CARTESIAN_POINT('Ctrl Pts',(12.5410952464898,0.178141673866572,3.54155614424011));
#58343=CARTESIAN_POINT('Ctrl Pts',(12.5888110825527,0.481954687902679,3.90189340664049));
#58344=CARTESIAN_POINT('Ctrl Pts',(12.6365269186155,0.343181296211668,4.35232346328687));
#58345=CARTESIAN_POINT('Ctrl Pts',(12.6842427546783,-0.110740760313508,
4.47920946240362));
#58346=CARTESIAN_POINT('Ctrl Pts',(12.7319585907412,-0.462967872677167,
4.16603003860975));
#58347=CARTESIAN_POINT('Ctrl Pts',(12.779674426804,-0.390044463885,3.70038267566003));
#58348=CARTESIAN_POINT('Ctrl Pts',(12.8273902628668,0.0410627776982723,
3.50987851185683));
#58349=CARTESIAN_POINT('Ctrl Pts',(12.8751060989297,0.434461438689172,3.76946045210395));
#58350=CARTESIAN_POINT('Ctrl Pts',(12.9228219349925,0.42888747548329,4.24075040649094));
#58351=CARTESIAN_POINT('Ctrl Pts',(12.9705377710553,0.0294595442590321,
4.49095555817611));
#58352=CARTESIAN_POINT('Ctrl Pts',(13.0182536071182,-0.397021539751646,
4.29030866646591));
#58353=CARTESIAN_POINT('Ctrl Pts',(13.065969443181,-0.458911634846768,3.82306685936703));
#58354=CARTESIAN_POINT('Ctrl Pts',(13.1136852792439,-0.0993761143989603,
3.51830547777773));
#58355=CARTESIAN_POINT('Ctrl Pts',(13.1614011153067,0.351418020999476,3.65589158776806));
#58356=CARTESIAN_POINT('Ctrl Pts',(13.2091169513695,0.479499580452807,4.10947774749948));
#58357=CARTESIAN_POINT('Ctrl Pts',(13.2568327874324,0.167249297126924,4.46252880717046));
#58358=CARTESIAN_POINT('Ctrl Pts',(13.3045486234952,-0.298588589211839,
4.39083254629632));
#58359=CARTESIAN_POINT('Ctrl Pts',(13.352264459558,-0.490227979701372,3.96022874442655));
#58360=CARTESIAN_POINT('Ctrl Pts',(13.3999802956209,-0.23168347330409,3.56614749850931));
#58361=CARTESIAN_POINT('Ctrl Pts',(13.4476961316837,0.239619531536799,3.57047968038978));
#58362=CARTESIAN_POINT('Ctrl Pts',(13.4954119677466,0.490876233547033,3.96924698078795));
#58363=CARTESIAN_POINT('Ctrl Pts',(13.5431278038094,0.291353737189313,4.39625525192456));
#58364=CARTESIAN_POINT('Ctrl Pts',(13.5908436398722,-0.175723379082843,
4.45937622804808));
#58365=CARTESIAN_POINT('Ctrl Pts',(13.6385594759351,-0.481431012491488,
4.10064494554323));
#58366=CARTESIAN_POINT('Ctrl Pts',(13.6862753119979,-0.345033139360895,
3.64948986092447));
#58367=CARTESIAN_POINT('Ctrl Pts',(13.7339911480608,0.108213974662067,3.52021363031051));
#58368=CARTESIAN_POINT('Ctrl Pts',(13.7817069841236,0.462086530666827,3.83153260544464));
#58369=CARTESIAN_POINT('Ctrl Pts',(13.8294228201864,0.391617915445045,4.297557781203));
#58370=CARTESIAN_POINT('Ctrl Pts',(13.8771386562493,-0.0384794573460961,
4.49033106796769));
#58371=CARTESIAN_POINT('Ctrl Pts',(13.9248544923121,-0.433240552373761,
4.23282579030437));
#58372=CARTESIAN_POINT('Ctrl Pts',(13.9725703283749,-0.430150181893835,
3.76151300691929));
#58373=CARTESIAN_POINT('Ctrl Pts',(14.0202861644378,-0.032046280669499,
3.50920649887429));
#58374=CARTESIAN_POINT('Ctrl Pts',(14.0680020005006,0.39548621318905,3.70760321474174));
#58375=CARTESIAN_POINT('Ctrl Pts',(14.1157178365634,0.459837632138507,4.1745123976147));
#58376=CARTESIAN_POINT('Ctrl Pts',(14.1634336726263,0.101913077983734,4.48116416053968));
#58377=CARTESIAN_POINT('Ctrl Pts',(14.2111495086891,-0.349599823817769,
4.34595547117883));
#58378=CARTESIAN_POINT('Ctrl Pts',(14.258865344752,-0.480069828122688,3.8930505494253));
#58379=CARTESIAN_POINT('Ctrl Pts',(14.3065811808148,-0.169684322438749,
3.53835895376334));
#58380=CARTESIAN_POINT('Ctrl Pts',(14.3542970168777,0.296524907469595,3.60759943412104));
#58381=CARTESIAN_POINT('Ctrl Pts',(14.4020128529405,0.49043075222644,4.0371873919842));
#58382=CARTESIAN_POINT('Ctrl Pts',(14.4497286890033,0.233966490966644,4.43262559558668));
#58383=CARTESIAN_POINT('Ctrl Pts',(14.4974445250662,-0.237352798985028,
4.43077705796148));
#58384=CARTESIAN_POINT('Ctrl Pts',(14.545160361129,-0.490707361486496,4.03333931965322));
#58385=CARTESIAN_POINT('Ctrl Pts',(14.5928761971918,-0.293437803431633,
3.60528557111603));
#58386=CARTESIAN_POINT('Ctrl Pts',(14.6405920332547,0.173300204635467,3.53970415608515));
#58387=CARTESIAN_POINT('Ctrl Pts',(14.6883078693175,0.480893968219416,3.89681949708321));
#58388=CARTESIAN_POINT('Ctrl Pts',(14.7360237053804,0.346875401282657,4.34868708154587));
#58389=CARTESIAN_POINT('Ctrl Pts',(14.7837395414432,-0.10568418401607,4.48034995378457));
#58390=CARTESIAN_POINT('Ctrl Pts',(14.831455377506,-0.461192356972643,4.17090007232882));
#58391=CARTESIAN_POINT('Ctrl Pts',(14.8791712135689,-0.393180492164677,
3.7045100248179));
#58392=CARTESIAN_POINT('Ctrl Pts',(14.9268870496317,0.0358950684576197,
3.50947296821438));
#58393=CARTESIAN_POINT('Ctrl Pts',(14.9746028856945,0.432007635398663,3.76489443262817));
#58394=CARTESIAN_POINT('Ctrl Pts',(15.0223187217574,0.431400943461215,4.23621695712364));
#58395=CARTESIAN_POINT('Ctrl Pts',(15.0700345578202,0.0346321271865876,
4.4906178152274));
#58396=CARTESIAN_POINT('Ctrl Pts',(15.1177503938831,-0.393939904367254,
4.2944767844824));
#58397=CARTESIAN_POINT('Ctrl Pts',(15.1654662299459,-0.46075086019608,3.82791319143947));
#58398=CARTESIAN_POINT('Ctrl Pts',(15.2131820660087,-0.104447211543591,
3.51937956259357));
#58399=CARTESIAN_POINT('Ctrl Pts',(15.2608979020716,0.347771918596306,3.652207076714));
#58400=CARTESIAN_POINT('Ctrl Pts',(15.3086137381344,0.480626744730421,4.10441818376995));
#58401=CARTESIAN_POINT('Ctrl Pts',(15.3563295741973,0.172114635785536,4.46074046598969));
#58402=CARTESIAN_POINT('Ctrl Pts',(15.4040454102601,-0.294452991525291,
4.39395768888776));
#58403=CARTESIAN_POINT('Ctrl Pts',(15.4517612463229,-0.490619905976795,
3.96539750426199));
#58404=CARTESIAN_POINT('Ctrl Pts',(15.4994770823858,-0.236243011612202,
3.56861332390027));
#58405=CARTESIAN_POINT('Ctrl Pts',(15.5471929184486,0.235079475381852,3.56797816593814));
#58406=CARTESIAN_POINT('Ctrl Pts',(15.5949087545115,0.490524862970081,3.9640753057054));
#58407=CARTESIAN_POINT('Ctrl Pts',(15.6426245905743,0.295513721197704,4.39316264501585));
#58408=CARTESIAN_POINT('Ctrl Pts',(15.6903404266371,-0.170872217813597,
4.46120267782338));
#58409=CARTESIAN_POINT('Ctrl Pts',(15.7380562626999,-0.480343569999647,
4.1057131950703));
#58410=CARTESIAN_POINT('Ctrl Pts',(15.7857720987628,-0.348708030819167,
3.6531456586776));
#58411=CARTESIAN_POINT('Ctrl Pts',(15.8334879348256,0.103151458625294,3.5190998009613));
#58412=CARTESIAN_POINT('Ctrl Pts',(15.8812037708885,0.460285376424935,3.82667199562295));
#58413=CARTESIAN_POINT('Ctrl Pts',(15.9289196069513,0.39473215065269,4.29341396369818));
#58414=CARTESIAN_POINT('Ctrl Pts',(15.9766354430142,-0.033309682798763,
4.49070937415524));
#58415=CARTESIAN_POINT('Ctrl Pts',(16.024351279077,-0.430762722000766,4.23737881579128));
#58416=CARTESIAN_POINT('Ctrl Pts',(16.0720671151398,-0.432639725453012,
3.76605963834362));
#58417=CARTESIAN_POINT('Ctrl Pts',(16.1197829512026,-0.0372170120039125,
3.50957149464017));
#58418=CARTESIAN_POINT('Ctrl Pts',(16.1674987872655,0.392382656225717,3.70345139362117));
#58419=CARTESIAN_POINT('Ctrl Pts',(16.2152146233283,0.461651293660056,4.16965644082667));
#58420=CARTESIAN_POINT('Ctrl Pts',(16.2629304593912,0.106978444708158,4.48006336792116));
#58421=CARTESIAN_POINT('Ctrl Pts',(16.310646295454,-0.345934356094203,4.34962071752925));
#58422=CARTESIAN_POINT('Ctrl Pts',(16.3583621315169,-0.481170314810987,
3.89811598262401));
#58423=CARTESIAN_POINT('Ctrl Pts',(16.4060779675797,-0.174540169679895,
3.54017290856226));
#58424=CARTESIAN_POINT('Ctrl Pts',(16.4537938036425,0.292372898913969,3.60449612791703));
#58425=CARTESIAN_POINT('Ctrl Pts',(16.5015096397054,0.490795435699827,4.0320166386149));
#58426=CARTESIAN_POINT('Ctrl Pts',(16.5492254757682,0.238512972024049,4.4301357774334));
#58427=CARTESIAN_POINT('Ctrl Pts',(16.596941311831,-0.23279962385521,4.43325461334514));
#58428=CARTESIAN_POINT('Ctrl Pts',(16.6446571478939,-0.490328743065594,
4.03850907134293));
#58429=CARTESIAN_POINT('Ctrl Pts',(16.6923729839567,-0.297581432841348,
3.60840005658827));
#58430=CARTESIAN_POINT('Ctrl Pts',(16.7400888200196,0.168439486040012,3.53790329540825));
#58431=CARTESIAN_POINT('Ctrl Pts',(16.7878046560824,0.479779833116189,3.89175704832657));
#58432=CARTESIAN_POINT('Ctrl Pts',(16.8355204921452,0.350530977080134,4.3450119692985));
#58433=CARTESIAN_POINT('Ctrl Pts',(16.8832363282081,-0.100615868820984,
4.4814370901721));
#58434=CARTESIAN_POINT('Ctrl Pts',(16.9309521642709,-0.459365614209645,
4.17575112327883));
#58435=CARTESIAN_POINT('Ctrl Pts',(16.9786680003337,-0.396272847821079,
3.70867019559999));
#58436=CARTESIAN_POINT('Ctrl Pts',(17.0263838363966,0.0307233721630972,
3.5091219099869));
#58437=CARTESIAN_POINT('Ctrl Pts',(17.0740996724594,0.429505846750062,3.76035452756312));
#58438=CARTESIAN_POINT('Ctrl Pts',(17.1218155085223,0.433866493469502,4.23165726989771));
#58439=CARTESIAN_POINT('Ctrl Pts',(17.1695313445851,0.039800863341802,4.49022557677993));
#58440=CARTESIAN_POINT('Ctrl Pts',(17.217247180648,-0.390814512007675,4.29861219341511));
#58441=CARTESIAN_POINT('Ctrl Pts',(17.2649630167107,-0.462538907526291,
3.83277863809798));
#58442=CARTESIAN_POINT('Ctrl Pts',(17.3126788527736,-0.109506707187599,
3.52050703244687));
#58443=CARTESIAN_POINT('Ctrl Pts',(17.3603946888365,0.344087187338735,3.64856119684745));
#58444=CARTESIAN_POINT('Ctrl Pts',(17.4081105248993,0.481700523269991,4.09934702176407));
#58445=CARTESIAN_POINT('Ctrl Pts',(17.4558263609621,0.176960856767158,4.45890094794434));
#58446=CARTESIAN_POINT('Ctrl Pts',(17.503542197025,-0.290284687397741,4.39703907252861));
#58447=CARTESIAN_POINT('Ctrl Pts',(17.5512580330878,-0.490957336521241,
3.97057010757845));
#58448=CARTESIAN_POINT('Ctrl Pts',(17.5989738691507,-0.240776309167652,
3.57112706567612));
#58449=CARTESIAN_POINT('Ctrl Pts',(17.6466897052135,0.230513307714322,3.56552463842171));
#58450=CARTESIAN_POINT('Ctrl Pts',(17.6944055412763,0.490119007219086,3.95890762096741));
#58451=CARTESIAN_POINT('Ctrl Pts',(17.7421213773392,0.299640880944266,4.39002636746625));
#58452=CARTESIAN_POINT('Ctrl Pts',(17.789837213402,-0.166002076869247,4.46297789939377));
#58453=CARTESIAN_POINT('Ctrl Pts',(17.8375530494648,-0.479202773223469,
4.11076970247734));
#58454=CARTESIAN_POINT('Ctrl Pts',(17.8852688855277,-0.352344189444135,
3.65683998336499));
#58455=CARTESIAN_POINT('Ctrl Pts',(17.9329847215905,0.0980774850139738,
3.51803938772416));
#58456=CARTESIAN_POINT('Ctrl Pts',(17.9807005576534,0.458433095867658,3.82183063825345));
#58457=CARTESIAN_POINT('Ctrl Pts',(18.0284163937162,0.397802540886209,4.28923755516265));
#58458=CARTESIAN_POINT('Ctrl Pts',(18.076132229779,-0.0281362083699241,
4.49103317467411));
#58459=CARTESIAN_POINT('Ctrl Pts',(18.1238480658419,-0.428237044548737,
4.24190547436581));
#58460=CARTESIAN_POINT('Ctrl Pts',(18.1715639019047,-0.435081213444543,
3.7706322547532));
#58461=CARTESIAN_POINT('Ctrl Pts',(18.2192797379675,-0.0423836094492617,
3.50999096487715));
#58462=CARTESIAN_POINT('Ctrl Pts',(18.2669955740304,0.389235515258945,3.69933251171255));
#58463=CARTESIAN_POINT('Ctrl Pts',(18.3147114100932,0.463413677146622,4.16478163940629));
#58464=CARTESIAN_POINT('Ctrl Pts',(18.3624272461561,0.112031928774586,4.4789092521418));
#58465=CARTESIAN_POINT('Ctrl Pts',(18.4101430822189,-0.342230463623947,
4.35324712966946));
#58466=CARTESIAN_POINT('Ctrl Pts',(18.4578589182817,-0.482217355384067,
3.90319273261591));
#58467=CARTESIAN_POINT('Ctrl Pts',(18.5055747543446,-0.179376629827252,
3.54203793877243));
#58468=CARTESIAN_POINT('Ctrl Pts',(18.5532905904074,0.288188414964166,3.60143675240633));
#58469=CARTESIAN_POINT('Ctrl Pts',(18.6010064264702,0.491105603945206,4.02684232898929));
#58470=CARTESIAN_POINT('Ctrl Pts',(18.6487222625331,0.243032960192409,4.42759818183915));
#58471=CARTESIAN_POINT('Ctrl Pts',(18.6964380985959,-0.228220590447982,
4.43568404486223));
#58472=CARTESIAN_POINT('Ctrl Pts',(18.7441539346588,-0.489895661254576,
4.0436745456279));
#58473=CARTESIAN_POINT('Ctrl Pts',(18.7918697707216,-0.301692008317894,
3.6115580391236));
#58474=CARTESIAN_POINT('Ctrl Pts',(18.8395856067845,0.163560057986223,3.53615376224111));
#58475=CARTESIAN_POINT('Ctrl Pts',(18.8873014428472,0.478612406344963,3.88670662268212));
#58476=CARTESIAN_POINT('Ctrl Pts',(18.9350172789101,0.35414761756175,4.34129853476112));
#58477=CARTESIAN_POINT('Ctrl Pts',(18.982733114973,-0.0955363776958117,
4.48247075080787));
#58478=CARTESIAN_POINT('Ctrl Pts',(19.0304489510358,-0.457487847288108,
4.18058265263639));
#58479=CARTESIAN_POINT('Ctrl Pts',(19.0781647870987,-0.399321187381313,
3.71286272589862));
#58480=CARTESIAN_POINT('Ctrl Pts',(19.1258806231614,0.0255482632835279,
3.50882537619781));
#58481=CARTESIAN_POINT('Ctrl Pts',(19.1735964592243,0.426956350589889,3.75584124112414));
#58482=CARTESIAN_POINT('Ctrl Pts',(19.2213122952871,0.436283851722622,4.22707185138688));
#58483=CARTESIAN_POINT('Ctrl Pts',(19.26902813135,0.0449651784623906,4.48977888620274));
#58484=CARTESIAN_POINT('Ctrl Pts',(19.3167439674128,-0.387645709555542,
4.3027144342981));
#58485=CARTESIAN_POINT('Ctrl Pts',(19.3644598034757,-0.464275578741542,
3.8376626582024));
#58486=CARTESIAN_POINT('Ctrl Pts',(19.4121756395385,-0.114554038379521,
3.52168776344319));
#58487=CARTESIAN_POINT('Ctrl Pts',(19.4598914756013,0.340364234683876,3.64495435060606));
#58488=CARTESIAN_POINT('Ctrl Pts',(19.5076073116642,0.482720800247919,4.09426482953845));
#58489=CARTESIAN_POINT('Ctrl Pts',(19.555323147727,0.181787415268628,4.45701044834135));
#58490=CARTESIAN_POINT('Ctrl Pts',(19.6030389837899,-0.28608412753634,4.40007637198121));
#58491=CARTESIAN_POINT('Ctrl Pts',(19.6507548198527,-0.491240257057309,
3.97574594767572));
#58492=CARTESIAN_POINT('Ctrl Pts',(19.6984706559155,-0.245282818621706,
3.57368850533185));
#58493=CARTESIAN_POINT('Ctrl Pts',(19.7461864919783,0.225921452997342,3.56311925573479));
#58494=CARTESIAN_POINT('Ctrl Pts',(19.7939023280412,0.489658867576397,3.95374471702426));
#58495=CARTESIAN_POINT('Ctrl Pts',(19.841618164104,0.303734463062876,4.38684635894002));
#58496=CARTESIAN_POINT('Ctrl Pts',(19.8893340001669,-0.161112940293692,
4.46470246728215));
#58497=CARTESIAN_POINT('Ctrl Pts',(19.9370498362297,-0.47800980043334,4.11581244897344));
#58498=CARTESIAN_POINT('Ctrl Pts',(19.9847656722926,-0.355939225796451,
3.66057517601247));
#58499=CARTESIAN_POINT('Ctrl Pts',(20.0324815083554,0.0929888682922082,
3.51702731322357));
#58500=CARTESIAN_POINT('Ctrl Pts',(20.0801973444182,0.456536973876988,3.81701888067549));
#58501=CARTESIAN_POINT('Ctrl Pts',(20.1279131804811,0.400815378068436,4.28501049648274));
#58502=CARTESIAN_POINT('Ctrl Pts',(20.1756290165439,-0.022934367574535,
4.49133741301101));
#58503=CARTESIAN_POINT('Ctrl Pts',(20.2233448526067,-0.425711472830213,
4.24633918020534));
#58504=CARTESIAN_POINT('Ctrl Pts',(20.2710606886696,-0.437384262562023,
3.77535541015343));
#58505=CARTESIAN_POINT('Ctrl Pts',(20.3187765247324,-0.0477164433392854,
3.51022640082505));
#58506=CARTESIAN_POINT('Ctrl Pts',(20.3664923607953,0.386374384143037,3.69571627142296));
#58507=CARTESIAN_POINT('Ctrl Pts',(20.4062555575143,0.45143962727185,4.08165775845481));
#58508=CARTESIAN_POINT('Ctrl Pts',(20.4380661148895,0.291471375703242,4.31996082336987));
#58509=CARTESIAN_POINT('Ctrl Pts',(20.461924032921,0.103697252552815,4.42124466395835));
#58510=CARTESIAN_POINT('Ctrl Pts',(20.4857819509523,-0.111451542568667,
4.41901444157942));
#58511=CARTESIAN_POINT('Ctrl Pts',(20.5096398689838,-0.298255971346869,
4.31460392554555));
#58512=CARTESIAN_POINT('Ctrl Pts',(20.5334977870152,-0.412709509332759,
4.13311446574462));
#58513=CARTESIAN_POINT('Ctrl Pts',(20.5573557050466,-0.425936384696969,
3.91915434697803));
#58514=CARTESIAN_POINT('Ctrl Pts',(20.581213623078,-0.335173342752607,3.72492109335083));
#58515=CARTESIAN_POINT('Ctrl Pts',(20.6050715411095,-0.162364888615448,
3.59797442377207));
#58516=CARTESIAN_POINT('Ctrl Pts',(20.6289294591408,0.0501004451364318,
3.56932214892951));
#58517=CARTESIAN_POINT('Ctrl Pts',(20.6527873771723,0.250339089241223,3.64598859455508));
#58518=CARTESIAN_POINT('Ctrl Pts',(20.6766452952037,0.389350172549011,3.80921715950176));
#58519=CARTESIAN_POINT('Ctrl Pts',(20.7005032132352,0.433161330121289,4.01909908002448));
#58520=CARTESIAN_POINT('Ctrl Pts',(20.7243611312665,0.371049143609512,4.22430982617278));
#58521=CARTESIAN_POINT('Ctrl Pts',(20.748219049298,0.218207240773441,4.37467120177868));
#58522=CARTESIAN_POINT('Ctrl Pts',(20.7720769673293,0.01200671405148,4.43341500212799));
#58523=CARTESIAN_POINT('Ctrl Pts',(20.7959348853608,-0.197129246586683,
4.38617716647524));
#58524=CARTESIAN_POINT('Ctrl Pts',(20.8197928033922,-0.358062019934396,
4.24450842127602));
#58525=CARTESIAN_POINT('Ctrl Pts',(20.8436507214237,-0.431438726014498,
4.04305074550709));
#58526=CARTESIAN_POINT('Ctrl Pts',(20.867508639455,-0.399316990859146,3.83106596928302));
#58527=CARTESIAN_POINT('Ctrl Pts',(20.8913665574865,-0.269551332195825,
3.66039017609669));
#58528=CARTESIAN_POINT('Ctrl Pts',(20.9152244755179,-0.0738730526583281,
3.57275822989076));
#58529=CARTESIAN_POINT('Ctrl Pts',(20.9390823935493,0.139869212314499,3.58959853735383));
#58530=CARTESIAN_POINT('Ctrl Pts',(20.9629403115807,0.319409638666883,3.70679317993256));
#58531=CARTESIAN_POINT('Ctrl Pts',(20.9867982296122,0.420845711130686,3.8956848776653));
#58532=CARTESIAN_POINT('Ctrl Pts',(21.0106561476436,0.419373541863394,4.11008446384341));
#58533=CARTESIAN_POINT('Ctrl Pts',(21.034514065675,0.315353119032788,4.29756540021079));
#58534=CARTESIAN_POINT('Ctrl Pts',(21.0583719837064,0.134220268060588,4.41228349058099));
#58535=CARTESIAN_POINT('Ctrl Pts',(21.0822299017379,-0.079733094278782,
4.42618703719455));
#58536=CARTESIAN_POINT('Ctrl Pts',(21.1060878197692,-0.274189543318984,
4.33587624407661));
#58537=CARTESIAN_POINT('Ctrl Pts',(21.1299457378007,-0.401599180171465,
4.16343456021562));
#58538=CARTESIAN_POINT('Ctrl Pts',(21.1538036558321,-0.430806878168669,
3.95102867450389));
#58539=CARTESIAN_POINT('Ctrl Pts',(21.1776615738635,-0.354670559489406,
3.75059761183336));
#58540=CARTESIAN_POINT('Ctrl Pts',(21.2015194918949,-0.191807627993766,
3.61115222665144));
#58541=CARTESIAN_POINT('Ctrl Pts',(21.2253774099264,0.0179574932869785,
3.56679071405539));
#58542=CARTESIAN_POINT('Ctrl Pts',(21.2492353279577,0.223331518303719,3.62836067225603));
#58543=CARTESIAN_POINT('Ctrl Pts',(21.2730932459892,0.374094903668402,3.78080656934254));
#58544=CARTESIAN_POINT('Ctrl Pts',(21.2969511640206,0.433381894944723,3.98685123093373));
#58545=CARTESIAN_POINT('Ctrl Pts',(21.320809082052,0.386695207821707,4.19611112472705));
#58546=CARTESIAN_POINT('Ctrl Pts',(21.3446670000834,0.245451009020076,4.35741650656472));
#58547=CARTESIAN_POINT('Ctrl Pts',(21.3685249181149,0.0441873525619181,
4.43132381671722));
#58548=CARTESIAN_POINT('Ctrl Pts',(21.3923828361462,-0.167881315237013,
4.39976070465745));
#58549=CARTESIAN_POINT('Ctrl Pts',(21.4162407541777,-0.338898428465248,
4.27044521104599));
#58550=CARTESIAN_POINT('Ctrl Pts',(21.4400986722091,-0.427045644525908,
4.07499849655415));
#58551=CARTESIAN_POINT('Ctrl Pts',(21.4639565902406,-0.410768568010174,
3.86121260673678));
#58552=CARTESIAN_POINT('Ctrl Pts',(21.4878145082719,-0.294047387504818,
3.68136401506497));
#58553=CARTESIAN_POINT('Ctrl Pts',(21.5116724263034,-0.105423611064507,
3.57943060117972));
#58554=CARTESIAN_POINT('Ctrl Pts',(21.5355303443348,0.108979109962582,3.58033786138646));
#58555=CARTESIAN_POINT('Ctrl Pts',(21.5593882623662,0.296733470072461,3.68386394585134));
#58556=CARTESIAN_POINT('Ctrl Pts',(21.5832461803976,0.411928413892185,3.86469390692879));
#58557=CARTESIAN_POINT('Ctrl Pts',(21.6071040984291,0.426395639810567,4.07860989342611));
#58558=CARTESIAN_POINT('Ctrl Pts',(21.6309620164605,0.33659751701124,4.27330361969026));
#58559=CARTESIAN_POINT('Ctrl Pts',(21.6548199344919,0.164492132570386,4.401167166299));
#58560=CARTESIAN_POINT('Ctrl Pts',(21.6786778525233,-0.0478360589596606,
4.43093441317345));
#58561=CARTESIAN_POINT('Ctrl Pts',(21.7025357705547,-0.248467031045983,
4.35532645760922));
#58562=CARTESIAN_POINT('Ctrl Pts',(21.7263936885861,-0.388341045935521,
4.1928315042612));
#58563=CARTESIAN_POINT('Ctrl Pts',(21.7502516066176,-0.433255096896122,
3.98318399549658));
#58564=CARTESIAN_POINT('Ctrl Pts',(21.774109524649,-0.372226475033738,3.77764845789182));
#58565=CARTESIAN_POINT('Ctrl Pts',(21.7979674426804,-0.220178340780001,
3.62648392906691));
#58566=CARTESIAN_POINT('Ctrl Pts',(21.8218253607118,-0.0142906046679706,
3.56665425395863));
#58567=CARTESIAN_POINT('Ctrl Pts',(21.8456832787432,0.195091573553633,3.61278941785858));
#58568=CARTESIAN_POINT('Ctrl Pts',(21.8695411967747,0.356768547853618,3.75360811649661));
#58569=CARTESIAN_POINT('Ctrl Pts',(21.8933991148061,0.431205894023261,3.95467634223136));
#58570=CARTESIAN_POINT('Ctrl Pts',(21.9172570328375,0.400201653291494,4.16682743688221));
#58571=CARTESIAN_POINT('Ctrl Pts',(21.941114950869,0.271337207055788,4.33818467892719));
#58572=CARTESIAN_POINT('Ctrl Pts',(21.9649728689003,0.0761234226178432,
4.4268465550088));
#58573=CARTESIAN_POINT('Ctrl Pts',(21.9888307869318,-0.137704612210607,
4.41113282132402));
#58574=CARTESIAN_POINT('Ctrl Pts',(22.0126887049632,-0.317860118355158,
4.29488591379237));
#58575=CARTESIAN_POINT('Ctrl Pts',(22.0365466229946,-0.420290167226249,
4.10653136780738));
#58576=CARTESIAN_POINT('Ctrl Pts',(22.060404541026,-0.419947821735935,3.89212700053744));
#58577=CARTESIAN_POINT('Ctrl Pts',(22.0842624590574,-0.316916794682727,
3.70410052003731));
#58578=CARTESIAN_POINT('Ctrl Pts',(22.1081203770888,-0.136390978688423,
3.58842952252864));
#58579=CARTESIAN_POINT('Ctrl Pts',(22.1319782951203,0.0774861468089536,
3.57339871771534));
#58580=CARTESIAN_POINT('Ctrl Pts',(22.1558362131517,0.27241579873489,3.66268354680831));
#58581=CARTESIAN_POINT('Ctrl Pts',(22.1796941311831,0.400732367405962,3.83445143701846));
#58582=CARTESIAN_POINT('Ctrl Pts',(22.2035520492145,0.431058956528623,4.04670046033727));
#58583=CARTESIAN_POINT('Ctrl Pts',(22.227409967246,0.355979888945518,4.24752994899471));
#58584=CARTESIAN_POINT('Ctrl Pts',(22.2512678852773,0.193854041863619,4.38783162256878));
#58585=CARTESIAN_POINT('Ctrl Pts',(22.2751258033088,-0.0156743990186396,
4.43329790005389));
#58586=CARTESIAN_POINT('Ctrl Pts',(22.2989837213402,-0.221370022215225,
4.37281103827166));
#58587=CARTESIAN_POINT('Ctrl Pts',(22.3228416393716,-0.372934645290675,
4.22116172228637));
#58588=CARTESIAN_POINT('Ctrl Pts',(22.346699557403,-0.43330658847365,4.01543234121164));
#58589=CARTESIAN_POINT('Ctrl Pts',(22.3705574754345,-0.387723268841402,
3.80592933171158));
#58590=CARTESIAN_POINT('Ctrl Pts',(22.3944153934659,-0.247331046528593,
3.64388188817752));
#58591=CARTESIAN_POINT('Ctrl Pts',(22.4182733114973,-0.0464596501027702,
3.56891502119853));
#58592=CARTESIAN_POINT('Ctrl Pts',(22.4421312295287,0.165772403721094,3.59936017830047));
#58593=CARTESIAN_POINT('Ctrl Pts',(22.4659891475602,0.337468575289321,3.7277726770023));
#58594=CARTESIAN_POINT('Ctrl Pts',(22.4898470655915,0.426644514167594,3.92275218663495));
#58595=CARTESIAN_POINT('Ctrl Pts',(22.513704983623,0.411494197867752,4.13662086224655));
#58596=CARTESIAN_POINT('Ctrl Pts',(22.5375629016544,0.295722435535401,4.31708206952049));
#58597=CARTESIAN_POINT('Ctrl Pts',(22.5614208196858,0.107638304484935,4.42000797176855));
#58598=CARTESIAN_POINT('Ctrl Pts',(22.5852787377172,-0.106765988085903,
4.42023067651324));
#58599=CARTESIAN_POINT('Ctrl Pts',(22.6091366557487,-0.295063722636797,
4.31769517074077));
#58600=CARTESIAN_POINT('Ctrl Pts',(22.6329945737801,-0.411209141905604,
4.13747522778479));
#58601=CARTESIAN_POINT('Ctrl Pts',(22.6568524918115,-0.426804986482714,
3.92363755172126));
#58602=CARTESIAN_POINT('Ctrl Pts',(22.6807104098429,-0.33803111495158,3.72847502015617));
#58603=CARTESIAN_POINT('Ctrl Pts',(22.7045683278743,-0.16660749730952,3.59970312177549));
#58604=CARTESIAN_POINT('Ctrl Pts',(22.7284262459057,0.0455714674079685,
3.56882345794434));
#58605=CARTESIAN_POINT('Ctrl Pts',(22.7522841639372,0.246577802732478,3.64336153500176));
#58606=CARTESIAN_POINT('Ctrl Pts',(22.7761420819686,0.387346815298129,3.80514019809748));
#58607=CARTESIAN_POINT('Ctrl Pts',(22.7920473606562,0.417963038852713,3.94471011778788));
#58608=CARTESIAN_POINT('Ctrl Pts',(22.8,0.415641328671541,4.01393920819689));
#58609=CARTESIAN_POINT('Ctrl Pts',(3.96816317011929,0.203757107801821,4.42939176513376));
#58610=CARTESIAN_POINT('Ctrl Pts',(3.9761158094631,0.132237748973037,4.46332948562603));
#58611=CARTESIAN_POINT('Ctrl Pts',(3.99202108815071,-0.0280119004087947,
4.49474661085258));
#58612=CARTESIAN_POINT('Ctrl Pts',(4.01587900618213,-0.261670681609628,
4.42079217330492));
#58613=CARTESIAN_POINT('Ctrl Pts',(4.03973692421355,-0.431283260509235,
4.24398813071681));
#58614=CARTESIAN_POINT('Ctrl Pts',(4.06359484224497,-0.495466080430727,
4.00749935521381));
#58615=CARTESIAN_POINT('Ctrl Pts',(4.08745276027639,-0.438477829352452,
3.76918881818141));
#58616=CARTESIAN_POINT('Ctrl Pts',(4.11131067830781,-0.274278321106756,
3.5873115455631));
#58617=CARTESIAN_POINT('Ctrl Pts',(4.13516859633923,-0.0430057845205295,
3.50635120590702));
#58618=CARTESIAN_POINT('Ctrl Pts',(4.15902651437064,0.198780450874126,3.54609966156282));
#58619=CARTESIAN_POINT('Ctrl Pts',(4.18288443240206,0.391960715466274,3.69684005745713));
#58620=CARTESIAN_POINT('Ctrl Pts',(4.20674235043348,0.489295238859844,3.92171081754005));
#58621=CARTESIAN_POINT('Ctrl Pts',(4.2306002684649,0.466984102771714,4.16572567991789));
#58622=CARTESIAN_POINT('Ctrl Pts',(4.25445818649632,0.330482445391075,4.36921595913043));
#58623=CARTESIAN_POINT('Ctrl Pts',(4.27831610452774,0.113168927396708,4.48242295331799));
#58624=CARTESIAN_POINT('Ctrl Pts',(4.30217402255916,-0.131817528672551,
4.47766435517297));
#58625=CARTESIAN_POINT('Ctrl Pts',(4.32603194059057,-0.344570980451485,
4.35610383169054));
#58626=CARTESIAN_POINT('Ctrl Pts',(4.349889858622,-0.473067456356951,4.14746621026076));
#58627=CARTESIAN_POINT('Ctrl Pts',(4.37374777665341,-0.485886045261059,
3.9027690893624));
#58628=CARTESIAN_POINT('Ctrl Pts',(4.39760569468484,-0.379892264971952,
3.68184757153936));
#58629=CARTESIAN_POINT('Ctrl Pts',(4.42146361271625,-0.181004475645389,
3.53872299041084));
#58630=CARTESIAN_POINT('Ctrl Pts',(4.44532153074767,0.0621438372772935,
3.50839320219298));
#58631=CARTESIAN_POINT('Ctrl Pts',(4.46917944877909,0.290096289836991,3.5982746675986));
#58632=CARTESIAN_POINT('Ctrl Pts',(4.49303736681051,0.447112297141319,3.78638891931142));
#58633=CARTESIAN_POINT('Ctrl Pts',(4.51689528484194,0.494797168872773,4.02673689903048));
#58634=CARTESIAN_POINT('Ctrl Pts',(4.54075320287334,0.421490654719143,4.26054697856981));
#58635=CARTESIAN_POINT('Ctrl Pts',(4.56461112090478,0.245118194360182,4.43064622472778));
#58636=CARTESIAN_POINT('Ctrl Pts',(4.58846903893618,0.00880765856895839,
4.49544073835303));
#58637=CARTESIAN_POINT('Ctrl Pts',(4.61232695696761,-0.229656589644598,
4.43908649592634));
#58638=CARTESIAN_POINT('Ctrl Pts',(4.63618487499902,-0.411963545977342,
4.2753636447643));
#58639=CARTESIAN_POINT('Ctrl Pts',(4.66004279303045,-0.493534193653132,
4.04430688170513));
#58640=CARTESIAN_POINT('Ctrl Pts',(4.68390071106186,-0.454422287381232,
3.80241587917234));
#58641=CARTESIAN_POINT('Ctrl Pts',(4.70775862909328,-0.304191753628974,
3.60883957626609));
#58642=CARTESIAN_POINT('Ctrl Pts',(4.7316165471247,-0.0795780500979935,
3.51091265195837));
#58643=CARTESIAN_POINT('Ctrl Pts',(4.75547446515612,0.164494654344808,3.53258090671894));
#58644=CARTESIAN_POINT('Ctrl Pts',(4.77933238318754,0.368343935055725,3.66854586202706));
#58645=CARTESIAN_POINT('Ctrl Pts',(4.80319030121895,0.482123090158262,3.88556038269908));
#58646=CARTESIAN_POINT('Ctrl Pts',(4.82704821925038,0.478010016947761,4.13055850707372));
#58647=CARTESIAN_POINT('Ctrl Pts',(4.85090613728179,0.357010473862124,4.34363152012653));
#58648=CARTESIAN_POINT('Ctrl Pts',(4.87476405531322,0.14871214514713,4.47267726617372));
#58649=CARTESIAN_POINT('Ctrl Pts',(4.89862197334463,-0.0959503538938319,
4.48614054517122));
#58650=CARTESIAN_POINT('Ctrl Pts',(4.92247989137606,-0.317150377772593,
4.38072921867179));
#58651=CARTESIAN_POINT('Ctrl Pts',(4.94633780940747,-0.460798495283114,
4.1822192273514));
#58652=CARTESIAN_POINT('Ctrl Pts',(4.97019572743889,-0.49176882879792,3.93915167139151));
#58653=CARTESIAN_POINT('Ctrl Pts',(4.99405364547031,-0.40248828815769,3.71096318925158));
#58654=CARTESIAN_POINT('Ctrl Pts',(5.01791156350173,-0.214788397502062,
3.55345208054429));
#58655=CARTESIAN_POINT('Ctrl Pts',(5.04176948153314,0.0254331070612992,
3.50513410186502));
#58656=CARTESIAN_POINT('Ctrl Pts',(5.06562739956457,0.259435524164246,3.57782431515618));
#58657=CARTESIAN_POINT('Ctrl Pts',(5.08948531759598,0.429998888727244,3.75374798322641));
#58658=CARTESIAN_POINT('Ctrl Pts',(5.11334323562741,0.495415812061873,3.98988697716804));
#58659=CARTESIAN_POINT('Ctrl Pts',(5.13720115365882,0.439690074491602,4.2284988806653));
#58660=CARTESIAN_POINT('Ctrl Pts',(5.16105907169025,0.276448136790977,4.41123658365534));
#58661=CARTESIAN_POINT('Ctrl Pts',(5.18491698972166,0.0456070993489057,
4.49341574008204));
#58662=CARTESIAN_POINT('Ctrl Pts',(5.20877490775308,-0.196386116196418,
4.45494130768376));
#58663=CARTESIAN_POINT('Ctrl Pts',(5.2326328257845,-0.390357576881318,4.3052213332044));
#58664=CARTESIAN_POINT('Ctrl Pts',(5.25649074381592,-0.488875976891831,
4.08086642869437));
#58665=CARTESIAN_POINT('Ctrl Pts',(5.28034866184734,-0.467850883838054,
3.83673747961128));
#58666=CARTESIAN_POINT('Ctrl Pts',(5.30420657987876,-0.332423505683668,
3.632530663945));
#58667=CARTESIAN_POINT('Ctrl Pts',(5.32806449791017,-0.115709525355139,
3.5181801106079));
#58668=CARTESIAN_POINT('Ctrl Pts',(5.3519224159416,0.129298585786916,3.52164764473745));
#58669=CARTESIAN_POINT('Ctrl Pts',(5.37578033397301,0.342689670681295,3.64208535978523));
#58670=CARTESIAN_POINT('Ctrl Pts',(5.39963825200445,0.472283796414913,3.85004295376459));
#58671=CARTESIAN_POINT('Ctrl Pts',(5.42349617003584,0.48639166917272,4.09466913029638));
#58672=CARTESIAN_POINT('Ctrl Pts',(5.44735408806728,0.381563529774833,4.31614612573549));
#58673=CARTESIAN_POINT('Ctrl Pts',(5.47121200609869,0.183432713764955,4.46031678178449));
#58674=CARTESIAN_POINT('Ctrl Pts',(5.49506992413012,-0.059552397366927,
4.49192744591021));
#58675=CARTESIAN_POINT('Ctrl Pts',(5.51892784216153,-0.287975325168481,
4.40324844967551));
#58676=CARTESIAN_POINT('Ctrl Pts',(5.54278576019295,-0.445980441674811,
4.21596422322942));
#58677=CARTESIAN_POINT('Ctrl Pts',(5.56664367822437,-0.494931191930538,
3.97587086145358));
#58678=CARTESIAN_POINT('Ctrl Pts',(5.59050159625579,-0.422857784100094,
3.74167773132221));
#58679=CARTESIAN_POINT('Ctrl Pts',(5.61435951428721,-0.247384129650275,
3.57065143242979));
#58680=CARTESIAN_POINT('Ctrl Pts',(5.63821743231862,-0.0114183168777074,
3.50461255354752));
#58681=CARTESIAN_POINT('Ctrl Pts',(5.66207535035005,0.227339585372105,3.55970939936999));
#58682=CARTESIAN_POINT('Ctrl Pts',(5.68593326838146,0.410506766445453,3.72246929038963));
#58683=CARTESIAN_POINT('Ctrl Pts',(5.70979118641288,0.493293861043031,3.9530929995654));
#58684=CARTESIAN_POINT('Ctrl Pts',(5.73364910444431,0.455457169749513,4.19518674831082));
#58685=CARTESIAN_POINT('Ctrl Pts',(5.75750702247572,0.306248793691327,4.38955201985635));
#58686=CARTESIAN_POINT('Ctrl Pts',(5.78136494050715,0.0821542461994931,
4.48866121222712));
#58687=CARTESIAN_POINT('Ctrl Pts',(5.80522285853855,-0.162029253596618,
4.46827942571263));
#58688=CARTESIAN_POINT('Ctrl Pts',(5.82908077656998,-0.366592184898752,
4.33339056701663));
#58689=CARTESIAN_POINT('Ctrl Pts',(5.85293869460139,-0.481513345756758,
4.11697862749145));
#58690=CARTESIAN_POINT('Ctrl Pts',(5.87679661263282,-0.478691368855474,
3.87196223809426));
#58691=CARTESIAN_POINT('Ctrl Pts',(5.90065453066423,-0.358816329143926,
3.65825454842257));
#58692=CARTESIAN_POINT('Ctrl Pts',(5.92451244869565,-0.151200892471453,
3.52811296978032));
#58693=CARTESIAN_POINT('Ctrl Pts',(5.94837036672708,0.093387223403125,3.5133605500302));
#58694=CARTESIAN_POINT('Ctrl Pts',(5.97222828475848,0.315139728168714,3.61760487120619));
#58695=CARTESIAN_POINT('Ctrl Pts',(5.99608620278992,0.459831779670103,3.81535495398299));
#58696=CARTESIAN_POINT('Ctrl Pts',(6.01994412082132,0.492082823488737,4.05825627791571));
#58697=CARTESIAN_POINT('Ctrl Pts',(6.04380203885276,0.404005480250355,4.28691141512903));
#58698=CARTESIAN_POINT('Ctrl Pts',(6.06765995688416,0.21713917558903,4.44541067075535));
#58699=CARTESIAN_POINT('Ctrl Pts',(6.09151787491559,-0.0228261843714051,
4.49499153360272));
#58700=CARTESIAN_POINT('Ctrl Pts',(6.11537579294701,-0.257204988275768,
4.42353981062321));
#58701=CARTESIAN_POINT('Ctrl Pts',(6.13923371097843,-0.428699479426561,
4.24850911946619));
#58702=CARTESIAN_POINT('Ctrl Pts',(6.16309162900984,-0.49534768549136,4.01273373861842));
#58703=CARTESIAN_POINT('Ctrl Pts',(6.18694954704127,-0.440903093044182,
3.77380201544612));
#58704=CARTESIAN_POINT('Ctrl Pts',(6.21080746507268,-0.278582990390117,
3.59026229064107));
#58705=CARTESIAN_POINT('Ctrl Pts',(6.23466538310411,-0.048260127889517,
3.50676273730504));
#58706=CARTESIAN_POINT('Ctrl Pts',(6.25852330113552,0.194087080856728,3.5441598063702));
#58707=CARTESIAN_POINT('Ctrl Pts',(6.28238121916694,0.388553448942855,3.69248145192407));
#58708=CARTESIAN_POINT('Ctrl Pts',(6.30623913719837,0.488798280742691,3.9170164641697));
#58709=CARTESIAN_POINT('Ctrl Pts',(6.33009705522977,0.468067515948433,4.15995908608738));
#58710=CARTESIAN_POINT('Ctrl Pts',(6.36190761260502,0.291040001689194,4.43610431491443));
#58711=CARTESIAN_POINT('Ctrl Pts',(6.40167080932402,-0.143168317426403,
4.54352222151223));
#58712=CARTESIAN_POINT('Ctrl Pts',(6.44938664538688,-0.535165231989368,
4.17285582464912));
#58713=CARTESIAN_POINT('Ctrl Pts',(6.49710248144971,-0.434543251113388,
3.64369891234367));
#58714=CARTESIAN_POINT('Ctrl Pts',(6.54481831751255,0.0645215567551043,
3.4416075490323));
#58715=CARTESIAN_POINT('Ctrl Pts',(6.59253415357539,0.504653900644641,3.75236619672659));
#58716=CARTESIAN_POINT('Ctrl Pts',(6.64024998963822,0.481186238846835,4.29049388273239));
#58717=CARTESIAN_POINT('Ctrl Pts',(6.68796582570107,0.01592709648968,4.56187610740764));
#58718=CARTESIAN_POINT('Ctrl Pts',(6.7356816617639,-0.464005405879062,4.31726850783359));
#58719=CARTESIAN_POINT('Ctrl Pts',(6.78339749782674,-0.517809574500644,
3.78131383674221));
#58720=CARTESIAN_POINT('Ctrl Pts',(6.83111333388957,-0.0961144992151805,
3.44617913151078));
#58721=CARTESIAN_POINT('Ctrl Pts',(6.87882916995242,0.413851019972934,3.61962818876606));
#58722=CARTESIAN_POINT('Ctrl Pts',(6.92654500601525,0.543767061592725,4.14237771887731));
#58723=CARTESIAN_POINT('Ctrl Pts',(6.97426084207809,0.174335412693353,4.53438003016987));
#58724=CARTESIAN_POINT('Ctrl Pts',(7.02197667814094,-0.355192171006393,
4.43565270890428));
#58725=CARTESIAN_POINT('Ctrl Pts',(7.06969251420376,-0.558540766450571,
3.93685892261342));
#58726=CARTESIAN_POINT('Ctrl Pts',(7.11740835026661,-0.248973074301851,
3.49604849518665));
#58727=CARTESIAN_POINT('Ctrl Pts',(7.16512418632944,0.289230577826905,3.51802452284194));
#58728=CARTESIAN_POINT('Ctrl Pts',(7.21284002239229,0.561829257914175,3.98260602935256));
#58729=CARTESIAN_POINT('Ctrl Pts',(7.26055585845511,0.318491529052478,4.46316069626365));
#58730=CARTESIAN_POINT('Ctrl Pts',(7.30827169451797,-0.217321894570402,
4.51838776411367));
#58731=CARTESIAN_POINT('Ctrl Pts',(7.35598753058078,-0.553565266295818,
4.09757137442565));
#58732=CARTESIAN_POINT('Ctrl Pts',(7.40370336664365,-0.381461142739227,
3.58715368886071));
#58733=CARTESIAN_POINT('Ctrl Pts',(7.45141920270646,0.140944621146953,3.45585912402047));
#58734=CARTESIAN_POINT('Ctrl Pts',(7.49913503876933,0.533918768911932,3.82425749787944));
#58735=CARTESIAN_POINT('Ctrl Pts',(7.54685087483214,0.436587096747522,4.3540429157916));
#58736=CARTESIAN_POINT('Ctrl Pts',(7.594566710895,-0.0616692246238245,4.5587052763707));
#58737=CARTESIAN_POINT('Ctrl Pts',(7.64228254695782,-0.503293747851232,
4.25029998493175));
#58738=CARTESIAN_POINT('Ctrl Pts',(7.68999838302067,-0.482735878399531,
3.7120403659385));
#58739=CARTESIAN_POINT('Ctrl Pts',(7.7377142190835,-0.0188742238918736,
3.43821850974892));
#58740=CARTESIAN_POINT('Ctrl Pts',(7.78543005514633,0.462319920793015,3.6802892401675));
#58741=CARTESIAN_POINT('Ctrl Pts',(7.83314589120918,0.518958568528469,4.21595528072725));
#58742=CARTESIAN_POINT('Ctrl Pts',(7.88086172727202,0.099029577569048,4.55330626409362));
#58743=CARTESIAN_POINT('Ctrl Pts',(7.92857756333485,-0.411839798232008,
4.38254759143289));
#58744=CARTESIAN_POINT('Ctrl Pts',(7.9762933993977,-0.544510350349916,3.86048957930736));
#58745=CARTESIAN_POINT('Ctrl Pts',(8.02400923546053,-0.177148669371157,
3.466546133148));
#58746=CARTESIAN_POINT('Ctrl Pts',(8.07172507152338,0.352891360472903,3.56248158116143));
#58747=CARTESIAN_POINT('Ctrl Pts',(8.1194409075862,0.558865824063627,4.06019692528064));
#58748=CARTESIAN_POINT('Ctrl Pts',(8.16715674364906,0.251625202160443,4.50263250666582));
#58749=CARTESIAN_POINT('Ctrl Pts',(8.21487257971187,-0.286686714637947,
4.48349292318459));
#58750=CARTESIAN_POINT('Ctrl Pts',(8.26258841577472,-0.561729810142263,
4.02035434884804));
#58751=CARTESIAN_POINT('Ctrl Pts',(8.31030425183756,-0.32092777766878,3.53852406277244));
#58752=CARTESIAN_POINT('Ctrl Pts',(8.3580200879004,0.21458717114652,3.4804742305729));
#58753=CARTESIAN_POINT('Ctrl Pts',(8.40573592396324,0.553043418849938,3.89951290636976));
#58754=CARTESIAN_POINT('Ctrl Pts',(8.45345176002607,0.383631385356639,4.41083042643994));
#58755=CARTESIAN_POINT('Ctrl Pts',(8.50116759608892,-0.13807525223727,4.54487604447167));
#58756=CARTESIAN_POINT('Ctrl Pts',(8.54888343215175,-0.532985261140852,
4.17855360686946));
#58757=CARTESIAN_POINT('Ctrl Pts',(8.59659926821459,-0.43844670370641,3.64826264467864));
#58758=CARTESIAN_POINT('Ctrl Pts',(8.64431510427743,0.0587242081113278,
3.4409775080543));
#58759=CARTESIAN_POINT('Ctrl Pts',(8.69203094034026,0.501967776032349,3.74705132745037));
#58760=CARTESIAN_POINT('Ctrl Pts',(8.73974677640311,0.484246611455832,4.28541180496438));
#58761=CARTESIAN_POINT('Ctrl Pts',(8.78746261246592,0.021834332487559,4.56167423035448));
#58762=CARTESIAN_POINT('Ctrl Pts',(8.83517844852879,-0.460628749968427,
4.32214256754115));
#58763=CARTESIAN_POINT('Ctrl Pts',(8.88289428459161,-0.520089363644054,
3.78678242815423));
#58764=CARTESIAN_POINT('Ctrl Pts',(8.93061012065447,-0.101943912081849,
3.44722326576734));
#58765=CARTESIAN_POINT('Ctrl Pts',(8.97832595671729,0.409818202553832,3.61528748398963));
#58766=CARTESIAN_POINT('Ctrl Pts',(9.02604179278014,0.545237955920739,4.1366391252272));
#58767=CARTESIAN_POINT('Ctrl Pts',(9.07375762884296,0.179957304801303,4.53251295530543));
#58768=CARTESIAN_POINT('Ctrl Pts',(9.12147346490582,-0.350580908316224,
4.43937194476168));
#58769=CARTESIAN_POINT('Ctrl Pts',(9.16918930096864,-0.559175278946307,
3.94274891673689));
#58770=CARTESIAN_POINT('Ctrl Pts',(9.21690513703149,-0.254270386902387,
3.49870043939378));
#58771=CARTESIAN_POINT('Ctrl Pts',(9.26462097309432,0.284134913886797,3.51500306204057));
#58772=CARTESIAN_POINT('Ctrl Pts',(9.31233680915716,0.56161475127612,3.97668583545263));
#58773=CARTESIAN_POINT('Ctrl Pts',(9.36005264522,0.323355121014866,4.45977836490307));
#58774=CARTESIAN_POINT('Ctrl Pts',(9.40776848128284,-0.211846492332409,
4.52064934726353));
#58775=CARTESIAN_POINT('Ctrl Pts',(9.45548431734568,-0.552506212093558,
4.10340002281193));
#58776=CARTESIAN_POINT('Ctrl Pts',(9.50320015340851,-0.385790975888367,
3.59119686639829));
#58777=CARTESIAN_POINT('Ctrl Pts',(9.55091598947136,0.135202049632292,3.45440391781584));
#58778=CARTESIAN_POINT('Ctrl Pts',(9.59863182553417,0.532036952624682,3.81864024657791));
#58779=CARTESIAN_POINT('Ctrl Pts',(9.64634766159704,0.440294135581046,4.34942202748599));
#58780=CARTESIAN_POINT('Ctrl Pts',(9.69406349765985,-0.0557775609627595,
4.55932418400469));
#58781=CARTESIAN_POINT('Ctrl Pts',(9.74177933372271,-0.500627865026369,
4.25559033604309));
#58782=CARTESIAN_POINT('Ctrl Pts',(9.78949516978553,-0.485743897486414,
3.71714394973028));
#58783=CARTESIAN_POINT('Ctrl Pts',(9.83721100584839,-0.0247938347541151,
3.43844862667992));
#58784=CARTESIAN_POINT('Ctrl Pts',(9.88492684191122,0.458924787935076,3.67543457032792));
#58785=CARTESIAN_POINT('Ctrl Pts',(9.93264267797406,0.521205716397956,4.21047394212484));
#58786=CARTESIAN_POINT('Ctrl Pts',(9.98035851403688,0.104855415711801,4.55223185431066));
#58787=CARTESIAN_POINT('Ctrl Pts',(10.0280743500997,-0.407785226630454,
4.3868667575037));
#58788=CARTESIAN_POINT('Ctrl Pts',(10.0757901861625,-0.54595042077573,3.86623596457089));
#58789=CARTESIAN_POINT('Ctrl Pts',(10.1235060222254,-0.182760942995651,
3.46844274359687));
#58790=CARTESIAN_POINT('Ctrl Pts',(10.1712218582882,0.34826072087591,3.55878673023755));
#58791=CARTESIAN_POINT('Ctrl Pts',(10.2189376943511,0.559469206087141,4.05430365143988));
#58792=CARTESIAN_POINT('Ctrl Pts',(10.2666535304139,0.256908510808291,4.49995269395588));
#58793=CARTESIAN_POINT('Ctrl Pts',(10.3143693664768,-0.281575222991369,
4.4864874848512));
#58794=CARTESIAN_POINT('Ctrl Pts',(10.3620852025396,-0.561484096926345,
4.02627333283551));
#58795=CARTESIAN_POINT('Ctrl Pts',(10.4098010386024,-0.325773485110519,
3.5419319750098));
#58796=CARTESIAN_POINT('Ctrl Pts',(10.4575168746653,0.209099930751681,3.47824153281512));
#58797=CARTESIAN_POINT('Ctrl Pts',(10.5052327107281,0.55195366278862,3.89368991932227));
#58798=CARTESIAN_POINT('Ctrl Pts',(10.552948546791,0.387939853388008,4.40676448870664));
#58799=CARTESIAN_POINT('Ctrl Pts',(10.6006643828538,-0.13232509260073,4.54630096923553));
#58800=CARTESIAN_POINT('Ctrl Pts',(10.6483802189166,-0.531073869970951,
4.18416086379456));
#58801=CARTESIAN_POINT('Ctrl Pts',(10.6960960549795,-0.442129340924997,
3.6529030034519));
#58802=CARTESIAN_POINT('Ctrl Pts',(10.7438118910423,0.0528293649267388,
3.44038965581316));
#58803=CARTESIAN_POINT('Ctrl Pts',(10.7915277271051,0.499274052081986,3.74177509795313));
#58804=CARTESIAN_POINT('Ctrl Pts',(10.839243563168,0.487227694891584,4.28029244094358));
#58805=CARTESIAN_POINT('Ctrl Pts',(10.8869593992308,0.0277526485205102,
4.56141292256198));
#58806=CARTESIAN_POINT('Ctrl Pts',(10.9346752352937,-0.457208082016334,
4.32697927894352));
#58807=CARTESIAN_POINT('Ctrl Pts',(10.9823910713565,-0.522307595786967,
3.79227553224832));
#58808=CARTESIAN_POINT('Ctrl Pts',(11.0301069074193,-0.107764007611043,
3.44832836054127));
#58809=CARTESIAN_POINT('Ctrl Pts',(11.0778227434822,0.405740926916492,3.61098974390844));
#58810=CARTESIAN_POINT('Ctrl Pts',(11.125538579545,0.54664772512998,4.13088523113667));
#58811=CARTESIAN_POINT('Ctrl Pts',(11.1732544156078,0.185559506100192,4.53058679668394));
#58812=CARTESIAN_POINT('Ctrl Pts',(11.2209702516707,-0.345930862581405,
4.4430423427091));
#58813=CARTESIAN_POINT('Ctrl Pts',(11.2686860877335,-0.559747597323992,
3.94864528834179));
#58814=CARTESIAN_POINT('Ctrl Pts',(11.3164019237964,-0.259539500620097,
3.50140805588402));
#58815=CARTESIAN_POINT('Ctrl Pts',(11.3641177598592,0.279007713031768,3.51203547753114));
#58816=CARTESIAN_POINT('Ctrl Pts',(11.411833595922,0.561337850721073,3.97076822846069));
#58817=CARTESIAN_POINT('Ctrl Pts',(11.4595494319849,0.328182802800164,4.45634496498341));
#58818=CARTESIAN_POINT('Ctrl Pts',(11.5072652680477,-0.206347562673641,
4.52285309839201));
#58819=CARTESIAN_POINT('Ctrl Pts',(11.5549811041106,-0.551385786278872,
4.10921718641821));
#58820=CARTESIAN_POINT('Ctrl Pts',(11.6026969401734,-0.390077958183356,
3.59528545163414));
#58821=CARTESIAN_POINT('Ctrl Pts',(11.6504127762362,0.129444461032819,3.45300931394821));
#58822=CARTESIAN_POINT('Ctrl Pts',(11.6981286122991,0.530096039923511,3.8130431397972));
#58823=CARTESIAN_POINT('Ctrl Pts',(11.7458444483619,0.443952268776438,4.34476232707146));
#58824=CARTESIAN_POINT('Ctrl Pts',(11.7935602844247,-0.0498797018717475,
4.55988096454574));
#58825=CARTESIAN_POINT('Ctrl Pts',(11.8412761204876,-0.497906374793238,
4.26085229740167));
#58826=CARTESIAN_POINT('Ctrl Pts',(11.8889919565504,-0.48869796246776,3.72227895182515));
#58827=CARTESIAN_POINT('Ctrl Pts',(11.9367077926133,-0.0307106916234339,
3.43874111807518));
#58828=CARTESIAN_POINT('Ctrl Pts',(11.9844236286761,0.455478679883424,3.67061595167475));
#58829=CARTESIAN_POINT('Ctrl Pts',(12.0321394647389,0.523394971212992,4.20496922507643));
#58830=CARTESIAN_POINT('Ctrl Pts',(12.0798553008018,0.110669607010866,4.5510961052335));
#58831=CARTESIAN_POINT('Ctrl Pts',(12.1275711368646,-0.403685360180124,
4.39114295225112));
#58832=CARTESIAN_POINT('Ctrl Pts',(12.1752869729274,-0.547329849620031,
3.8719972077086));
#58833=CARTESIAN_POINT('Ctrl Pts',(12.2230028089903,-0.188352916401613,
3.4703983969034));
#58834=CARTESIAN_POINT('Ctrl Pts',(12.2707186450531,0.34359139813055,3.55514088718992));
#58835=CARTESIAN_POINT('Ctrl Pts',(12.318434481116,0.560010444926212,4.04840434580723));
#58836=CARTESIAN_POINT('Ctrl Pts',(12.3661503171788,0.262163283277844,4.49721734887317));
#58837=CARTESIAN_POINT('Ctrl Pts',(12.4138661532417,-0.276432455305192,
4.48942800979656));
#58838=CARTESIAN_POINT('Ctrl Pts',(12.4615819893045,-0.561176016721412,
4.03218939850585));
#58839=CARTESIAN_POINT('Ctrl Pts',(12.5092978253673,-0.330583007179444,
3.54539076726965));
#58840=CARTESIAN_POINT('Ctrl Pts',(12.5570136614301,0.203589464528802,3.47606678951191));
#58841=CARTESIAN_POINT('Ctrl Pts',(12.604729497493,0.550802598333678,3.88787874069406));
#58842=CARTESIAN_POINT('Ctrl Pts',(12.6524453335558,0.392205230901379,4.40265336950419));
#58843=CARTESIAN_POINT('Ctrl Pts',(12.7001611696187,-0.126560234920843,
4.54766521348015));
#58844=CARTESIAN_POINT('Ctrl Pts',(12.7478770056815,-0.529103489635726,
4.18974766500481));
#58845=CARTESIAN_POINT('Ctrl Pts',(12.7955928417443,-0.44576286851447,3.65758191611243));
#58846=CARTESIAN_POINT('Ctrl Pts',(12.8433086778072,0.0469286537069902,
3.43986396243348));
#58847=CARTESIAN_POINT('Ctrl Pts',(12.89102451387,0.496524871139168,3.73652755085263));
#58848=CARTESIAN_POINT('Ctrl Pts',(12.9387403499328,0.490154659387074,4.27514194336855));
#58849=CARTESIAN_POINT('Ctrl Pts',(12.9864561859957,0.0336678819209607,
4.56108925568614));
#58850=CARTESIAN_POINT('Ctrl Pts',(13.0341720220585,-0.45373662956012,4.33177967103923));
#58851=CARTESIAN_POINT('Ctrl Pts',(13.0818878581214,-0.524467812480695,
3.79779170939055));
#58852=CARTESIAN_POINT('Ctrl Pts',(13.1296036941842,-0.113572133225654,
3.44949473238301));
#58853=CARTESIAN_POINT('Ctrl Pts',(13.177319530247,0.401618583502394,3.60673521324049));
#58854=CARTESIAN_POINT('Ctrl Pts',(13.2250353663099,0.547996775303968,4.12511679893576));
#58855=CARTESIAN_POINT('Ctrl Pts',(13.2727512023727,0.191141096329688,4.52860170299893));
#58856=CARTESIAN_POINT('Ctrl Pts',(13.3204670384356,-0.341242392487953,
4.4466635296155));
#58857=CARTESIAN_POINT('Ctrl Pts',(13.3681828744984,-0.560257741594785,
3.95454736418435));
#58858=CARTESIAN_POINT('Ctrl Pts',(13.4158987105612,-0.264779785921688,
3.5041710536014));
#58859=CARTESIAN_POINT('Ctrl Pts',(13.4636145466241,0.273849521323983,3.50912209380529));
#58860=CARTESIAN_POINT('Ctrl Pts',(13.5113303826869,0.560998599421335,3.96485386839523));
#58861=CARTESIAN_POINT('Ctrl Pts',(13.5590462187498,0.332974031597074,4.45286087643057));
#58862=CARTESIAN_POINT('Ctrl Pts',(13.6067620548126,-0.200825712906817,
4.52499877347948));
#58863=CARTESIAN_POINT('Ctrl Pts',(13.6544778908754,-0.550204115147588,
4.11502221869768));
#58864=CARTESIAN_POINT('Ctrl Pts',(13.7021937269383,-0.394321612469819,
3.5994189906415));
#58865=CARTESIAN_POINT('Ctrl Pts',(13.7499095630011,0.123672494356884,3.45167546721031));
#58866=CARTESIAN_POINT('Ctrl Pts',(13.7976253990639,0.528096246669736,3.80746679929733));
#58867=CARTESIAN_POINT('Ctrl Pts',(13.8453412351268,0.44756108986054,4.34006433209368));
#58868=CARTESIAN_POINT('Ctrl Pts',(13.8930570711896,-0.0439763023801491,
4.56037555616609));
#58869=CARTESIAN_POINT('Ctrl Pts',(13.9407729072525,-0.495129579482757,
4.26608528452492));
#58870=CARTESIAN_POINT('Ctrl Pts',(13.9884887433153,-0.491597745198497,
3.72744480185615));
#58871=CARTESIAN_POINT('Ctrl Pts',(14.0362045793781,-0.0366241372948624,
3.43909595144367));
#58872=CARTESIAN_POINT('Ctrl Pts',(14.083920415441,0.451981979421435,3.66583391943861));
#58873=CARTESIAN_POINT('Ctrl Pts',(14.1316362515038,0.525526089798339,4.19944174101915));
#58874=CARTESIAN_POINT('Ctrl Pts',(14.1793520875667,0.11647150565515,4.54989914301615));
#58875=CARTESIAN_POINT('Ctrl Pts',(14.2270679236295,-0.399540654275635,
4.39537570069553));
#58876=CARTESIAN_POINT('Ctrl Pts',(14.2747837596924,-0.548648483661927,
3.87777266878906));
#58877=CARTESIAN_POINT('Ctrl Pts',(14.3224995957551,-0.193923968459428,
3.47241287584284));
#58878=CARTESIAN_POINT('Ctrl Pts',(14.370215431818,0.338883910883161,3.5515444569815));
#58879=CARTESIAN_POINT('Ctrl Pts',(14.4179312678808,0.560489480462528,4.04249966364955));
#58880=CARTESIAN_POINT('Ctrl Pts',(14.4656471039437,0.267388935893957,4.49442677524682));
#58881=CARTESIAN_POINT('Ctrl Pts',(14.5133629400065,-0.271258982813659,
4.49231417140114));
#58882=CARTESIAN_POINT('Ctrl Pts',(14.5610787760694,-0.560805603747543,
4.03810188873054));
#58883=CARTESIAN_POINT('Ctrl Pts',(14.6087946121322,-0.335355809656676,
3.54890005536578));
#58884=CARTESIAN_POINT('Ctrl Pts',(14.656510448195,0.198056384554314,3.47395024222346));
#58885=CARTESIAN_POINT('Ctrl Pts',(14.7042262842579,0.549590353339887,3.88208001596329));
#58886=CARTESIAN_POINT('Ctrl Pts',(14.7519421203207,0.396427044118869,4.3984975254762));
#58887=CARTESIAN_POINT('Ctrl Pts',(14.7996579563836,-0.120781319530639,
4.54896862567174));
#58888=CARTESIAN_POINT('Ctrl Pts',(14.8473737924464,-0.527074338995675,
4.19531338994486));
#58889=CARTESIAN_POINT('Ctrl Pts',(14.8950896285092,-0.449346882879826,
3.66229886294881));
#58890=CARTESIAN_POINT('Ctrl Pts',(14.9428054645721,0.041022729875082,3.43940048630678));
#58891=CARTESIAN_POINT('Ctrl Pts',(14.9905213006349,0.493720538569869,3.73130926902151));
#58892=CARTESIAN_POINT('Ctrl Pts',(15.0382371366977,0.493027179828974,4.2699608843321));
#58893=CARTESIAN_POINT('Ctrl Pts',(15.0859529727606,0.0395793756528551,
4.56070326567839));
#58894=CARTESIAN_POINT('Ctrl Pts',(15.1336688088234,-0.450214778192253,
4.33654321062351));
#58895=CARTESIAN_POINT('Ctrl Pts',(15.1813846448863,-0.526569773778615,
3.80333034687015));
#58896=CARTESIAN_POINT('Ctrl Pts',(15.2291004809491,-0.119367643786657,
3.45072225173751));
#58897=CARTESIAN_POINT('Ctrl Pts',(15.2768163170119,0.397451630201876,3.60252436455885));
#58898=CARTESIAN_POINT('Ctrl Pts',(15.3245321530748,0.549284956596614,4.11933446935456));
#58899=CARTESIAN_POINT('Ctrl Pts',(15.3722479891376,0.196701455513243,4.52655789474516));
#58900=CARTESIAN_POINT('Ctrl Pts',(15.4199638252005,-0.336516018808871,
4.45023510325662));
#58901=CARTESIAN_POINT('Ctrl Pts',(15.4676796612633,-0.560705655094284,
3.96045448869));
#58902=CARTESIAN_POINT('Ctrl Pts',(15.5153954973261,-0.269990660741143,
3.50698912564524));
#58903=CARTESIAN_POINT('Ctrl Pts',(15.5631113333889,0.268660911710894,3.50626323446785));
#58904=CARTESIAN_POINT('Ctrl Pts',(15.6108271694518,0.560597035059331,3.95894341219528));
#58905=CARTESIAN_POINT('Ctrl Pts',(15.6585430055146,0.337728275218647,4.44932648624059));
#58906=CARTESIAN_POINT('Ctrl Pts',(15.7062588415775,-0.1952815563728,4.52708613419449));
#58907=CARTESIAN_POINT('Ctrl Pts',(15.7539746776403,-0.548961329954127,
4.12081447485494));
#58908=CARTESIAN_POINT('Ctrl Pts',(15.8016905137031,-0.398521467382777,
3.60359702428645));
#58909=CARTESIAN_POINT('Ctrl Pts',(15.849406349766,0.117886790727162,3.4504025257595));
#58910=CARTESIAN_POINT('Ctrl Pts',(15.8971221858288,0.526037794990907,3.80191184447176));
#58911=CARTESIAN_POINT('Ctrl Pts',(15.9448380218916,0.451120197982628,4.33532856438364));
#58912=CARTESIAN_POINT('Ctrl Pts',(15.9925538579545,-0.0380680182095728,
4.56080790392885));
#58913=CARTESIAN_POINT('Ctrl Pts',(16.0402696940173,-0.492297787528177,
4.27128871615743));
#58914=CARTESIAN_POINT('Ctrl Pts',(16.0879855300802,-0.494442923584513,
3.73264092602517));
#58915=CARTESIAN_POINT('Ctrl Pts',(16.135701366143,-0.0425335149309099,
3.43951308737216));
#58916=CARTESIAN_POINT('Ctrl Pts',(16.1834172022058,0.448435074945997,3.66108900478495));
#58917=CARTESIAN_POINT('Ctrl Pts',(16.2311330382687,0.52759883543946,4.19389210391969));
#58918=CARTESIAN_POINT('Ctrl Pts',(16.2788488743315,0.122260467197297,4.54864110061148));
#58919=CARTESIAN_POINT('Ctrl Pts',(16.3265647103944,-0.395351569291248,
4.39956453268331));
#58920=CARTESIAN_POINT('Ctrl Pts',(16.3742805464572,-0.549906176433804,
3.88356170630145));
#58921=CARTESIAN_POINT('Ctrl Pts',(16.42199638252,-0.199473480363076,3.47448595665642));
#58922=CARTESIAN_POINT('Ctrl Pts',(16.4697122185829,0.334138782019088,3.54799783908671));
#58923=CARTESIAN_POINT('Ctrl Pts',(16.5174280546457,0.560906259487099,4.0365902608309));
#58924=CARTESIAN_POINT('Ctrl Pts',(16.5651438907085,0.272584888215931,4.49158128304055));
#58925=CARTESIAN_POINT('Ctrl Pts',(16.6128597267714,-0.26605538016154,4.49514564908375));
#58926=CARTESIAN_POINT('Ctrl Pts',(16.6605755628342,-0.560372899148451,
4.04401014677825));
#58927=CARTESIAN_POINT('Ctrl Pts',(16.7082913988971,-0.340091362401967,
3.55245944950311));
#58928=CARTESIAN_POINT('Ctrl Pts',(16.7560072349599,0.19250130541649,3.4718921260458));
#58929=CARTESIAN_POINT('Ctrl Pts',(16.8037230710227,0.548317062457662,3.87629438922476));
#58930=CARTESIAN_POINT('Ctrl Pts',(16.8514389070856,0.400604824101502,4.39429741823411));
#58931=CARTESIAN_POINT('Ctrl Pts',(16.8991547431484,-0.114988988324618,
4.55021106103346));
#58932=CARTESIAN_POINT('Ctrl Pts',(16.9468705792113,-0.524986643439221,
4.20085742040038));
#58933=CARTESIAN_POINT('Ctrl Pts',(16.9945864152741,-0.45288098592576,3.66705332002498));
#58934=CARTESIAN_POINT('Ctrl Pts',(17.0423022513369,0.0351122494330066,
3.4389992789138));
#58935=CARTESIAN_POINT('Ctrl Pts',(17.0900180873998,0.490861365866046,3.72612083208173));
#58936=CARTESIAN_POINT('Ctrl Pts',(17.1377339234626,0.49584493715134,4.26474983932169));
#58937=CARTESIAN_POINT('Ctrl Pts',(17.1854497595254,0.0454864730955262,
4.56025499541263));
#58938=CARTESIAN_POINT('Ctrl Pts',(17.2331655955883,-0.446642919103261,
4.34126936858499));
#58939=CARTESIAN_POINT('Ctrl Pts',(17.2808814316511,-0.528613246204851,
3.80889082948154));
#58940=CARTESIAN_POINT('Ctrl Pts',(17.328597267714,-0.125149895556227,3.45201078225777));
#58941=CARTESIAN_POINT('Ctrl Pts',(17.3763131037768,0.393240529860342,3.59835766558462));
#58942=CARTESIAN_POINT('Ctrl Pts',(17.4240289398397,0.55051212592285,4.1135388846668));
#58943=CARTESIAN_POINT('Ctrl Pts',(17.4717447759024,0.202239966032548,4.52445559893916));
#58944=CARTESIAN_POINT('Ctrl Pts',(17.5194606119653,-0.331752266527324,
4.45375666691904));
#58945=CARTESIAN_POINT('Ctrl Pts',(17.5671764480281,-0.561091288070378,
3.96636600572338));
#58946=CARTESIAN_POINT('Ctrl Pts',(17.614892284091,-0.275171546279217,3.50986195899749));
#58947=CARTESIAN_POINT('Ctrl Pts',(17.6626081201538,0.263442460518632,3.50345921706735));
#58948=CARTESIAN_POINT('Ctrl Pts',(17.7103239562167,0.560133202238927,3.95303751636628));
#58949=CARTESIAN_POINT('Ctrl Pts',(17.7580397922795,0.342445005586054,4.44574218699675));
#58950=CARTESIAN_POINT('Ctrl Pts',(17.8057556283423,-0.189715708890181,
4.52911494868296));
#58951=CARTESIAN_POINT('Ctrl Pts',(17.8534714644052,-0.547657568741173,
4.12659331151364));
#58952=CARTESIAN_POINT('Ctrl Pts',(17.901187300468,-0.402677056422281,3.60781908849286));
#58953=CARTESIAN_POINT('Ctrl Pts',(17.9489031365308,0.112087992792125,3.44919063098808));
#58954=CARTESIAN_POINT('Ctrl Pts',(17.9966189725937,0.523920913530056,3.79637889233847));
#58955=CARTESIAN_POINT('Ctrl Pts',(18.0443348086565,0.454629197813879,4.33055554996792));
#58956=CARTESIAN_POINT('Ctrl Pts',(18.0920506447194,-0.0321555056241734,
4.56117795981091));
#58957=CARTESIAN_POINT('Ctrl Pts',(18.1397664807822,-0.489411313471489,
4.27646201432672));
#58958=CARTESIAN_POINT('Ctrl Pts',(18.1874823168451,-0.497233181596917,
3.73786674717144));
#58959=CARTESIAN_POINT('Ctrl Pts',(18.2351981529079,-0.0484381681459794,
3.43999247952716));
#58960=CARTESIAN_POINT('Ctrl Pts',(18.2829139889707,0.444838360430441,3.65638173475637));
#58961=CARTESIAN_POINT('Ctrl Pts',(18.3306298250336,0.529612977905601,4.18832093020544));
#58962=CARTESIAN_POINT('Ctrl Pts',(18.3783456610964,0.128035848626906,4.54732211775687));
#58963=CARTESIAN_POINT('Ctrl Pts',(18.4260614971592,-0.391118570530631,
4.40370898293889));
#58964=CARTESIAN_POINT('Ctrl Pts',(18.4737773332221,-0.551102788237131,
3.88936367722697));
#58965=CARTESIAN_POINT('Ctrl Pts',(18.5214931692849,-0.205000835699102,
3.47661740907615));
#58966=CARTESIAN_POINT('Ctrl Pts',(18.5692090053478,0.329356538604741,3.54450142744705));
#58967=CARTESIAN_POINT('Ctrl Pts',(18.6169248414106,0.561260735706054,4.03067679373969));
#58968=CARTESIAN_POINT('Ctrl Pts',(18.6646406774734,0.2777505631021,4.48868118831814));
#58969=CARTESIAN_POINT('Ctrl Pts',(18.7123565135363,-0.260822225340423,
4.49792212833724));
#58970=CARTESIAN_POINT('Ctrl Pts',(18.7600723495991,-0.559877950986752,
4.04991351638789));
#58971=CARTESIAN_POINT('Ctrl Pts',(18.8077881856619,-0.344789139412875,
3.55606855432066));
#58972=CARTESIAN_POINT('Ctrl Pts',(18.8555040217248,0.186924844147682,3.46989266958543));
#58973=CARTESIAN_POINT('Ctrl Pts',(18.9032198577876,0.546982867117114,3.87052250311704));
#58974=CARTESIAN_POINT('Ctrl Pts',(18.9509356938504,0.404738106803207,4.39005351430856));
#58975=CARTESIAN_POINT('Ctrl Pts',(18.9986515299133,-0.109183884691052,
4.55139238155646));
#58976=CARTESIAN_POINT('Ctrl Pts',(19.0463673659761,-0.522840634850846,
4.20637914057629));
#58977=CARTESIAN_POINT('Ctrl Pts',(19.094083202039,-0.456364785113784,3.67184475922049));
#58978=CARTESIAN_POINT('Ctrl Pts',(19.1417990381018,0.029197868913272,3.43866038485254));
#58979=CARTESIAN_POINT('Ctrl Pts',(19.1895148741647,0.487947670564988,3.72096281627648));
#58980=CARTESIAN_POINT('Ctrl Pts',(19.2372307102275,0.498607618457993,4.25950938727589));
#58981=CARTESIAN_POINT('Ctrl Pts',(19.2849465462903,0.0513885179525073,
4.55974449445321));
#58982=CARTESIAN_POINT('Ctrl Pts',(19.3326623823531,-0.44302144872845,4.34595762039384));
#58983=CARTESIAN_POINT('Ctrl Pts',(19.380378218416,-0.530598003365269,3.81447253878192));
#58984=CARTESIAN_POINT('Ctrl Pts',(19.4280940544788,-0.130918245164485,
3.45336018235082));
#58985=CARTESIAN_POINT('Ctrl Pts',(19.4758098905417,0.38898574814073,3.59423557624425));
#58986=CARTESIAN_POINT('Ctrl Pts',(19.5235257266045,0.551678150913516,4.10773069407674));
#58987=CARTESIAN_POINT('Ctrl Pts',(19.5712415626673,0.207756005258534,4.52229503878775));
#58988=CARTESIAN_POINT('Ctrl Pts',(19.6189573987302,-0.326951650734615,
4.4572278489044));
#58989=CARTESIAN_POINT('Ctrl Pts',(19.666673234793,-0.561414624206118,3.9722812219163));
#58990=CARTESIAN_POINT('Ctrl Pts',(19.7143890708559,-0.280321816997631,
3.51278930393937));
#58991=CARTESIAN_POINT('Ctrl Pts',(19.7621049069187,0.258194652845487,3.5007102220535));
#58992=CARTESIAN_POINT('Ctrl Pts',(19.8098207429815,0.559607330995945,3.94713708427543));
#58993=CARTESIAN_POINT('Ctrl Pts',(19.8575365790444,0.347123361713752,4.44210790974427));
#58994=CARTESIAN_POINT('Ctrl Pts',(19.9052524151072,-0.184128152223511,
4.53108587353909));
#58995=CARTESIAN_POINT('Ctrl Pts',(19.9529682511701,-0.546294178096705,
4.13235642149579));
#58996=CARTESIAN_POINT('Ctrl Pts',(20.0006840872329,-0.406785648814185,
3.61208785870539));
#58997=CARTESIAN_POINT('Ctrl Pts',(20.0483999232957,0.106272459957556,3.44803398021027));
#58998=CARTESIAN_POINT('Ctrl Pts',(20.0961157593586,0.5217539278249,3.7908797683689));
#58999=CARTESIAN_POINT('Ctrl Pts',(20.1438315954214,0.458072423058868,4.32572464996293));
#59000=CARTESIAN_POINT('Ctrl Pts',(20.1915474314842,-0.0262105744965466,
4.56152565902554));
#59001=CARTESIAN_POINT('Ctrl Pts',(20.2392632675471,-0.486524960252488,
4.28152908133109));
#59002=CARTESIAN_POINT('Ctrl Pts',(20.2869791036099,-0.499865224545849,
3.74326461201656));
#59003=CARTESIAN_POINT('Ctrl Pts',(20.3346949396728,-0.0545328049175168,
3.440261547834));
#59004=CARTESIAN_POINT('Ctrl Pts',(20.3824107757356,0.441568512678419,3.6522489094147));
#59005=CARTESIAN_POINT('Ctrl Pts',(20.4221739724547,0.515928418030698,4.09332268501583));
#59006=CARTESIAN_POINT('Ctrl Pts',(20.4539845298298,0.333108474939506,4.36566768059473));
#59007=CARTESIAN_POINT('Ctrl Pts',(20.4778424478613,0.118510552090848,4.48142006140068));
#59008=CARTESIAN_POINT('Ctrl Pts',(20.5017003658927,-0.127372553428812,
4.47887124859312));
#59009=CARTESIAN_POINT('Ctrl Pts',(20.5255582839241,-0.340862259689409,
4.35954554232165));
#59010=CARTESIAN_POINT('Ctrl Pts',(20.5494162019555,-0.471665647836603,
4.15213005589169));
#59011=CARTESIAN_POINT('Ctrl Pts',(20.5732741199869,-0.486782001098211,
3.90760543082941));
#59012=CARTESIAN_POINT('Ctrl Pts',(20.5971320380184,-0.38305332993788,3.68562568155832));
#59013=CARTESIAN_POINT('Ctrl Pts',(20.6209899560498,-0.185558943137764,
3.54054450025879));
#59014=CARTESIAN_POINT('Ctrl Pts',(20.6448478740812,0.0572573647513246,
3.50779920733485));
#59015=CARTESIAN_POINT('Ctrl Pts',(20.6687057921126,0.28610038304352,3.59541756340761));
#59016=CARTESIAN_POINT('Ctrl Pts',(20.6925637101441,0.444969396676924,3.78196356026503));
#59017=CARTESIAN_POINT('Ctrl Pts',(20.7164216281754,0.495039040219165,4.02182741068269));
#59018=CARTESIAN_POINT('Ctrl Pts',(20.7402795462069,0.424054039808096,4.25635280284423));
#59019=CARTESIAN_POINT('Ctrl Pts',(20.7641374642383,0.249378454468877,4.42819351412177));
#59020=CARTESIAN_POINT('Ctrl Pts',(20.7879953822697,0.0137218901755031,
4.49532894963167));
#59021=CARTESIAN_POINT('Ctrl Pts',(20.8118533003011,-0.22528943893053,4.44134312218709));
#59022=CARTESIAN_POINT('Ctrl Pts',(20.8357112183326,-0.409211687104306,
4.27943679589328));
#59023=CARTESIAN_POINT('Ctrl Pts',(20.859569136364,-0.493070359673604,4.04920060553547));
#59024=CARTESIAN_POINT('Ctrl Pts',(20.8834270543954,-0.456359989112496,
3.80693350349834));
#59025=CARTESIAN_POINT('Ctrl Pts',(20.9072849724268,-0.308057122141145,
3.61187643128937));
#59026=CARTESIAN_POINT('Ctrl Pts',(20.9311428904583,-0.0844259229598539,
3.51172613733272));
#59027=CARTESIAN_POINT('Ctrl Pts',(20.9550008084896,0.159849727585384,3.53097210659131));
#59028=CARTESIAN_POINT('Ctrl Pts',(20.9788587265211,0.365037758375503,3.66490817000854));
#59029=CARTESIAN_POINT('Ctrl Pts',(21.0027166445525,0.480964117596,3.88078331455297));
#59030=CARTESIAN_POINT('Ctrl Pts',(21.026574562584,0.479281646861755,4.12581018556955));
#59031=CARTESIAN_POINT('Ctrl Pts',(21.0504324806153,0.360401759160676,4.34007303948752));
#59032=CARTESIAN_POINT('Ctrl Pts',(21.0742903986468,0.153393823636192,4.47117877170218));
#59033=CARTESIAN_POINT('Ctrl Pts',(21.0981483166782,-0.0911230798336762,
4.48706845966041));
#59034=CARTESIAN_POINT('Ctrl Pts',(21.1220062347096,-0.313357908298923,
4.38385664171252));
#59035=CARTESIAN_POINT('Ctrl Pts',(21.145864152741,-0.458968192403581,4.18678141884249));
#59036=CARTESIAN_POINT('Ctrl Pts',(21.1697220707724,-0.492348251467217,
3.94403305123036));
#59037=CARTESIAN_POINT('Ctrl Pts',(21.1935799888039,-0.405335751726616,
3.71497012710753));
#59038=CARTESIAN_POINT('Ctrl Pts',(21.2174379068353,-0.21920761957706,3.55560477096155));
#59039=CARTESIAN_POINT('Ctrl Pts',(21.2412958248667,0.0205227466613194,
3.50490615340017));
#59040=CARTESIAN_POINT('Ctrl Pts',(21.2651537428981,0.255234742309135,3.57527146741714));
#59041=CARTESIAN_POINT('Ctrl Pts',(21.2890116609295,0.427534891009427,3.74949447702405));
#59042=CARTESIAN_POINT('Ctrl Pts',(21.312869578961,0.495291113040325,3.98497291063177));
#59043=CARTESIAN_POINT('Ctrl Pts',(21.3367274969923,0.441935166474334,4.22412587691986));
#59044=CARTESIAN_POINT('Ctrl Pts',(21.3605854150238,0.280514033632862,4.40847396123464));
#59045=CARTESIAN_POINT('Ctrl Pts',(21.3844433330552,0.0504995785194436,
4.49293903542029));
#59046=CARTESIAN_POINT('Ctrl Pts',(21.4083012510867,-0.191863399122956,
4.45686708805594));
#59047=CARTESIAN_POINT('Ctrl Pts',(21.432159169118,-0.387310549425693,4.3090786928523));
#59048=CARTESIAN_POINT('Ctrl Pts',(21.4560170871495,-0.488049720266331,
4.08571213811173));
#59049=CARTESIAN_POINT('Ctrl Pts',(21.4798750051809,-0.469447440294381,
3.84138663085107));
#59050=CARTESIAN_POINT('Ctrl Pts',(21.5037329232123,-0.336052473678932,
3.63584641288874));
#59051=CARTESIAN_POINT('Ctrl Pts',(21.5275908412437,-0.120483523363382,
3.51935166631968));
#59052=CARTESIAN_POINT('Ctrl Pts',(21.5514487592752,0.124546930319796,3.5203885299332));
#59053=CARTESIAN_POINT('Ctrl Pts',(21.5753066773065,0.339122266949511,3.63870346233219));
#59054=CARTESIAN_POINT('Ctrl Pts',(21.599164595338,0.470772971804989,3.84536523971104));
#59055=CARTESIAN_POINT('Ctrl Pts',(21.6230225133694,0.487306861455871,4.08983942814686));
#59056=CARTESIAN_POINT('Ctrl Pts',(21.6468804314008,0.384680949508402,4.31234542922385));
#59057=CARTESIAN_POINT('Ctrl Pts',(21.6707383494323,0.187990066907445,4.45847446473699));
#59058=CARTESIAN_POINT('Ctrl Pts',(21.6945962674636,-0.0546695077989956,
4.49249400502822));
#59059=CARTESIAN_POINT('Ctrl Pts',(21.7184541854951,-0.283960898681086,
4.40608534582272));
#59060=CARTESIAN_POINT('Ctrl Pts',(21.7423121035264,-0.443816114896065,
4.22037775802082));
#59061=CARTESIAN_POINT('Ctrl Pts',(21.766170021558,-0.495146201710716,3.98078180541326));
#59062=CARTESIAN_POINT('Ctrl Pts',(21.7900279395893,-0.425399554695369,
3.74588522487523));
#59063=CARTESIAN_POINT('Ctrl Pts',(21.8138858576208,-0.25163112890579,3.57312662880273));
#59064=CARTESIAN_POINT('Ctrl Pts',(21.8377437756521,-0.0163320378044167,
3.50475019978512));
#59065=CARTESIAN_POINT('Ctrl Pts',(21.8616016936836,0.222960681415914,3.55747583725374));
#59066=CARTESIAN_POINT('Ctrl Pts',(21.885459611715,0.407733440703041,3.71841068663001));
#59067=CARTESIAN_POINT('Ctrl Pts',(21.9093175297464,0.492804267302335,3.94820179346412));
#59068=CARTESIAN_POINT('Ctrl Pts',(21.9331754477779,0.457371026827486,4.19065897275109));
#59069=CARTESIAN_POINT('Ctrl Pts',(21.9570333658092,0.310098111756678,4.38649483975425));
#59070=CARTESIAN_POINT('Ctrl Pts',(21.9808912838407,0.0869977614584207,
4.48782219052945));
#59071=CARTESIAN_POINT('Ctrl Pts',(22.0047492018721,-0.15737591128791,4.46986372771052));
#59072=CARTESIAN_POINT('Ctrl Pts',(22.0286071199035,-0.363266886890503,
4.33701078463543));
#59073=CARTESIAN_POINT('Ctrl Pts',(22.0524650379349,-0.480329213457224,
4.12174952472744));
#59074=CARTESIAN_POINT('Ctrl Pts',(22.0763229559664,-0.479937963428243,
3.87671718963328));
#59075=CARTESIAN_POINT('Ctrl Pts',(22.1001808739978,-0.362188808094022,
3.66183085982978));
#59076=CARTESIAN_POINT('Ctrl Pts',(22.1240387920292,-0.155874623354616,
3.529636096341));
#59077=CARTESIAN_POINT('Ctrl Pts',(22.1478967100606,0.0885551527323001,
3.51245811975107));
#59078=CARTESIAN_POINT('Ctrl Pts',(22.1717546280921,0.311330781786364,3.61449741325855));
#59079=CARTESIAN_POINT('Ctrl Pts',(22.1956125461234,0.457977554205651,3.81080259009947));
#59080=CARTESIAN_POINT('Ctrl Pts',(22.2194704641549,0.492636339578261,4.05337168730347));
#59081=CARTESIAN_POINT('Ctrl Pts',(22.2433283821863,0.406832120751761,4.28288995313029));
#59082=CARTESIAN_POINT('Ctrl Pts',(22.2671863002177,0.22154636656941,4.44323391967918));
#59083=CARTESIAN_POINT('Ctrl Pts',(22.2910442182491,-0.0179135091400202,
4.49519511936025));
#59084=CARTESIAN_POINT('Ctrl Pts',(22.3149021362805,-0.2529930437236,4.42606762362056));
#59085=CARTESIAN_POINT('Ctrl Pts',(22.338760054312,-0.426208888077552,4.25275498785448));
#59086=CARTESIAN_POINT('Ctrl Pts',(22.3626179723434,-0.495205048933098,
4.01763687303198));
#59087=CARTESIAN_POINT('Ctrl Pts',(22.3864758903748,-0.443110087468167,
3.77820606161377));
#59088=CARTESIAN_POINT('Ctrl Pts',(22.4103338084062,-0.282662637164788,
3.59300991103726));
#59089=CARTESIAN_POINT('Ctrl Pts',(22.4341917264377,-0.0530964769854286,
3.50733392083031));
#59090=CARTESIAN_POINT('Ctrl Pts',(22.458049644469,0.189453226607198,3.5421282117862));
#59091=CARTESIAN_POINT('Ctrl Pts',(22.4819075625005,0.385676439696491,3.6888846179772));
#59092=CARTESIAN_POINT('Ctrl Pts',(22.5057654805319,0.487591287867653,3.9117172269821));
#59093=CARTESIAN_POINT('Ctrl Pts',(22.5296233985634,0.470276727405835,4.15613734610506));
#59094=CARTESIAN_POINT('Ctrl Pts',(22.5534813165947,0.337966804695391,4.36237769267677));
#59095=CARTESIAN_POINT('Ctrl Pts',(22.5773392346262,0.123014588878675,4.48000670597833));
#59096=CARTESIAN_POINT('Ctrl Pts',(22.6011971526576,-0.122017660845505,
4.48026122441149));
#59097=CARTESIAN_POINT('Ctrl Pts',(22.625055070689,-0.337213993725473,4.36307837627545));
#59098=CARTESIAN_POINT('Ctrl Pts',(22.6489129887204,-0.469950950795418,
4.15711375897153));
#59099=CARTESIAN_POINT('Ctrl Pts',(22.6727709067518,-0.487774683880463,
3.912729067726));
#59100=CARTESIAN_POINT('Ctrl Pts',(22.6966288247832,-0.386319338946922,
3.6896872918462));
#59101=CARTESIAN_POINT('Ctrl Pts',(22.7204867428147,-0.190407614498503,
3.54252014522276));
#59102=CARTESIAN_POINT('Ctrl Pts',(22.7443446608461,0.0520814161336476,
3.50722927763546));
#59103=CARTESIAN_POINT('Ctrl Pts',(22.7682025788775,0.281801791424649,3.59241522467272));
#59104=CARTESIAN_POINT('Ctrl Pts',(22.7920604969089,0.442679857002608,3.77730419914427));
#59105=CARTESIAN_POINT('Ctrl Pts',(22.8079657755965,0.477669651496365,3.93681187972983));
#59106=CARTESIAN_POINT('Ctrl Pts',(22.8159184149403,0.475016281724327,4.01593044384941));
#59107=CARTESIAN_POINT('Ctrl Pts',(3.98408158505964,0.229225853138217,4.48306385360099));
#59108=CARTESIAN_POINT('Ctrl Pts',(3.99203422440344,0.148766887950233,4.52124364039387));
#59109=CARTESIAN_POINT('Ctrl Pts',(4.00793950309106,-0.0315132651739855,
4.55658776856145));
#59110=CARTESIAN_POINT('Ctrl Pts',(4.03179742112247,-0.29437836981663,4.47338935048851));
#59111=CARTESIAN_POINT('Ctrl Pts',(4.0556553391539,-0.485191777607318,4.27448557757091));
#59112=CARTESIAN_POINT('Ctrl Pts',(4.07951325718531,-0.557397168683185,
4.00843674174317));
#59113=CARTESIAN_POINT('Ctrl Pts',(4.10337117521674,-0.493285636019562,
3.74033843218029));
#59114=CARTESIAN_POINT('Ctrl Pts',(4.12722909324815,-0.308561908987092,
3.53572729771651));
#59115=CARTESIAN_POINT('Ctrl Pts',(4.15108701127957,-0.0483813190761145,
3.44464727048097));
#59116=CARTESIAN_POINT('Ctrl Pts',(4.17494492931099,0.223627135909104,3.48936410886239));
#59117=CARTESIAN_POINT('Ctrl Pts',(4.19880284734241,0.440954086798485,3.65894639349553));
#59118=CARTESIAN_POINT('Ctrl Pts',(4.22266076537383,0.55045499896491,3.91192501290154));
#59119=CARTESIAN_POINT('Ctrl Pts',(4.24651868340524,0.525355068663259,4.18644066347397));
#59120=CARTESIAN_POINT('Ctrl Pts',(4.27037660143667,0.371791302444591,4.41536633561891));
#59121=CARTESIAN_POINT('Ctrl Pts',(4.29423451946808,0.127314547262185,4.54272370785395));
#59122=CARTESIAN_POINT('Ctrl Pts',(4.31809243749951,-0.14829414195428,4.5373703057994));
#59123=CARTESIAN_POINT('Ctrl Pts',(4.34195035553092,-0.387640842632661,
4.40061524972397));
#59124=CARTESIAN_POINT('Ctrl Pts',(4.36580827356235,-0.53219881478122,4.16589884014724));
#59125=CARTESIAN_POINT('Ctrl Pts',(4.38966619159376,-0.546619671109945,
3.89061565172978));
#59126=CARTESIAN_POINT('Ctrl Pts',(4.41352410962518,-0.427377132892538,
3.64207991255526));
#59127=CARTESIAN_POINT('Ctrl Pts',(4.4373820276566,-0.203629241694984,3.48106538615089));
#59128=CARTESIAN_POINT('Ctrl Pts',(4.46123994568802,0.0699115445388116,
3.44694450735191));
#59129=CARTESIAN_POINT('Ctrl Pts',(4.48509786371944,0.326357054473012,3.54806076195131));
#59130=CARTESIAN_POINT('Ctrl Pts',(4.50895578175085,0.502999374434197,3.7596884705576));
#59131=CARTESIAN_POINT('Ctrl Pts',(4.53281369978229,0.556644646112557,4.03007889421215));
#59132=CARTESIAN_POINT('Ctrl Pts',(4.55667161781369,0.474175139017821,4.29311420882242));
#59133=CARTESIAN_POINT('Ctrl Pts',(4.58052953584512,0.275756894216243,4.48447511514554));
#59134=CARTESIAN_POINT('Ctrl Pts',(4.60438745387653,0.00990857728296194,
4.55736865895685));
#59135=CARTESIAN_POINT('Ctrl Pts',(4.62824537190795,-0.258362656684952,
4.49397038324719));
#59136=CARTESIAN_POINT('Ctrl Pts',(4.65210328993938,-0.463457183444019,
4.30978289334447));
#59137=CARTESIAN_POINT('Ctrl Pts',(4.67596120797079,-0.555223804526532,
4.04984504770563));
#59138=CARTESIAN_POINT('Ctrl Pts',(4.69981912600221,-0.511223081411799,
3.77771873014923));
#59139=CARTESIAN_POINT('Ctrl Pts',(4.72367704403363,-0.342214389453536,
3.55994623789246));
#59140=CARTESIAN_POINT('Ctrl Pts',(4.74753496206505,-0.0895249575417115,
3.44977887729433));
#59141=CARTESIAN_POINT('Ctrl Pts',(4.77139288009647,0.185055765100279,3.47415556892044));
#59142=CARTESIAN_POINT('Ctrl Pts',(4.79525079812788,0.414385312357242,3.62711554766008));
#59143=CARTESIAN_POINT('Ctrl Pts',(4.81910871615931,0.542386363113676,3.87125593216545));
#59144=CARTESIAN_POINT('Ctrl Pts',(4.84296663419071,0.537759173780872,4.14687774817434));
#59145=CARTESIAN_POINT('Ctrl Pts',(4.86682455222215,0.401635218192884,4.38658395388507));
#59146=CARTESIAN_POINT('Ctrl Pts',(4.89068247025356,0.167300511433038,4.53175985253543));
#59147=CARTESIAN_POINT('Ctrl Pts',(4.91454038828499,-0.107943727546613,
4.54690598239331));
#59148=CARTESIAN_POINT('Ctrl Pts',(4.9383983063164,-0.356792784813018,4.42831870213619));
#59149=CARTESIAN_POINT('Ctrl Pts',(4.96225622434782,-0.518396287352312,
4.20499583203957));
#59150=CARTESIAN_POINT('Ctrl Pts',(4.98611414237924,-0.553237776802617,
3.93154589703492));
#59151=CARTESIAN_POINT('Ctrl Pts',(5.00997206041066,-0.452797559930213,
3.67483485485756));
#59152=CARTESIAN_POINT('Ctrl Pts',(5.03382997844208,-0.241636005696979,
3.49763554798826));
#59153=CARTESIAN_POINT('Ctrl Pts',(5.05768789647349,0.0286121339618079,
3.44327803376872));
#59154=CARTESIAN_POINT('Ctrl Pts',(5.08154581450492,0.291863827488053,3.52505420509465));
#59155=CARTESIAN_POINT('Ctrl Pts',(5.10540373253633,0.48374686498243,3.72296756053861));
#59156=CARTESIAN_POINT('Ctrl Pts',(5.12926165056775,0.557340616988569,3.98862289364304));
#59157=CARTESIAN_POINT('Ctrl Pts',(5.15311956859917,0.49464940648741,4.25706023915787));
#59158=CARTESIAN_POINT('Ctrl Pts',(5.17697748663059,0.311002942120779,4.46263935401832));
#59159=CARTESIAN_POINT('Ctrl Pts',(5.20083540466201,0.0513077868555636,
4.55509054477827));
#59160=CARTESIAN_POINT('Ctrl Pts',(5.22469332269342,-0.22093351989189,4.5118069769771));
#59161=CARTESIAN_POINT('Ctrl Pts',(5.24855124072485,-0.439150562917527,
4.34337266196288));
#59162=CARTESIAN_POINT('Ctrl Pts',(5.27240915875626,-0.549983331088669,
4.09097437781523));
#59163=CARTESIAN_POINT('Ctrl Pts',(5.29626707678769,-0.526330193563486,
3.81633038019944));
#59164=CARTESIAN_POINT('Ctrl Pts',(5.32012499481911,-0.373974986765411,
3.5865986076849));
#59165=CARTESIAN_POINT('Ctrl Pts',(5.34398291285052,-0.130172708829089,
3.45795473641922));
#59166=CARTESIAN_POINT('Ctrl Pts',(5.36784083088195,0.145460342249349,3.46185569711558));
#59167=CARTESIAN_POINT('Ctrl Pts',(5.39169874891335,0.385524377387638,3.59734759862366));
#59168=CARTESIAN_POINT('Ctrl Pts',(5.41555666694479,0.531317200781484,3.83129898029949));
#59169=CARTESIAN_POINT('Ctrl Pts',(5.4394145849762,0.547188495794237,4.10650235661553));
#59170=CARTESIAN_POINT('Ctrl Pts',(5.46327250300762,0.42925729847004,4.35566300567327));
#59171=CARTESIAN_POINT('Ctrl Pts',(5.48713042103904,0.206360998935678,4.51785436177788));
#59172=CARTESIAN_POINT('Ctrl Pts',(5.51098833907045,-0.0669961859988386,
4.55341622035867));
#59173=CARTESIAN_POINT('Ctrl Pts',(5.53484625710188,-0.323970978517869,
4.45365273830571));
#59174=CARTESIAN_POINT('Ctrl Pts',(5.55870417513329,-0.501726041995696,
4.2429588044862));
#59175=CARTESIAN_POINT('Ctrl Pts',(5.58256209316472,-0.556795421465071,
3.97285482490167));
#59176=CARTESIAN_POINT('Ctrl Pts',(5.60642001119613,-0.475713153578786,
3.70938858005442));
#59177=CARTESIAN_POINT('Ctrl Pts',(5.63027792922756,-0.27830606148521,3.51698474346866));
#59178=CARTESIAN_POINT('Ctrl Pts',(5.65413584725897,-0.0128455564368745,
3.44269129419766));
#59179=CARTESIAN_POINT('Ctrl Pts',(5.67799376529039,0.255756037034639,3.5046750042392));
#59180=CARTESIAN_POINT('Ctrl Pts',(5.70185168332181,0.46181831285622,3.68777916820271));
#59181=CARTESIAN_POINT('Ctrl Pts',(5.72570960135323,0.554953431393631,3.94722983012095));
#59182=CARTESIAN_POINT('Ctrl Pts',(5.74956751938465,0.512387319539865,4.21958423627784));
#59183=CARTESIAN_POINT('Ctrl Pts',(5.77342543741606,0.344528550506956,4.43824431479549));
#59184=CARTESIAN_POINT('Ctrl Pts',(5.79728335544749,0.0924231668635294,
4.54974172178225));
#59185=CARTESIAN_POINT('Ctrl Pts',(5.82114127347891,-0.182282200065281,
4.52681230129395));
#59186=CARTESIAN_POINT('Ctrl Pts',(5.84499919151032,-0.412414601109181,
4.37506292652603));
#59187=CARTESIAN_POINT('Ctrl Pts',(5.86885710954175,-0.541700403334708,
4.13160044316952));
#59188=CARTESIAN_POINT('Ctrl Pts',(5.89271502757316,-0.538525691690445,
3.85595807909033));
#59189=CARTESIAN_POINT('Ctrl Pts',(5.91657294560459,-0.403666797469215,
3.61553786496538));
#59190=CARTESIAN_POINT('Ctrl Pts',(5.94043086363599,-0.170100341263849,
3.46912915944898));
#59191=CARTESIAN_POINT('Ctrl Pts',(5.96428878166742,0.105060216979666,3.45253275189516));
#59192=CARTESIAN_POINT('Ctrl Pts',(5.98814669969884,0.354530812822036,3.5698071562788));
#59193=CARTESIAN_POINT('Ctrl Pts',(6.01200461773026,0.517308736525128,3.79227513259484));
#59194=CARTESIAN_POINT('Ctrl Pts',(6.03586253576167,0.553591019453439,4.06553805729756));
#59195=CARTESIAN_POINT('Ctrl Pts',(6.0597204537931,0.454504394384077,4.32277408438697));
#59196=CARTESIAN_POINT('Ctrl Pts',(6.08357837182452,0.244280620740535,4.50108505220882));
#59197=CARTESIAN_POINT('Ctrl Pts',(6.10743628985593,-0.0256793573627324,
4.55686330558177));
#59198=CARTESIAN_POINT('Ctrl Pts',(6.13129420788736,-0.289354484390735,
4.47648043042773));
#59199=CARTESIAN_POINT('Ctrl Pts',(6.15515212591877,-0.482285035214929,
4.27957167009689));
#59200=CARTESIAN_POINT('Ctrl Pts',(6.17901004395019,-0.557263974895364,
4.01432540012922));
#59201=CARTESIAN_POINT('Ctrl Pts',(6.20286796198161,-0.496014047041978,
3.74552825888183));
#59202=CARTESIAN_POINT('Ctrl Pts',(6.22672588001303,-0.313404643062,3.53904687299508));
#59203=CARTESIAN_POINT('Ctrl Pts',(6.25058379804445,-0.0542924323345977,
3.44511024149985));
#59204=CARTESIAN_POINT('Ctrl Pts',(6.27444171607587,0.218347115212216,3.48718178027374));
#59205=CARTESIAN_POINT('Ctrl Pts',(6.29829963410728,0.437120926894882,3.65404298137615));
#59206=CARTESIAN_POINT('Ctrl Pts',(6.32215755213871,0.549895923261456,3.90664388593688));
#59207=CARTESIAN_POINT('Ctrl Pts',(6.34601547017011,0.526573903738089,4.17995327069166));
#59208=CARTESIAN_POINT('Ctrl Pts',(6.37782602754536,0.327418726170013,4.4906154426808));
#59209=CARTESIAN_POINT('Ctrl Pts',(6.41758922426438,-0.161063729547888,
4.61146011675295));
#59210=CARTESIAN_POINT('Ctrl Pts',(6.46530506032721,-0.60205854017139,4.19446204504257));
#59211=CARTESIAN_POINT('Ctrl Pts',(6.51302089639007,-0.488859252747234,
3.59916283817905));
#59212=CARTESIAN_POINT('Ctrl Pts',(6.56073673245289,0.0725864685289804,
3.37181094029106));
#59213=CARTESIAN_POINT('Ctrl Pts',(6.60845256851574,0.567733426150434,3.72141305678318));
#59214=CARTESIAN_POINT('Ctrl Pts',(6.65616840457857,0.541332409494817,4.32680434473755));
#59215=CARTESIAN_POINT('Ctrl Pts',(6.70388424064141,0.0179179137367747,
4.6321081579338));
#59216=CARTESIAN_POINT('Ctrl Pts',(6.75160007670425,-0.522004047715759,
4.35692568061372));
#59217=CARTESIAN_POINT('Ctrl Pts',(6.79931591276708,-0.582533501572452,
3.75397902491298));
#59218=CARTESIAN_POINT('Ctrl Pts',(6.84703174882993,-0.10812839031349,3.37695395054049));
#59219=CARTESIAN_POINT('Ctrl Pts',(6.89474758489276,0.465580583415614,3.57208337966475));
#59220=CARTESIAN_POINT('Ctrl Pts',(6.9424634209556,0.611735560770294,4.16017430964564));
#59221=CARTESIAN_POINT('Ctrl Pts',(6.99017925701844,0.196126575106773,4.60117519156627));
#59222=CARTESIAN_POINT('Ctrl Pts',(7.03789509308127,-0.399589635450545,
4.49010738789885));
#59223=CARTESIAN_POINT('Ctrl Pts',(7.08561092914412,-0.628355913977057,
3.92896656470948));
#59224=CARTESIAN_POINT('Ctrl Pts',(7.13332676520695,-0.280093617253323,
3.43305676608093));
#59225=CARTESIAN_POINT('Ctrl Pts',(7.1810426012698,0.325383132256395,3.45777970086456));
#59226=CARTESIAN_POINT('Ctrl Pts',(7.22875843733263,0.632055452459012,3.98043185926557));
#59227=CARTESIAN_POINT('Ctrl Pts',(7.27647427339546,0.358301574124045,4.52105375310108));
#59228=CARTESIAN_POINT('Ctrl Pts',(7.32419010945831,-0.244486178793781,
4.58318396235269));
#59229=CARTESIAN_POINT('Ctrl Pts',(7.37190594552114,-0.622758498112341,
4.10976736853928));
#59230=CARTESIAN_POINT('Ctrl Pts',(7.41962178158399,-0.42914211350377,3.53554970961824));
#59231=CARTESIAN_POINT('Ctrl Pts',(7.46733761764681,0.158562080980748,3.38784389968312));
#59232=CARTESIAN_POINT('Ctrl Pts',(7.51505345370967,0.600656274672958,3.80229045545538));
#59233=CARTESIAN_POINT('Ctrl Pts',(7.56276928977248,0.491158570126743,4.3982967283715));
#59234=CARTESIAN_POINT('Ctrl Pts',(7.61048512583535,-0.0693776073840611,
4.62854098691609));
#59235=CARTESIAN_POINT('Ctrl Pts',(7.65820096189817,-0.566203260219877,
4.28158638589565));
#59236=CARTESIAN_POINT('Ctrl Pts',(7.70591679796101,-0.543075747198986,
3.67604667390869));
#59237=CARTESIAN_POINT('Ctrl Pts',(7.75363263402386,-0.0212334191459514,
3.36799828595259));
#59238=CARTESIAN_POINT('Ctrl Pts',(7.80134847008666,0.520107884382028,3.64032679659274));
#59239=CARTESIAN_POINT('Ctrl Pts',(7.84906430614954,0.583826114817312,4.24294874421058));
#59240=CARTESIAN_POINT('Ctrl Pts',(7.89678014221235,0.111407840683781,4.62246712177016));
#59241=CARTESIAN_POINT('Ctrl Pts',(7.94449597827521,-0.463317967772962,
4.43036436352186));
#59242=CARTESIAN_POINT('Ctrl Pts',(7.99221181433803,-0.612571757364041,
3.84305138824375));
#59243=CARTESIAN_POINT('Ctrl Pts',(8.03992765040088,-0.199291476537812,
3.39986673810663));
#59244=CARTESIAN_POINT('Ctrl Pts',(8.08764348646372,0.397001233685627,3.50779369660314));
#59245=CARTESIAN_POINT('Ctrl Pts',(8.13535932252656,0.628721602366905,4.06772127707659));
#59246=CARTESIAN_POINT('Ctrl Pts',(8.18307515858938,0.283077249469033,4.56545936678474));
#59247=CARTESIAN_POINT('Ctrl Pts',(8.23079099465223,-0.32252129731946,4.54392741926377));
#59248=CARTESIAN_POINT('Ctrl Pts',(8.27850683071506,-0.631943574151527,
4.02289855323374));
#59249=CARTESIAN_POINT('Ctrl Pts',(8.32622266677791,-0.361042343138453,
3.48084159342964));
#59250=CARTESIAN_POINT('Ctrl Pts',(8.37393850284074,0.241409626929164,3.41553578665797));
#59251=CARTESIAN_POINT('Ctrl Pts',(8.42165433890358,0.622171422023167,3.88695246013618));
#59252=CARTESIAN_POINT('Ctrl Pts',(8.46937017496642,0.431583626935426,4.46218242893131));
#59253=CARTESIAN_POINT('Ctrl Pts',(8.51708601102927,-0.155334053534803,
4.61298316164806));
#59254=CARTESIAN_POINT('Ctrl Pts',(8.56480184709209,-0.599606082522386,
4.20087202506506));
#59255=CARTESIAN_POINT('Ctrl Pts',(8.61251768315494,-0.493250619804184,
3.60429701705146));
#59256=CARTESIAN_POINT('Ctrl Pts',(8.66023351921777,0.0660644767165412,
3.37110214695249));
#59257=CARTESIAN_POINT('Ctrl Pts',(8.70794935528061,0.564711547735832,3.71543385214437));
#59258=CARTESIAN_POINT('Ctrl Pts',(8.75566519134344,0.544775315265253,4.32108702952508));
#59259=CARTESIAN_POINT('Ctrl Pts',(8.80338102740629,0.0245635283409047,
4.6318810471339));
#59260=CARTESIAN_POINT('Ctrl Pts',(8.85109686346912,-0.518205324617361,
4.36240897642002));
#59261=CARTESIAN_POINT('Ctrl Pts',(8.89881269953197,-0.585098254365674,
3.76013116628075));
#59262=CARTESIAN_POINT('Ctrl Pts',(8.9465285355948,-0.114686454236133,3.3781285970023));
#59263=CARTESIAN_POINT('Ctrl Pts',(8.99424437165764,0.461043681496376,3.56720010581811));
#59264=CARTESIAN_POINT('Ctrl Pts',(9.04196020772047,0.613390310441866,4.15371841694351));
#59265=CARTESIAN_POINT('Ctrl Pts',(9.08967604378332,0.202451179085494,4.59907474052783));
#59266=CARTESIAN_POINT('Ctrl Pts',(9.13739187984615,-0.394401985136886,
4.49429151193569));
#59267=CARTESIAN_POINT('Ctrl Pts',(9.18510771590899,-0.629069737753471,
3.93559278228048));
#59268=CARTESIAN_POINT('Ctrl Pts',(9.23282355197184,-0.28605307070895,3.43604019168954));
#59269=CARTESIAN_POINT('Ctrl Pts',(9.28053938803466,0.319650532659854,3.45438057070715));
#59270=CARTESIAN_POINT('Ctrl Pts',(9.32825522409751,0.631814133431458,3.97377166707843));
#59271=CARTESIAN_POINT('Ctrl Pts',(9.37597106016033,0.363773093762905,4.51724864514637));
#59272=CARTESIAN_POINT('Ctrl Pts',(9.4236868962232,-0.238326375276645,4.58572823348297));
#59273=CARTESIAN_POINT('Ctrl Pts',(9.47140273228601,-0.621567066777005,
4.11632457242483));
#59274=CARTESIAN_POINT('Ctrl Pts',(9.51911856834886,-0.434013156817378,
3.54009826662536));
#59275=CARTESIAN_POINT('Ctrl Pts',(9.5668344044117,0.152101713198456,3.38620679908157));
#59276=CARTESIAN_POINT('Ctrl Pts',(9.61455024047453,0.598539239598464,3.79597107236355));
#59277=CARTESIAN_POINT('Ctrl Pts',(9.66226607653739,0.495328972565208,4.39309824928265));
#59278=CARTESIAN_POINT('Ctrl Pts',(9.7099819126002,-0.0627495115905886,
4.62923725529147));
#59279=CARTESIAN_POINT('Ctrl Pts',(9.75769774866305,-0.563204153727404,
4.28753800770644));
#59280=CARTESIAN_POINT('Ctrl Pts',(9.80541358472588,-0.54645975548653,3.68178818330365));
#59281=CARTESIAN_POINT('Ctrl Pts',(9.85312942078873,-0.027892955418244,
3.36825716649128));
#59282=CARTESIAN_POINT('Ctrl Pts',(9.90084525685157,0.516288374798902,3.63486531430293));
#59283=CARTESIAN_POINT('Ctrl Pts',(9.9485610929144,0.58635414632045,4.2367822623095));
#59284=CARTESIAN_POINT('Ctrl Pts',(9.99627692897723,0.117961883057689,4.62125841547385));
#59285=CARTESIAN_POINT('Ctrl Pts',(10.0439927650401,-0.458756592493822,
4.4352234064191));
#59286=CARTESIAN_POINT('Ctrl Pts',(10.0917086011029,-0.614191830280748,
3.8495160464768));
#59287=CARTESIAN_POINT('Ctrl Pts',(10.1394244371658,-0.205605259764808,
3.40200041654811));
#59288=CARTESIAN_POINT('Ctrl Pts',(10.1871402732286,0.391791784436726,3.5036370055096));
#59289=CARTESIAN_POINT('Ctrl Pts',(10.2348561092915,0.629400404498524,4.06109136983801));
#59290=CARTESIAN_POINT('Ctrl Pts',(10.2825719453542,0.289020948539269,4.56244458923262));
#59291=CARTESIAN_POINT('Ctrl Pts',(10.3302877814171,-0.316770891622519,
4.54729628801251));
#59292=CARTESIAN_POINT('Ctrl Pts',(10.3780036174799,-0.631667147860668,
4.02955738427466));
#59293=CARTESIAN_POINT('Ctrl Pts',(10.4257194535428,-0.366493742769977,
3.48467547975859));
#59294=CARTESIAN_POINT('Ctrl Pts',(10.4734352896056,0.235236505537468,3.41302401146715));
#59295=CARTESIAN_POINT('Ctrl Pts',(10.5211511256685,0.620945451230968,3.88040162523195));
#59296=CARTESIAN_POINT('Ctrl Pts',(10.5688669617313,0.436430634585191,4.45760826680378));
#59297=CARTESIAN_POINT('Ctrl Pts',(10.6165827977941,-0.148865149148659,
4.61458619576145));
#59298=CARTESIAN_POINT('Ctrl Pts',(10.664298633857,-0.597455775834545,4.20718016452724));
#59299=CARTESIAN_POINT('Ctrl Pts',(10.7120144699198,-0.497393570532806,
3.60951740033105));
#59300=CARTESIAN_POINT('Ctrl Pts',(10.7597303059826,0.059432803973042,3.37044081575797));
#59301=CARTESIAN_POINT('Ctrl Pts',(10.8074461420455,0.56168112009921,3.70949811708754));
#59302=CARTESIAN_POINT('Ctrl Pts',(10.8551619781083,0.548129021063343,4.31532776744164));
#59303=CARTESIAN_POINT('Ctrl Pts',(10.9028778141712,0.0312216079359222,
4.63158707701274));
#59304=CARTESIAN_POINT('Ctrl Pts',(10.950593650234,-0.514357088165242,4.36785025554668));
#59305=CARTESIAN_POINT('Ctrl Pts',(10.9983094862968,-0.587593755803164,
3.7663108843084));
#59306=CARTESIAN_POINT('Ctrl Pts',(11.0460253223597,-0.12123403619496,3.37937182377895));
#59307=CARTESIAN_POINT('Ctrl Pts',(11.0937411584225,0.456456764276497,3.56236516706526));
#59308=CARTESIAN_POINT('Ctrl Pts',(11.1414569944854,0.61497629462275,4.14724531131301));
#59309=CARTESIAN_POINT('Ctrl Pts',(11.1891728305482,0.208753630990335,4.59690782052167));
#59310=CARTESIAN_POINT('Ctrl Pts',(11.236888666611,-0.389170704067994,4.49842069353791));
#59311=CARTESIAN_POINT('Ctrl Pts',(11.2846045026739,-0.629713593419695,
3.94222617449013));
#59312=CARTESIAN_POINT('Ctrl Pts',(11.3323203387367,-0.291980800545002,
3.43908624837263));
#59313=CARTESIAN_POINT('Ctrl Pts',(11.3800361747996,0.313882454172263,3.45104205114199));
#59314=CARTESIAN_POINT('Ctrl Pts',(11.4277520108624,0.631502621520784,3.96711438515144));
#59315=CARTESIAN_POINT('Ctrl Pts',(11.4754678469252,0.369204214609944,4.51338608528654));
#59316=CARTESIAN_POINT('Ctrl Pts',(11.5231836829881,-0.232140103514266,
4.58820744384271));
#59317=CARTESIAN_POINT('Ctrl Pts',(11.5708995190509,-0.620306592646703,
4.12286885598323));
#59318=CARTESIAN_POINT('Ctrl Pts',(11.6186153551137,-0.438835993107895,
3.54469790709399));
#59319=CARTESIAN_POINT('Ctrl Pts',(11.6663311911766,0.145624451261577,3.38463787584353));
#59320=CARTESIAN_POINT('Ctrl Pts',(11.7140470272394,0.596355721317347,3.78967435176932));
#59321=CARTESIAN_POINT('Ctrl Pts',(11.7617628633022,0.499444356375145,4.38785610674141));
#59322=CARTESIAN_POINT('Ctrl Pts',(11.8094786993651,-0.0561144459655822,
4.62986363095956));
#59323=CARTESIAN_POINT('Ctrl Pts',(11.8571945354279,-0.560142489144378,
4.29345769116983));
#59324=CARTESIAN_POINT('Ctrl Pts',(11.9049103714908,-0.549783065641843,
3.68756503815187));
#59325=CARTESIAN_POINT('Ctrl Pts',(11.9526262075536,-0.0345493934605723,
3.36858621802886));
#59326=CARTESIAN_POINT('Ctrl Pts',(12.0003420436164,0.512411518346294,3.62944438943981));
#59327=CARTESIAN_POINT('Ctrl Pts',(12.0480578796793,0.588817048391095,4.23058947975914));
#59328=CARTESIAN_POINT('Ctrl Pts',(12.0957737157421,0.1245028227835,4.61998070274044));
#59329=CARTESIAN_POINT('Ctrl Pts',(12.1434895518049,-0.454144260708352,
4.44003410676589));
#59330=CARTESIAN_POINT('Ctrl Pts',(12.1912053878678,-0.615743681684068,
3.85599741975318));
#59331=CARTESIAN_POINT('Ctrl Pts',(12.2389212239306,-0.211896205334937,
3.40420051794564));
#59332=CARTESIAN_POINT('Ctrl Pts',(12.2866370599935,0.386538816815474,3.49953544806202));
#59333=CARTESIAN_POINT('Ctrl Pts',(12.3343528960563,0.63000929582004,4.05445467686));
#59334=CARTESIAN_POINT('Ctrl Pts',(12.3820687321191,0.294932544534008,4.55936733800455));
#59335=CARTESIAN_POINT('Ctrl Pts',(12.429784568182,-0.310985300518122,4.55060436568669));
#59336=CARTESIAN_POINT('Ctrl Pts',(12.4775004042448,-0.631320558980542,
4.0362129322216));
#59337=CARTESIAN_POINT('Ctrl Pts',(12.5252162403077,-0.371904434015698,
3.48856660588983));
#59338=CARTESIAN_POINT('Ctrl Pts',(12.5729320763705,0.229037255191033,3.41057743478371));
#59339=CARTESIAN_POINT('Ctrl Pts',(12.6206479124333,0.619650508764677,3.87386407474765));
#59340=CARTESIAN_POINT('Ctrl Pts',(12.6683637484962,0.44122916559109,4.4529832757215));
#59341=CARTESIAN_POINT('Ctrl Pts',(12.716079584559,-0.142379709528176,4.61612096455669));
#59342=CARTESIAN_POINT('Ctrl Pts',(12.7637954206218,-0.595239106594286,
4.21346529139986));
#59343=CARTESIAN_POINT('Ctrl Pts',(12.8115112566847,-0.501481273143938,
3.61478115656484));
#59344=CARTESIAN_POINT('Ctrl Pts',(12.8592270927475,0.0527945297157079,
3.36984941301012));
#59345=CARTESIAN_POINT('Ctrl Pts',(12.9069429288104,0.558588303589165,3.70359464960132));
#59346=CARTESIAN_POINT('Ctrl Pts',(12.9546587648732,0.551421843290858,4.30953348024615));
#59347=CARTESIAN_POINT('Ctrl Pts',(13.002374600936,0.0378762195828894,4.63122295319618));
#59348=CARTESIAN_POINT('Ctrl Pts',(13.0500904369989,-0.510451719368595,
4.37325067561256));
#59349=CARTESIAN_POINT('Ctrl Pts',(13.0978062730617,-0.590023990114621,
3.77251655941407));
#59350=CARTESIAN_POINT('Ctrl Pts',(13.1455221091246,-0.127768152052348,
3.38068398698829));
#59351=CARTESIAN_POINT('Ctrl Pts',(13.1932379451874,0.451819146005312,3.55757883871291));
#59352=CARTESIAN_POINT('Ctrl Pts',(13.2409537812502,0.616493970155128,4.14075585037205));
#59353=CARTESIAN_POINT('Ctrl Pts',(13.2886696173131,0.215032895532453,4.59467459882739));
#59354=CARTESIAN_POINT('Ctrl Pts',(13.3363854533759,-0.383896195764066,
4.50249451293469));
#59355=CARTESIAN_POINT('Ctrl Pts',(13.3841012894387,-0.630287503488198,
3.94886598394213));
#59356=CARTESIAN_POINT('Ctrl Pts',(13.4318171255016,-0.297876098539286,
3.4421946086935));
#59357=CARTESIAN_POINT('Ctrl Pts',(13.4795329615644,0.308079511111167,3.44776450722078));
#59358=CARTESIAN_POINT('Ctrl Pts',(13.5272487976272,0.631120965295637,3.96046075600252));
#59359=CARTESIAN_POINT('Ctrl Pts',(13.5749646336901,0.374594326004835,4.50946650093658));
#59360=CARTESIAN_POINT('Ctrl Pts',(13.6226804697529,-0.225928046730791,
4.59062131891086));
#59361=CARTESIAN_POINT('Ctrl Pts',(13.6703963058158,-0.618977217803688,
4.12939949185215));
#59362=CARTESIAN_POINT('Ctrl Pts',(13.7181121418786,-0.443610085578744,
3.54934812035851));
#59363=CARTESIAN_POINT('Ctrl Pts',(13.7658279779415,0.139131014051702,3.38313730411011));
#59364=CARTESIAN_POINT('Ctrl Pts',(13.8135438140043,0.594105962672646,3.78340099315002));
#59365=CARTESIAN_POINT('Ctrl Pts',(13.8612596500671,0.503504264276035,4.38257088298437));
#59366=CARTESIAN_POINT('Ctrl Pts',(13.90897548613,-0.0494731474142026,4.63042004436449));
#59367=CARTESIAN_POINT('Ctrl Pts',(13.9566913221928,-0.557018606591754,
4.29934477874546));
#59368=CARTESIAN_POINT('Ctrl Pts',(14.0044071582556,-0.553045308503159,
3.69337659679301));
#59369=CARTESIAN_POINT('Ctrl Pts',(14.0521229943185,-0.0412019939202257,
3.36898540401303));
#59370=CARTESIAN_POINT('Ctrl Pts',(14.0998388303813,0.50847774565382,3.62406462413548));
#59371=CARTESIAN_POINT('Ctrl Pts',(14.1475546664442,0.591214547458171,4.22437108442359));
#59372=CARTESIAN_POINT('Ctrl Pts',(14.195270502507,0.131029933326566,4.61863412549262));
#59373=CARTESIAN_POINT('Ctrl Pts',(14.2429863385698,-0.4494814847335,4.44479593021223));
#59374=CARTESIAN_POINT('Ctrl Pts',(14.2907021746327,-0.617227139201166,
3.86249478815283));
#59375=CARTESIAN_POINT('Ctrl Pts',(14.3384180106955,-0.218163614480107,
3.40646679792233));
#59376=CARTESIAN_POINT('Ctrl Pts',(14.3861338467583,0.381242914296727,3.49548947984197));
#59377=CARTESIAN_POINT('Ctrl Pts',(14.4338496828212,0.630548208698617,4.0478119353149));
#59378=CARTESIAN_POINT('Ctrl Pts',(14.481565518884,0.300811380821271,4.55622795490698));
#59379=CARTESIAN_POINT('Ctrl Pts',(14.5292813549469,-0.305165166642291,
4.55385128484077));
#59380=CARTESIAN_POINT('Ctrl Pts',(14.5769971910097,-0.630903846008588,
4.04286445780787));
#59381=CARTESIAN_POINT('Ctrl Pts',(14.6247130270726,-0.37727381588172,3.49251453961553));
#59382=CARTESIAN_POINT('Ctrl Pts',(14.6724288631354,0.222812564473163,3.40819632836178));
#59383=CARTESIAN_POINT('Ctrl Pts',(14.7201446991982,0.618286738460357,3.86734053484336));
#59384=CARTESIAN_POINT('Ctrl Pts',(14.7678605352611,0.44597868695508,4.44830796940654));
#59385=CARTESIAN_POINT('Ctrl Pts',(14.8155763713239,-0.135878455045208,
4.6175872975589));
#59386=CARTESIAN_POINT('Ctrl Pts',(14.8632922073867,-0.592956321018707,
4.2197267075609));
#59387=CARTESIAN_POINT('Ctrl Pts',(14.9110080434496,-0.505513273594975,
3.62008770107973));
#59388=CARTESIAN_POINT('Ctrl Pts',(14.9587238795124,0.0461503912925444,
3.36932800439917));
#59389=CARTESIAN_POINT('Ctrl Pts',(15.0064397155752,0.555433441741075,3.69772410541485));
#59390=CARTESIAN_POINT('Ctrl Pts',(15.0541555516381,0.554653416196733,4.30370481154056));
#59391=CARTESIAN_POINT('Ctrl Pts',(15.1018713877009,0.0445266241191229,
4.63078871612938));
#59392=CARTESIAN_POINT('Ctrl Pts',(15.1495872237638,-0.506489652017253,
4.37860963676461));
#59393=CARTESIAN_POINT('Ctrl Pts',(15.1973030598266,-0.592388687361149,
3.77874750230084));
#59394=CARTESIAN_POINT('Ctrl Pts',(15.2450188958894,-0.134288076029725,
3.38206494088146));
#59395=CARTESIAN_POINT('Ctrl Pts',(15.2927347319523,0.447131341807447,3.5528416524037));
#59396=CARTESIAN_POINT('Ctrl Pts',(15.3404505680151,0.617943168462805,4.13425075493917));
#59397=CARTESIAN_POINT('Ctrl Pts',(15.3881664040779,0.221288275240951,4.59237532350063));
#59398=CARTESIAN_POINT('Ctrl Pts',(15.4358822401408,-0.378579046092452,
4.50651251762549));
#59399=CARTESIAN_POINT('Ctrl Pts',(15.4835980762036,-0.630791404211772,
3.95551147311801));
#59400=CARTESIAN_POINT('Ctrl Pts',(15.5313139122665,-0.303738309870084,
3.44536492739022));
#59401=CARTESIAN_POINT('Ctrl Pts',(15.5790297483293,0.302242348039936,3.44454830299756));
#59402=CARTESIAN_POINT('Ctrl Pts',(15.6267455843921,0.630669207148581,3.95381151868517));
#59403=CARTESIAN_POINT('Ctrl Pts',(15.674461420455,0.379942829239589,4.50549032746533));
#59404=CARTESIAN_POINT('Ctrl Pts',(15.7221772565178,-0.219690894932002,
4.59296959056563));
#59405=CARTESIAN_POINT('Ctrl Pts',(15.7698930925806,-0.617579089908608,
4.13591575463957));
#59406=CARTESIAN_POINT('Ctrl Pts',(15.8176089286435,-0.448334903946386,
3.5540483898953));
#59407=CARTESIAN_POINT('Ctrl Pts',(15.8653247647063,0.13262212282903,3.3817052505577));
#59408=CARTESIAN_POINT('Ctrl Pts',(15.9130406007692,0.591790213556878,3.77715169332057));
#59409=CARTESIAN_POINT('Ctrl Pts',(15.960756436832,0.507508245312566,4.37724316506909));
#59410=CARTESIAN_POINT('Ctrl Pts',(16.0084722728949,-0.0428263536203826,
4.63090643370248));
#59411=CARTESIAN_POINT('Ctrl Pts',(16.0561881089577,-0.553832853055588,
4.30519861652357));
#59412=CARTESIAN_POINT('Ctrl Pts',(16.1039039450205,-0.556246121716014,
3.69922221370673));
#59413=CARTESIAN_POINT('Ctrl Pts',(16.1516197810833,-0.0478500178579074,
3.36945468010413));
#59414=CARTESIAN_POINT('Ctrl Pts',(16.1993356171462,0.504487493666278,3.61872661594874));
#59415=CARTESIAN_POINT('Ctrl Pts',(16.247051453209,0.593546377218863,4.21812776701271));
#59416=CARTESIAN_POINT('Ctrl Pts',(16.2947672892719,0.137542489686435,4.61721883330181));
#59417=CARTESIAN_POINT('Ctrl Pts',(16.3424831253347,-0.444768782488292,
4.44950834783736));
#59418=CARTESIAN_POINT('Ctrl Pts',(16.3901989613976,-0.618642038056621,
3.86900742997889));
#59419=CARTESIAN_POINT('Ctrl Pts',(16.4379147974604,-0.224406791046256,
3.40879900475058));
#59420=CARTESIAN_POINT('Ctrl Pts',(16.4856306335233,0.375904665124208,3.49149955025639));
#59421=CARTESIAN_POINT('Ctrl Pts',(16.533346469586,0.631017083274371,4.04116388304691));
#59422=CARTESIAN_POINT('Ctrl Pts',(16.5810623056489,0.306656804407812,4.55302678864769));
#59423=CARTESIAN_POINT('Ctrl Pts',(16.6287781417117,-0.29931113646787,4.55703668482238));
#59424=CARTESIAN_POINT('Ctrl Pts',(16.6764939777746,-0.630417055231307,
4.04951122221356));
#59425=CARTESIAN_POINT('Ctrl Pts',(16.7242098138374,-0.382601291962586,
3.49651884241796));
#59426=CARTESIAN_POINT('Ctrl Pts',(16.7719256499003,0.216563124792967,3.40588095668335));
#59427=CARTESIAN_POINT('Ctrl Pts',(16.8196414859631,0.616854291799135,3.86083173012294));
#59428=CARTESIAN_POINT('Ctrl Pts',(16.8673573220259,0.450678671122871,4.44358286716973));
#59429=CARTESIAN_POINT('Ctrl Pts',(16.9150731580887,-0.129362107828251,
4.61898503189482));
#59430=CARTESIAN_POINT('Ctrl Pts',(16.9627889941516,-0.590607672668797,
4.22596371752193));
#59431=CARTESIAN_POINT('Ctrl Pts',(17.0105048302144,-0.509489124030439,
3.62543644444997));
#59432=CARTESIAN_POINT('Ctrl Pts',(17.0582206662773,0.0395011267029154,
3.3688766478407));
#59433=CARTESIAN_POINT('Ctrl Pts',(17.1059365023401,0.552216884982031,3.69188713660034));
#59434=CARTESIAN_POINT('Ctrl Pts',(17.153652338403,0.557823380833178,4.29784240874569));
#59435=CARTESIAN_POINT('Ctrl Pts',(17.2013681744658,0.0511720828492506,
4.63028441404532));
#59436=CARTESIAN_POINT('Ctrl Pts',(17.2490840105287,-0.502471326198846,
4.38392654375487));
#59437=CARTESIAN_POINT('Ctrl Pts',(17.2967998465914,-0.594687584883411,
3.78500302086511));
#59438=CARTESIAN_POINT('Ctrl Pts',(17.3445156826543,-0.140793083924855,
3.38351453206865));
#59439=CARTESIAN_POINT('Ctrl Pts',(17.3922315187171,0.442393872381948,3.5481541343218));
#59440=CARTESIAN_POINT('Ctrl Pts',(17.43994735478,0.61932372857571,4.1277307475695));
#59441=CARTESIAN_POINT('Ctrl Pts',(17.4876631908428,0.227519075297936,4.590010249934));
#59442=CARTESIAN_POINT('Ctrl Pts',(17.5353790269057,-0.373219845656906,
4.51047426130944));
#59443=CARTESIAN_POINT('Ctrl Pts',(17.5830948629685,-0.631225239619516,
3.96216190386831));
#59444=CARTESIAN_POINT('Ctrl Pts',(17.6308106990313,-0.309566783390781,
3.44859685231885));
#59445=CARTESIAN_POINT('Ctrl Pts',(17.6785265350942,0.29637161332294,3.44139379571298));
#59446=CARTESIAN_POINT('Ctrl Pts',(17.726242371157,0.630147397258769,3.94716741176515));
#59447=CARTESIAN_POINT('Ctrl Pts',(17.7739582072198,0.385249130227842,4.50145800652724));
#59448=CARTESIAN_POINT('Ctrl Pts',(17.8216740432827,-0.213429340911116,
4.59525199797214));
#59449=CARTESIAN_POINT('Ctrl Pts',(17.8693898793456,-0.616112364258878,
4.14241692054995));
#59450=CARTESIAN_POINT('Ctrl Pts',(17.9171057154084,-0.453009923400427,
3.55879819362073));
#59451=CARTESIAN_POINT('Ctrl Pts',(17.9648215514712,0.126098500570276,3.38034187425201));
#59452=CARTESIAN_POINT('Ctrl Pts',(18.012537387534,0.589408731192455,3.77092714642348));
#59453=CARTESIAN_POINT('Ctrl Pts',(18.0602532235969,0.511455854741549,4.3718735447732));
#59454=CARTESIAN_POINT('Ctrl Pts',(18.1079690596597,-0.0361748028784226,
4.6313227449477));
#59455=CARTESIAN_POINT('Ctrl Pts',(18.1556848957226,-0.55058558239424,4.31101855428765));
#59456=CARTESIAN_POINT('Ctrl Pts',(18.2034007317854,-0.559385149749292,
3.70510123958967));
#59457=CARTESIAN_POINT('Ctrl Pts',(18.2511165678482,-0.0544927268426965,
3.36999399417717));
#59458=CARTESIAN_POINT('Ctrl Pts',(18.2988324039111,0.500441205601937,3.6134309578002));
#59459=CARTESIAN_POINT('Ctrl Pts',(18.3465482399739,0.595812278664582,4.21186022100458));
#59460=CARTESIAN_POINT('Ctrl Pts',(18.3942640760367,0.144039768479226,4.61573498337195));
#59461=CARTESIAN_POINT('Ctrl Pts',(18.4419799120996,-0.440006677437314,
4.4541708362083));
#59462=CARTESIAN_POINT('Ctrl Pts',(18.4896957481624,-0.619988221090196,
3.87553462183804));
#59463=CARTESIAN_POINT('Ctrl Pts',(18.5374115842252,-0.230625041570952,
3.41119687937986));
#59464=CARTESIAN_POINT('Ctrl Pts',(18.5851274202881,0.370524662245315,3.48756610248778));
#59465=CARTESIAN_POINT('Ctrl Pts',(18.6328432563509,0.631415867466904,4.03451125849008));
#59466=CARTESIAN_POINT('Ctrl Pts',(18.6805590924138,0.31246816601179,4.54976419479712));
#59467=CARTESIAN_POINT('Ctrl Pts',(18.7282749284766,-0.293423860232864,
4.56016021181225));
#59468=CARTESIAN_POINT('Ctrl Pts',(18.7759907645394,-0.629860240718928,
4.05615248714788));
#59469=CARTESIAN_POINT('Ctrl Pts',(18.8237066006023,-0.387886270507855,
3.50057906951772));
#59470=CARTESIAN_POINT('Ctrl Pts',(18.8714224366651,0.210289630309142,3.40363157692976));
#59471=CARTESIAN_POINT('Ctrl Pts',(18.919138272728,0.615353327889266,3.85433838355196));
#59472=CARTESIAN_POINT('Ctrl Pts',(18.9668541087908,0.455328596044662,4.43880849385601));
#59473=CARTESIAN_POINT('Ctrl Pts',(19.0145699448537,-0.122831391686292,
4.62031401230505));
#59474=CARTESIAN_POINT('Ctrl Pts',(19.0622857809165,-0.588193422413584,
4.2321756285162));
#59475=CARTESIAN_POINT('Ctrl Pts',(19.1100016169793,-0.513408382846255,
3.63082679254236));
#59476=CARTESIAN_POINT('Ctrl Pts',(19.1577174530421,0.0328474745430158,
3.36849539350727));
#59477=CARTESIAN_POINT('Ctrl Pts',(19.205433289105,0.548938990540088,3.68608439142882));
#59478=CARTESIAN_POINT('Ctrl Pts',(19.2531491251678,0.560931385193363,4.2919469231649));
#59479=CARTESIAN_POINT('Ctrl Pts',(19.3008649612307,0.0578118574426247,
4.62971010270368));
#59480=CARTESIAN_POINT('Ctrl Pts',(19.3485807972935,-0.498397187901359,
4.38920080648958));
#59481=CARTESIAN_POINT('Ctrl Pts',(19.3962966333563,-0.596920427988996,
3.79128241936144));
#59482=CARTESIAN_POINT('Ctrl Pts',(19.4440124694192,-0.147282451949449,
3.38503260125846));
#59483=CARTESIAN_POINT('Ctrl Pts',(19.491728305482,0.437607261597584,3.54351680188243));
#59484=CARTESIAN_POINT('Ctrl Pts',(19.5394441415449,0.620635501579114,4.12119655861503));
#59485=CARTESIAN_POINT('Ctrl Pts',(19.5871599776077,0.233724595248439,4.58757962923414));
#59486=CARTESIAN_POINT('Ctrl Pts',(19.6348758136705,-0.367819173932889,
4.51437932582758));
#59487=CARTESIAN_POINT('Ctrl Pts',(19.6825916497334,-0.631588991354928,
3.96881649615688));
#59488=CARTESIAN_POINT('Ctrl Pts',(19.7303074857962,-0.315360815373557,
3.4518901025469));
#59489=CARTESIAN_POINT('Ctrl Pts',(19.778023321859,0.290467852693633,3.43830118837221));
#59490=CARTESIAN_POINT('Ctrl Pts',(19.8257391579219,0.629555794415491,3.94052945152661));
#59491=CARTESIAN_POINT('Ctrl Pts',(19.8734549939847,0.390512260364629,4.49736946054851));
#59492=CARTESIAN_POINT('Ctrl Pts',(19.9211708300476,-0.207143364153331,
4.59746927979605));
#59493=CARTESIAN_POINT('Ctrl Pts',(19.9688866661104,-0.61457855576007,4.14890039401813));
#59494=CARTESIAN_POINT('Ctrl Pts',(20.0166025021732,-0.45763207183192,3.5636005413983));
#59495=CARTESIAN_POINT('Ctrl Pts',(20.0643183382361,0.119556051622903,3.37904064719698));
#59496=CARTESIAN_POINT('Ctrl Pts',(20.1120341742989,0.586970881772813,3.7647406560623));
#59497=CARTESIAN_POINT('Ctrl Pts',(20.1597500103618,0.515329468049299,4.36643880344312));
#59498=CARTESIAN_POINT('Ctrl Pts',(20.2074658464246,-0.029486781418557,
4.63171390504007));
#59499=CARTESIAN_POINT('Ctrl Pts',(20.2551816824874,-0.547338447674763,
4.31671898245684));
#59500=CARTESIAN_POINT('Ctrl Pts',(20.3028975185503,-0.562346186529673,
3.71117381387971));
#59501=CARTESIAN_POINT('Ctrl Pts',(20.3506133546131,-0.0613491664957494,
3.37029669484294));
#59502=CARTESIAN_POINT('Ctrl Pts',(20.398329190676,0.496762641213801,3.60878154740643));
#59503=CARTESIAN_POINT('Ctrl Pts',(20.4380923873949,0.580417208789547,4.10498761157686));
#59504=CARTESIAN_POINT('Ctrl Pts',(20.4699029447702,0.374745574175769,4.41137453781958));
#59505=CARTESIAN_POINT('Ctrl Pts',(20.4937608628016,0.13332385162888,4.54159545884303));
#59506=CARTESIAN_POINT('Ctrl Pts',(20.517618780833,-0.143293564288956,4.53872805560682));
#59507=CARTESIAN_POINT('Ctrl Pts',(20.5414766988645,-0.38346854803195,4.40448715909776));
#59508=CARTESIAN_POINT('Ctrl Pts',(20.5653346168959,-0.530621786340447,
4.17114564603877));
#59509=CARTESIAN_POINT('Ctrl Pts',(20.5891925349273,-0.547627617499454,
3.89605651468078));
#59510=CARTESIAN_POINT('Ctrl Pts',(20.6130504529587,-0.430933317123153,
3.64633026976583));
#59511=CARTESIAN_POINT('Ctrl Pts',(20.6369083709901,-0.208752997660079,
3.48311457674551));
#59512=CARTESIAN_POINT('Ctrl Pts',(20.6607662890215,0.0644142843662171,
3.4462762657402));
#59513=CARTESIAN_POINT('Ctrl Pts',(20.684624207053,0.321861676845817,3.54484653226013));
#59514=CARTESIAN_POINT('Ctrl Pts',(20.7084821250844,0.500588620804837,3.75470996102831));
#59515=CARTESIAN_POINT('Ctrl Pts',(20.7323400431158,0.556916750317041,4.02455574134091));
#59516=CARTESIAN_POINT('Ctrl Pts',(20.7561979611472,0.47705893600668,4.28839577951569));
#59517=CARTESIAN_POINT('Ctrl Pts',(20.7800558791787,0.280549668164313,4.48171582646486));
#59518=CARTESIAN_POINT('Ctrl Pts',(20.8039137972101,0.0154370662995263,
4.55724289713534));
#59519=CARTESIAN_POINT('Ctrl Pts',(20.8277717152415,-0.253449631274377,
4.49650907789895));
#59520=CARTESIAN_POINT('Ctrl Pts',(20.8516296332729,-0.460361354274216,
4.31436517051053));
#59521=CARTESIAN_POINT('Ctrl Pts',(20.8754875513043,-0.554701993332711,
4.05535046556385));
#59522=CARTESIAN_POINT('Ctrl Pts',(20.8993454693358,-0.513402987365846,
3.78280103771366));
#59523=CARTESIAN_POINT('Ctrl Pts',(20.9232033873672,-0.346562912086465,
3.56336268648205));
#59524=CARTESIAN_POINT('Ctrl Pts',(20.9470613053986,-0.0949787932613798,
3.45069404477467));
#59525=CARTESIAN_POINT('Ctrl Pts',(20.97091922343,0.179830242856268,3.47234567582879));
#59526=CARTESIAN_POINT('Ctrl Pts',(20.9947771414614,0.410665878084123,3.62302316008453));
#59527=CARTESIAN_POINT('Ctrl Pts',(21.0186350594928,0.541082524061315,3.86588175144064));
#59528=CARTESIAN_POINT('Ctrl Pts',(21.0424929775243,0.539189751860116,4.14153590729571));
#59529=CARTESIAN_POINT('Ctrl Pts',(21.0663508955557,0.405450399288564,4.38258067876424));
#59530=CARTESIAN_POINT('Ctrl Pts',(21.0902088135871,0.172567379211795,4.53007405282339));
#59531=CARTESIAN_POINT('Ctrl Pts',(21.1140667316185,-0.102513065388571,
4.54794988212627));
#59532=CARTESIAN_POINT('Ctrl Pts',(21.1379246496499,-0.352526273278862,
4.43183703934844));
#59533=CARTESIAN_POINT('Ctrl Pts',(21.1617825676814,-0.516337204635697,
4.21012827746935));
#59534=CARTESIAN_POINT('Ctrl Pts',(21.1856404857128,-0.553889624765765,
3.93703742795684));
#59535=CARTESIAN_POINT('Ctrl Pts',(21.2094984037442,-0.456000943963824,
3.67934264238169));
#59536=CARTESIAN_POINT('Ctrl Pts',(21.2333563217756,-0.246607611160355,
3.50005731527167));
#59537=CARTESIAN_POINT('Ctrl Pts',(21.257214239807,0.0230880000356606,3.44302159274494));
#59538=CARTESIAN_POINT('Ctrl Pts',(21.2810721578385,0.287137966314551,3.52218226257825));
#59539=CARTESIAN_POINT('Ctrl Pts',(21.3049300758698,0.480974878350452,3.71818238470557));
#59540=CARTESIAN_POINT('Ctrl Pts',(21.3287879939013,0.557200331135927,3.9830945903298));
#59541=CARTESIAN_POINT('Ctrl Pts',(21.3526459119327,0.497175125126959,4.25214062911267));
#59542=CARTESIAN_POINT('Ctrl Pts',(21.3765038299641,0.31557705824565,4.45953141590455));
#59543=CARTESIAN_POINT('Ctrl Pts',(21.4003617479955,0.0568118044769688,
4.55455425412338));
#59544=CARTESIAN_POINT('Ctrl Pts',(21.424219666027,-0.215845483008899,4.51397347145443));
#59545=CARTESIAN_POINT('Ctrl Pts',(21.4480775840584,-0.435722670386138,
4.34771217465862));
#59546=CARTESIAN_POINT('Ctrl Pts',(21.4719355020898,-0.549053796006754,
4.0964257796693));
#59547=CARTESIAN_POINT('Ctrl Pts',(21.4957934201212,-0.528126312578589,
3.82156065496534));
#59548=CARTESIAN_POINT('Ctrl Pts',(21.5196513381527,-0.378057559853047,
3.59032881071252));
#59549=CARTESIAN_POINT('Ctrl Pts',(21.543509256184,-0.135543435662257,3.45927273145963));
#59550=CARTESIAN_POINT('Ctrl Pts',(21.5673671742155,0.14011475067701,3.46043919847993));
#59551=CARTESIAN_POINT('Ctrl Pts',(21.5912250922469,0.381511063826562,3.59354297881304));
#59552=CARTESIAN_POINT('Ctrl Pts',(21.6150830102783,0.529617529717794,3.8260365724933));
#59553=CARTESIAN_POINT('Ctrl Pts',(21.6389409283097,0.548218083101175,4.10106896286759));
#59554=CARTESIAN_POINT('Ctrl Pts',(21.6627988463412,0.432764382005563,4.35138723875747));
#59555=CARTESIAN_POINT('Ctrl Pts',(21.6866567643726,0.211488001244504,4.51578176317496));
#59556=CARTESIAN_POINT('Ctrl Pts',(21.710514682404,-0.0615029566383307,
4.55405359688301));
#59557=CARTESIAN_POINT('Ctrl Pts',(21.7343726004354,-0.319454766316188,
4.4568442340362));
#59558=CARTESIAN_POINT('Ctrl Pts',(21.7582305184669,-0.499291183856609,
4.24792401178047));
#59559=CARTESIAN_POINT('Ctrl Pts',(21.7820884364982,-0.557037306525311,
3.97837961532992));
#59560=CARTESIAN_POINT('Ctrl Pts',(21.8059463545297,-0.478572634356998,
3.71412199185867));
#59561=CARTESIAN_POINT('Ctrl Pts',(21.8298042725611,-0.283083917031579,
3.51976932853855));
#59562=CARTESIAN_POINT('Ctrl Pts',(21.8536621905926,-0.018373470940863,
3.44284614561161));
#59563=CARTESIAN_POINT('Ctrl Pts',(21.8775201086239,0.250829789278194,3.5021622566489));
#59564=CARTESIAN_POINT('Ctrl Pts',(21.9013780266554,0.458698333552465,3.68321325676341));
#59565=CARTESIAN_POINT('Ctrl Pts',(21.9252359446868,0.55440264058141,3.94172724469688));
#59566=CARTESIAN_POINT('Ctrl Pts',(21.9490938627182,0.514540400363477,4.21449050861997));
#59567=CARTESIAN_POINT('Ctrl Pts',(21.9729517807496,0.348859016457567,4.4348050005813));
#59568=CARTESIAN_POINT('Ctrl Pts',(21.996809698781,0.0978721002989983,4.54879782605011));
#59569=CARTESIAN_POINT('Ctrl Pts',(22.0206676168125,-0.177047210365213,
4.52859463409701));
#59570=CARTESIAN_POINT('Ctrl Pts',(22.0445255348439,-0.408673655425848,
4.3791356554785));
#59571=CARTESIAN_POINT('Ctrl Pts',(22.0683834528753,-0.540368259688198,
4.13696768164748));
#59572=CARTESIAN_POINT('Ctrl Pts',(22.0922413709067,-0.53992810512055,3.86130737872913));
#59573=CARTESIAN_POINT('Ctrl Pts',(22.1160992889381,-0.407460821505317,
3.61956119962225));
#59574=CARTESIAN_POINT('Ctrl Pts',(22.1399572069695,-0.175358268020808,
3.47084267015335));
#59575=CARTESIAN_POINT('Ctrl Pts',(22.163815125001,0.0996241586556461,3.45151752178681));
#59576=CARTESIAN_POINT('Ctrl Pts',(22.1876730430324,0.350245764837839,3.56631127970877));
#59577=CARTESIAN_POINT('Ctrl Pts',(22.2115309610638,0.51522274100534,3.78715374318048));
#59578=CARTESIAN_POINT('Ctrl Pts',(22.2353888790952,0.554213722627899,4.06004291426965));
#59579=CARTESIAN_POINT('Ctrl Pts',(22.2592467971266,0.457684352558003,4.31824995726588));
#59580=CARTESIAN_POINT('Ctrl Pts',(22.2831047151581,0.249238691275201,4.49863621678958));
#59581=CARTESIAN_POINT('Ctrl Pts',(22.3069626331895,-0.0201526192614011,
4.55709233866662));
#59582=CARTESIAN_POINT('Ctrl Pts',(22.3308205512209,-0.284616065231974,
4.47932420896945));
#59583=CARTESIAN_POINT('Ctrl Pts',(22.3546784692523,-0.479483130864429,
4.28434825342259));
#59584=CARTESIAN_POINT('Ctrl Pts',(22.3785363872838,-0.557103509392546,
4.01984140485232));
#59585=CARTESIAN_POINT('Ctrl Pts',(22.4023943053151,-0.498496906094933,
3.75048279151596));
#59586=CARTESIAN_POINT('Ctrl Pts',(22.4262522233466,-0.317994227800984,
3.542137933897));
#59587=CARTESIAN_POINT('Ctrl Pts',(22.450110141378,-0.0597333038680864,
3.44575282046209));
#59588=CARTESIAN_POINT('Ctrl Pts',(22.4739680594094,0.213134049493302,3.48489624527193));
#59589=CARTESIAN_POINT('Ctrl Pts',(22.4978259774408,0.433884304103661,3.6499965589521));
#59590=CARTESIAN_POINT('Ctrl Pts',(22.5216838954723,0.548538061567711,3.90068226732924));
#59591=CARTESIAN_POINT('Ctrl Pts',(22.5455418135037,0.529059256943919,4.17565382996358));
#59592=CARTESIAN_POINT('Ctrl Pts',(22.5693997315351,0.380211173855379,4.40767331583304));
#59593=CARTESIAN_POINT('Ctrl Pts',(22.5932576495665,0.138390873272415,4.54000544018811));
#59594=CARTESIAN_POINT('Ctrl Pts',(22.6171155675979,-0.137269333605106,
4.54029177230974));
#59595=CARTESIAN_POINT('Ctrl Pts',(22.6409734856293,-0.379364264814148,
4.40846158181013));
#59596=CARTESIAN_POINT('Ctrl Pts',(22.6648314036608,-0.528692759685234,
4.17675229015827));
#59597=CARTESIAN_POINT('Ctrl Pts',(22.6886893216921,-0.54874438127821,3.90182058373076));
#59598=CARTESIAN_POINT('Ctrl Pts',(22.7125472397236,-0.434607562942265,
3.65089956353622));
#59599=CARTESIAN_POINT('Ctrl Pts',(22.736405157755,-0.214207731687487,3.48533716867003));
#59600=CARTESIAN_POINT('Ctrl Pts',(22.7602630757864,0.0585913648593265,
3.44563509732658));
#59601=CARTESIAN_POINT('Ctrl Pts',(22.7841209938179,0.31702578011682,3.5414689143437));
#59602=CARTESIAN_POINT('Ctrl Pts',(22.8079789118493,0.498012898707086,3.74946820019106));
#59603=CARTESIAN_POINT('Ctrl Pts',(22.8238841905369,0.537376264140017,3.92891364167179));
#59604=CARTESIAN_POINT('Ctrl Pts',(22.8318368298807,0.534391234777113,4.01792167950194));
#59605=CARTESIAN_POINT('Ctrl Pts',(3.99999999999998,0.254694598474614,4.53673594206822));
#59606=CARTESIAN_POINT('Ctrl Pts',(4.00795263934379,0.165296026927429,4.57915779516171));
#59607=CARTESIAN_POINT('Ctrl Pts',(4.0238579180314,-0.0350146299391769,
4.61842892627033));
#59608=CARTESIAN_POINT('Ctrl Pts',(4.04771583606282,-0.327086058023631,
4.5259865276721));
#59609=CARTESIAN_POINT('Ctrl Pts',(4.07157375409423,-0.539100294705402,
4.30498302442502));
#59610=CARTESIAN_POINT('Ctrl Pts',(4.09543167212566,-0.619328256935644,
4.00937412827253));
#59611=CARTESIAN_POINT('Ctrl Pts',(4.11928959015708,-0.548093442686671,
3.71148804617917));
#59612=CARTESIAN_POINT('Ctrl Pts',(4.1431475081885,-0.342845496867427,3.48414304986991));
#59613=CARTESIAN_POINT('Ctrl Pts',(4.16700542621991,-0.0537568536316998,
3.38294333505492));
#59614=CARTESIAN_POINT('Ctrl Pts',(4.19086334425134,0.248473820944083,3.43262855616194));
#59615=CARTESIAN_POINT('Ctrl Pts',(4.21472126228276,0.489947458130694,3.62105272953394));
#59616=CARTESIAN_POINT('Ctrl Pts',(4.23857918031417,0.611614759069978,3.90213920826301));
#59617=CARTESIAN_POINT('Ctrl Pts',(4.26243709834559,0.583726034554802,4.20715564703007));
#59618=CARTESIAN_POINT('Ctrl Pts',(4.28629501637702,0.413100159498109,4.46151671210738));
#59619=CARTESIAN_POINT('Ctrl Pts',(4.31015293440843,0.141460167127662,4.60302446238992));
#59620=CARTESIAN_POINT('Ctrl Pts',(4.33401085243986,-0.164770755236008,
4.59707625642582));
#59621=CARTESIAN_POINT('Ctrl Pts',(4.35786877047126,-0.430710704813839,
4.44512666775742));
#59622=CARTESIAN_POINT('Ctrl Pts',(4.38172668850269,-0.59133017320549,4.18433147003372));
#59623=CARTESIAN_POINT('Ctrl Pts',(4.40558460653411,-0.607353296958831,
3.87846221409715));
#59624=CARTESIAN_POINT('Ctrl Pts',(4.42944252456553,-0.474862000813124,
3.60231225357117));
#59625=CARTESIAN_POINT('Ctrl Pts',(4.45330044259694,-0.226254007744579,
3.42340778189093));
#59626=CARTESIAN_POINT('Ctrl Pts',(4.47715836062837,0.0776792518003291,
3.38549581251083));
#59627=CARTESIAN_POINT('Ctrl Pts',(4.50101627865978,0.362617819109035,3.49784685630402));
#59628=CARTESIAN_POINT('Ctrl Pts',(4.5248741966912,0.558886451727075,3.73298802180378));
#59629=CARTESIAN_POINT('Ctrl Pts',(4.54873211472262,0.618492123352341,4.03342088939383));
#59630=CARTESIAN_POINT('Ctrl Pts',(4.57259003275404,0.5268596233165,4.32568143907503));
#59631=CARTESIAN_POINT('Ctrl Pts',(4.59644795078546,0.306395594072305,4.5383040055633));
#59632=CARTESIAN_POINT('Ctrl Pts',(4.62030586881688,0.0110094959969652,
4.61929657956068));
#59633=CARTESIAN_POINT('Ctrl Pts',(4.6441637868483,-0.287068723725306,4.54885427056805));
#59634=CARTESIAN_POINT('Ctrl Pts',(4.66802170487971,-0.514950820910697,
4.34420214192463));
#59635=CARTESIAN_POINT('Ctrl Pts',(4.69187962291114,-0.616913415399932,
4.05538321370614));
#59636=CARTESIAN_POINT('Ctrl Pts',(4.71573754094255,-0.568023875442366,
3.75302158112612));
#59637=CARTESIAN_POINT('Ctrl Pts',(4.73959545897398,-0.380237025278099,
3.51105289951885));
#59638=CARTESIAN_POINT('Ctrl Pts',(4.76345337700539,-0.0994718649854296,
3.38864510263028));
#59639=CARTESIAN_POINT('Ctrl Pts',(4.78731129503681,0.205616875855751,3.41573023112194));
#59640=CARTESIAN_POINT('Ctrl Pts',(4.81116921306823,0.460426689658758,3.5856852332931));
#59641=CARTESIAN_POINT('Ctrl Pts',(4.83502713109965,0.60264963606909,3.85695148163183));
#59642=CARTESIAN_POINT('Ctrl Pts',(4.85888504913107,0.597508330613982,4.16319698927494));
#59643=CARTESIAN_POINT('Ctrl Pts',(4.88274296716248,0.446259962523644,4.42953638764361));
#59644=CARTESIAN_POINT('Ctrl Pts',(4.90660088519391,0.185888877718945,4.59084243889714));
#59645=CARTESIAN_POINT('Ctrl Pts',(4.93045880322533,-0.119937101199393,
4.60767141961541));
#59646=CARTESIAN_POINT('Ctrl Pts',(4.95431672125674,-0.396435191853442,
4.47590818560059));
#59647=CARTESIAN_POINT('Ctrl Pts',(4.97817463928816,-0.575994079421511,
4.22777243672773));
#59648=CARTESIAN_POINT('Ctrl Pts',(5.00203255731958,-0.614706724807315,
3.92394012267834));
#59649=CARTESIAN_POINT('Ctrl Pts',(5.025890475351,-0.503106831702736,3.63870652046354));
#59650=CARTESIAN_POINT('Ctrl Pts',(5.04974839338242,-0.268483613891896,
3.44181901543221));
#59651=CARTESIAN_POINT('Ctrl Pts',(5.07360631141384,0.0317911608623165,
3.38142196567243));
#59652=CARTESIAN_POINT('Ctrl Pts',(5.09746422944526,0.32429213081186,3.47228409503311));
#59653=CARTESIAN_POINT('Ctrl Pts',(5.12132214747667,0.537494841237617,3.69218713785082));
#59654=CARTESIAN_POINT('Ctrl Pts',(5.1451800655081,0.619265421915264,3.98735881011802));
#59655=CARTESIAN_POINT('Ctrl Pts',(5.16903798353952,0.549608738483219,4.28562159765047));
#59656=CARTESIAN_POINT('Ctrl Pts',(5.19289590157094,0.34555774745058,4.51404212438126));
#59657=CARTESIAN_POINT('Ctrl Pts',(5.21675381960235,0.0570084743622218,
4.61676534947452));
#59658=CARTESIAN_POINT('Ctrl Pts',(5.24061173763377,-0.245480923587363,
4.56867264627043));
#59659=CARTESIAN_POINT('Ctrl Pts',(5.26446965566519,-0.487943548953736,
4.38152399072137));
#59660=CARTESIAN_POINT('Ctrl Pts',(5.28832757369661,-0.611090685285508,
4.10108232693608));
#59661=CARTESIAN_POINT('Ctrl Pts',(5.31218549172803,-0.584809503288917,
3.79592328078761));
#59662=CARTESIAN_POINT('Ctrl Pts',(5.33604340975945,-0.415526467847156,
3.5406665514248));
#59663=CARTESIAN_POINT('Ctrl Pts',(5.35990132779088,-0.144635892303038,
3.39772936223054));
#59664=CARTESIAN_POINT('Ctrl Pts',(5.38375924582228,0.161622098711782,3.40206374949372));
#59665=CARTESIAN_POINT('Ctrl Pts',(5.40761716385371,0.428359084093981,3.55260983746209));
#59666=CARTESIAN_POINT('Ctrl Pts',(5.43147508188512,0.590350605148055,3.81255500683439));
#59667=CARTESIAN_POINT('Ctrl Pts',(5.45533299991655,0.607985322415754,4.11833558293467));
#59668=CARTESIAN_POINT('Ctrl Pts',(5.47919091794796,0.476951067165249,4.39517988561105));
#59669=CARTESIAN_POINT('Ctrl Pts',(5.50304883597938,0.2292892841064,4.57539194177126));
#59670=CARTESIAN_POINT('Ctrl Pts',(5.5269067540108,-0.0744399746307492,
4.61490499480714));
#59671=CARTESIAN_POINT('Ctrl Pts',(5.55076467204222,-0.359966631867259,
4.5040570269359));
#59672=CARTESIAN_POINT('Ctrl Pts',(5.57462259007364,-0.55747164231658,4.26995338574299));
#59673=CARTESIAN_POINT('Ctrl Pts',(5.59848050810506,-0.618659650999605,
3.96983878834977));
#59674=CARTESIAN_POINT('Ctrl Pts',(5.62233842613648,-0.528568523057477,
3.67709942878664));
#59675=CARTESIAN_POINT('Ctrl Pts',(5.6461963441679,-0.309227993320144,3.46331805450751));
#59676=CARTESIAN_POINT('Ctrl Pts',(5.67005426219932,-0.0142727959960426,
3.38077003484781));
#59677=CARTESIAN_POINT('Ctrl Pts',(5.69391218023074,0.284172488697173,3.4496406091084));
#59678=CARTESIAN_POINT('Ctrl Pts',(5.71777009826216,0.513129859266986,3.65308904601577));
#59679=CARTESIAN_POINT('Ctrl Pts',(5.74162801629357,0.616613001744231,3.94136666067651));
#59680=CARTESIAN_POINT('Ctrl Pts',(5.765485934325,0.569317469330215,4.24398172424487));
#59681=CARTESIAN_POINT('Ctrl Pts',(5.78934385235641,0.382808307322586,4.48693660973462));
#59682=CARTESIAN_POINT('Ctrl Pts',(5.81320177038783,0.102692087527565,4.61082223133738));
#59683=CARTESIAN_POINT('Ctrl Pts',(5.83705968841925,-0.202535146533943,
4.58534517687525));
#59684=CARTESIAN_POINT('Ctrl Pts',(5.86091760645067,-0.458237017319611,
4.41673528603543));
#59685=CARTESIAN_POINT('Ctrl Pts',(5.88477552448209,-0.601887460912657,
4.14622225884759));
#59686=CARTESIAN_POINT('Ctrl Pts',(5.9086334425135,-0.598360014525416,3.83995392008642));
#59687=CARTESIAN_POINT('Ctrl Pts',(5.93249136054493,-0.448517265794504,
3.57282118150817));
#59688=CARTESIAN_POINT('Ctrl Pts',(5.95634927857635,-0.188999790056246,
3.41014534911766));
#59689=CARTESIAN_POINT('Ctrl Pts',(5.98020719660777,0.116733210556207,3.39170495376011));
#59690=CARTESIAN_POINT('Ctrl Pts',(6.00406511463918,0.393921897475357,3.52200944135141));
#59691=CARTESIAN_POINT('Ctrl Pts',(6.02792303267061,0.574785693380153,3.76919531120668));
#59692=CARTESIAN_POINT('Ctrl Pts',(6.05178095070201,0.61509921541814,4.07281983667942));
#59693=CARTESIAN_POINT('Ctrl Pts',(6.07563886873346,0.505003308517799,4.35863675364492));
#59694=CARTESIAN_POINT('Ctrl Pts',(6.09949678676485,0.27142206589204,4.55675943366228));
#59695=CARTESIAN_POINT('Ctrl Pts',(6.12335470479629,-0.0285325303540597,
4.61873507756083));
#59696=CARTESIAN_POINT('Ctrl Pts',(6.14721262282769,-0.321503980505702,
4.52942105023226));
#59697=CARTESIAN_POINT('Ctrl Pts',(6.17107054085913,-0.535870591003297,
4.31063422072759));
#59698=CARTESIAN_POINT('Ctrl Pts',(6.19492845889052,-0.619180264299368,
4.01591706164003));
#59699=CARTESIAN_POINT('Ctrl Pts',(6.21878637692196,-0.551125001039776,
3.71725450231754));
#59700=CARTESIAN_POINT('Ctrl Pts',(6.24264429495337,-0.348226295733882,
3.48783145534908));
#59701=CARTESIAN_POINT('Ctrl Pts',(6.2665022129848,-0.0603247367796791,
3.38345774569467));
#59702=CARTESIAN_POINT('Ctrl Pts',(6.29036013101621,0.242607149567705,3.43020375417728));
#59703=CARTESIAN_POINT('Ctrl Pts',(6.31421804904763,0.485688404846908,3.61560451082823));
#59704=CARTESIAN_POINT('Ctrl Pts',(6.33807596707905,0.61099356578022,3.89627130770405));
#59705=CARTESIAN_POINT('Ctrl Pts',(6.36193388511046,0.585080291527744,4.19994745529594));
#59706=CARTESIAN_POINT('Ctrl Pts',(6.3937444424857,0.363797450650833,4.54512657044717));
#59707=CARTESIAN_POINT('Ctrl Pts',(6.43350763920472,-0.178959141669374,
4.67939801199369));
#59708=CARTESIAN_POINT('Ctrl Pts',(6.48122347526757,-0.668951848353412,
4.21606826543601));
#59709=CARTESIAN_POINT('Ctrl Pts',(6.5289393113304,-0.543175254381078,3.55462676401443));
#59710=CARTESIAN_POINT('Ctrl Pts',(6.57665514739324,0.0806513803028556,
3.30201433154981));
#59711=CARTESIAN_POINT('Ctrl Pts',(6.62437098345608,0.630812951656228,3.69045991683978));
#59712=CARTESIAN_POINT('Ctrl Pts',(6.67208681951892,0.601478580142798,4.36311480674272));
#59713=CARTESIAN_POINT('Ctrl Pts',(6.71980265558175,0.0199087309838695,
4.70234020845997));
#59714=CARTESIAN_POINT('Ctrl Pts',(6.76751849164459,-0.580002689552455,
4.39658285339385));
#59715=CARTESIAN_POINT('Ctrl Pts',(6.81523432770743,-0.64725742864426,3.72664421308375));
#59716=CARTESIAN_POINT('Ctrl Pts',(6.86295016377027,-0.120142281411799,
3.30772876957018));
#59717=CARTESIAN_POINT('Ctrl Pts',(6.91066599983311,0.517310146858294,3.52453857056345));
#59718=CARTESIAN_POINT('Ctrl Pts',(6.95838183589594,0.679704059947864,4.17797090041396));
#59719=CARTESIAN_POINT('Ctrl Pts',(7.00609767195879,0.217917737520193,4.66797035296266));
#59720=CARTESIAN_POINT('Ctrl Pts',(7.05381350802161,-0.443987099894697,
4.54456206689342));
#59721=CARTESIAN_POINT('Ctrl Pts',(7.10152934408447,-0.698171061503544,
3.92107420680554));
#59722=CARTESIAN_POINT('Ctrl Pts',(7.14924518014729,-0.311214160204793,
3.3700650369752));
#59723=CARTESIAN_POINT('Ctrl Pts',(7.19696101621015,0.361535686685884,3.39753487888718));
#59724=CARTESIAN_POINT('Ctrl Pts',(7.24467685227297,0.702281647003851,3.97825768917858));
#59725=CARTESIAN_POINT('Ctrl Pts',(7.29239268833582,0.398111619195611,4.5789468099385));
#59726=CARTESIAN_POINT('Ctrl Pts',(7.34010852439865,-0.271650463017158,
4.64798016059173));
#59727=CARTESIAN_POINT('Ctrl Pts',(7.38782436046149,-0.691951729928866,
4.1219633626529));
#59728=CARTESIAN_POINT('Ctrl Pts',(7.43554019652432,-0.476823084268312,
3.48394573037578));
#59729=CARTESIAN_POINT('Ctrl Pts',(7.48325603258717,0.17617954081454,3.31982867534575));
#59730=CARTESIAN_POINT('Ctrl Pts',(7.53097186865001,0.667393780433987,3.78032341303133));
#59731=CARTESIAN_POINT('Ctrl Pts',(7.57868770471284,0.545730043505963,4.44255054095139));
#59732=CARTESIAN_POINT('Ctrl Pts',(7.62640354077568,-0.077085990144297,
4.69837669746149));
#59733=CARTESIAN_POINT('Ctrl Pts',(7.67411937683852,-0.629112772588521,
4.31287278685955));
#59734=CARTESIAN_POINT('Ctrl Pts',(7.72183521290136,-0.603415615998442,
3.64005298187887));
#59735=CARTESIAN_POINT('Ctrl Pts',(7.76955104896419,-0.0235926144000291,
3.29777806215626));
#59736=CARTESIAN_POINT('Ctrl Pts',(7.81726688502703,0.577895847971041,3.60036435301798));
#59737=CARTESIAN_POINT('Ctrl Pts',(7.86498272108987,0.648693661106154,4.26994220769392));
#59738=CARTESIAN_POINT('Ctrl Pts',(7.9126985571527,0.123786103798515,4.6916279794467));
#59739=CARTESIAN_POINT('Ctrl Pts',(7.96041439321555,-0.514796137313916,
4.47818113561083));
#59740=CARTESIAN_POINT('Ctrl Pts',(8.00813022927838,-0.680633164378164,
3.82561319718015));
#59741=CARTESIAN_POINT('Ctrl Pts',(8.05584606534123,-0.221434283704469,
3.33318734306526));
#59742=CARTESIAN_POINT('Ctrl Pts',(8.10356190140405,0.441111106898351,3.45310581204486));
#59743=CARTESIAN_POINT('Ctrl Pts',(8.1512777374669,0.698577380670183,4.07524562887252));
#59744=CARTESIAN_POINT('Ctrl Pts',(8.19899357352974,0.314529296777622,4.62828622690367));
#59745=CARTESIAN_POINT('Ctrl Pts',(8.24670940959258,-0.358355880000973,
4.60436191534297));
#59746=CARTESIAN_POINT('Ctrl Pts',(8.29442524565541,-0.70215733816079,4.02544275761943));
#59747=CARTESIAN_POINT('Ctrl Pts',(8.34214108171825,-0.401156908608127,
3.42315912408683));
#59748=CARTESIAN_POINT('Ctrl Pts',(8.3898569177811,0.268232082711808,3.35059734274305));
#59749=CARTESIAN_POINT('Ctrl Pts',(8.43757275384392,0.691299425196396,3.8743920139026));
#59750=CARTESIAN_POINT('Ctrl Pts',(8.48528858990677,0.479535868514212,4.51353443142269));
#59751=CARTESIAN_POINT('Ctrl Pts',(8.53300442596961,-0.172592854832336,
4.68109027882443));
#59752=CARTESIAN_POINT('Ctrl Pts',(8.58072026203244,-0.66622690390392,4.22319044326068));
#59753=CARTESIAN_POINT('Ctrl Pts',(8.62843609809529,-0.548054535901959,
3.56033138942427));
#59754=CARTESIAN_POINT('Ctrl Pts',(8.67615193415812,0.0734047453217555,
3.30122678585069));
#59755=CARTESIAN_POINT('Ctrl Pts',(8.72386777022095,0.627455319439314,3.68381637683837));
#59756=CARTESIAN_POINT('Ctrl Pts',(8.7715836062838,0.605304019074675,4.35676225408577));
#59757=CARTESIAN_POINT('Ctrl Pts',(8.81929944234663,0.0272927241942496,
4.70208786391332));
#59758=CARTESIAN_POINT('Ctrl Pts',(8.86701527840948,-0.575781899266294,
4.40267538529889));
#59759=CARTESIAN_POINT('Ctrl Pts',(8.9147311144723,-0.650107145087294,3.73347990440727));
#59760=CARTESIAN_POINT('Ctrl Pts',(8.96244695053515,-0.127428996390418,
3.30903392823725));
#59761=CARTESIAN_POINT('Ctrl Pts',(9.01016278659798,0.512269160438921,3.51911272764658));
#59762=CARTESIAN_POINT('Ctrl Pts',(9.05787862266082,0.681542664962993,4.17079770865984));
#59763=CARTESIAN_POINT('Ctrl Pts',(9.10559445872366,0.224945053369686,4.66563652575022));
#59764=CARTESIAN_POINT('Ctrl Pts',(9.1533102947865,-0.438223061957547,4.54921107910972));
#59765=CARTESIAN_POINT('Ctrl Pts',(9.20102613084934,-0.698964196560635,
3.92843664782408));
#59766=CARTESIAN_POINT('Ctrl Pts',(9.24874196691217,-0.317835754515511,
3.3733799439853));
#59767=CARTESIAN_POINT('Ctrl Pts',(9.29645780297501,0.355166151432911,3.39375807937372));
#59768=CARTESIAN_POINT('Ctrl Pts',(9.34417363903786,0.702013515586798,3.97085749870423));
#59769=CARTESIAN_POINT('Ctrl Pts',(9.39188947510068,0.404191066510942,4.57471892538967));
#59770=CARTESIAN_POINT('Ctrl Pts',(9.43960531116354,-0.264806258220881,
4.65080711970243));
#59771=CARTESIAN_POINT('Ctrl Pts',(9.48732114722635,-0.690627921460452,
4.12924912203773));
#59772=CARTESIAN_POINT('Ctrl Pts',(9.53503698328922,-0.482235337746388,
3.48899966685243));
#59773=CARTESIAN_POINT('Ctrl Pts',(9.58275281935202,0.169001376764621,3.31800968034731));
#59774=CARTESIAN_POINT('Ctrl Pts',(9.63046865541491,0.665041526572246,3.77330189814918));
#59775=CARTESIAN_POINT('Ctrl Pts',(9.6781844914777,0.550363809549371,4.43677447107931));
#59776=CARTESIAN_POINT('Ctrl Pts',(9.72590032754056,-0.0697214622184181,
4.69915032657822));
#59777=CARTESIAN_POINT('Ctrl Pts',(9.7736161636034,-0.625780442428439,4.31948567936979));
#59778=CARTESIAN_POINT('Ctrl Pts',(9.82133199966623,-0.607175613486645,
3.64643241687702));
#59779=CARTESIAN_POINT('Ctrl Pts',(9.86904783572907,-0.030992076082374,
3.29806570630264));
#59780=CARTESIAN_POINT('Ctrl Pts',(9.91676367179191,0.573651961662729,3.59429605827795));
#59781=CARTESIAN_POINT('Ctrl Pts',(9.96447950785474,0.651502576242943,4.26309058249416));
#59782=CARTESIAN_POINT('Ctrl Pts',(10.0121953439176,0.131068350403577,4.69028497663703));
#59783=CARTESIAN_POINT('Ctrl Pts',(10.0599111799804,-0.50972795835719,4.48358005533451));
#59784=CARTESIAN_POINT('Ctrl Pts',(10.1076270160433,-0.682433239785766,
3.83279612838271));
#59785=CARTESIAN_POINT('Ctrl Pts',(10.1553428521061,-0.228449576533966,
3.33555808949935));
#59786=CARTESIAN_POINT('Ctrl Pts',(10.2030586881689,0.435322847997542,3.44848728078164));
#59787=CARTESIAN_POINT('Ctrl Pts',(10.2507745242318,0.699331602909907,4.06787908823615));
#59788=CARTESIAN_POINT('Ctrl Pts',(10.2984903602946,0.321133386270249,4.62493648450936));
#59789=CARTESIAN_POINT('Ctrl Pts',(10.3462061963575,-0.351966560253669,
4.60810509117381));
#59790=CARTESIAN_POINT('Ctrl Pts',(10.3939220324203,-0.701850198794989,
4.03284143571381));
#59791=CARTESIAN_POINT('Ctrl Pts',(10.4416378684831,-0.407214000429435,
3.42741898450738));
#59792=CARTESIAN_POINT('Ctrl Pts',(10.489353704546,0.261373080323254,3.34780649011919));
#59793=CARTESIAN_POINT('Ctrl Pts',(10.5370695406088,0.689937239673316,3.86711333114163));
#59794=CARTESIAN_POINT('Ctrl Pts',(10.5847853766716,0.484921415782374,4.50845204490092));
#59795=CARTESIAN_POINT('Ctrl Pts',(10.6325012127345,-0.165405205696588,
4.68287142228737));
#59796=CARTESIAN_POINT('Ctrl Pts',(10.6802170487973,-0.66383768169814,4.23019946525991));
#59797=CARTESIAN_POINT('Ctrl Pts',(10.7279328848602,-0.552657800140614,
3.5661317972102));
#59798=CARTESIAN_POINT('Ctrl Pts',(10.775648720923,0.0660362430193439,3.30049197570278));
#59799=CARTESIAN_POINT('Ctrl Pts',(10.8233645569858,0.624088188116435,3.67722113622194));
#59800=CARTESIAN_POINT('Ctrl Pts',(10.8710803930487,0.609030347235101,4.3503630939397));
#59801=CARTESIAN_POINT('Ctrl Pts',(10.9187962291115,0.0346905673513346,
4.70176123146349));
#59802=CARTESIAN_POINT('Ctrl Pts',(10.9665120651743,-0.57150609431415,4.40872123214985));
#59803=CARTESIAN_POINT('Ctrl Pts',(11.0142279012372,-0.65287991581936,3.74034623636848));
#59804=CARTESIAN_POINT('Ctrl Pts',(11.0619437373,-0.134704064778877,3.31041528701663));
#59805=CARTESIAN_POINT('Ctrl Pts',(11.1096595733629,0.507172601636502,3.51374059022208));
#59806=CARTESIAN_POINT('Ctrl Pts',(11.1573754094257,0.68330486411552,4.16360539148934));
#59807=CARTESIAN_POINT('Ctrl Pts',(11.2050912454885,0.231947755880478,4.66322884435941));
#59808=CARTESIAN_POINT('Ctrl Pts',(11.2528070815514,-0.432410545554582,
4.55379904436673));
#59809=CARTESIAN_POINT('Ctrl Pts',(11.3005229176142,-0.699679589515398,
3.93580706063847));
#59810=CARTESIAN_POINT('Ctrl Pts',(11.348238753677,-0.324422100469907,3.37676444086124));
#59811=CARTESIAN_POINT('Ctrl Pts',(11.3959545897399,0.348757195312759,3.39004862475285));
#59812=CARTESIAN_POINT('Ctrl Pts',(11.4436704258027,0.701667392320496,3.9634605418422));
#59813=CARTESIAN_POINT('Ctrl Pts',(11.4913862618656,0.410225626419724,4.57042720558968));
#59814=CARTESIAN_POINT('Ctrl Pts',(11.5391020979284,-0.257932644354891,
4.65356178929341));
#59815=CARTESIAN_POINT('Ctrl Pts',(11.5868179339912,-0.689227399014534,
4.13652052554825));
#59816=CARTESIAN_POINT('Ctrl Pts',(11.6345337700541,-0.487594028032435,
3.49411036255383));
#59817=CARTESIAN_POINT('Ctrl Pts',(11.6822496061169,0.161804441490335,3.31626643773886));
#59818=CARTESIAN_POINT('Ctrl Pts',(11.7299654421798,0.662615402711184,3.76630556374144));
#59819=CARTESIAN_POINT('Ctrl Pts',(11.7776812782426,0.554936443973853,4.43094988641136));
#59820=CARTESIAN_POINT('Ctrl Pts',(11.8253971143054,-0.062349190059417,
4.69984629737339));
#59821=CARTESIAN_POINT('Ctrl Pts',(11.8731129503683,-0.622378603495518,
4.32606308493799));
#59822=CARTESIAN_POINT('Ctrl Pts',(11.9208287864311,-0.610868168815925,
3.65285112447858));
#59823=CARTESIAN_POINT('Ctrl Pts',(11.9685446224939,-0.0383880952977111,
3.29843131798253));
#59824=CARTESIAN_POINT('Ctrl Pts',(12.0162604585568,0.569344356809164,3.58827282720487));
#59825=CARTESIAN_POINT('Ctrl Pts',(12.0639762946196,0.654239125569198,4.25620973444184));
#59826=CARTESIAN_POINT('Ctrl Pts',(12.1116921306825,0.138336038556134,4.68886530024737));
#59827=CARTESIAN_POINT('Ctrl Pts',(12.1594079667453,-0.50460316123658,4.48892526128066));
#59828=CARTESIAN_POINT('Ctrl Pts',(12.2071238028081,-0.684157513748105,
3.83999763179777));
#59829=CARTESIAN_POINT('Ctrl Pts',(12.254839638871,-0.235439494268261,3.33800263898788));
#59830=CARTESIAN_POINT('Ctrl Pts',(12.3025554749338,0.429486235500398,3.44393000893412));
#59831=CARTESIAN_POINT('Ctrl Pts',(12.3502713109967,0.700008146713868,4.06050500791278));
#59832=CARTESIAN_POINT('Ctrl Pts',(12.3979871470595,0.327701805790174,4.62151732713591));
#59833=CARTESIAN_POINT('Ctrl Pts',(12.4457029831223,-0.345538145731053,
4.61178072157682));
#59834=CARTESIAN_POINT('Ctrl Pts',(12.4934188191852,-0.701465101239671,
4.04023646593735));
#59835=CARTESIAN_POINT('Ctrl Pts',(12.541134655248,-0.413225860851952,3.43174244451));
#59836=CARTESIAN_POINT('Ctrl Pts',(12.5888504913108,0.254485045853264,3.34508808005552));
#59837=CARTESIAN_POINT('Ctrl Pts',(12.6365663273737,0.688498419195676,3.85984940880123));
#59838=CARTESIAN_POINT('Ctrl Pts',(12.6842821634365,0.490253100280801,4.50331318193882));
#59839=CARTESIAN_POINT('Ctrl Pts',(12.7319979994994,-0.158199184135511,
4.68457671563321));
#59840=CARTESIAN_POINT('Ctrl Pts',(12.7797138355622,-0.661374723552845,
4.23718291779492));
#59841=CARTESIAN_POINT('Ctrl Pts',(12.827429671625,-0.557199677773407,3.57198039701723));
#59842=CARTESIAN_POINT('Ctrl Pts',(12.8751455076879,0.058660405724426,3.29983486358678));
#59843=CARTESIAN_POINT('Ctrl Pts',(12.9228613437507,0.62065173603916,3.67066174834999));
#59844=CARTESIAN_POINT('Ctrl Pts',(12.9705771798135,0.612689027194643,4.34392501712378));
#59845=CARTESIAN_POINT('Ctrl Pts',(13.0182930158764,0.0420845572448178,
4.7013566507062));
#59846=CARTESIAN_POINT('Ctrl Pts',(13.0660088519392,-0.567166809177069,
4.4147216801859));
#59847=CARTESIAN_POINT('Ctrl Pts',(13.1137246880021,-0.655580167748548,
3.74724140943759));
#59848=CARTESIAN_POINT('Ctrl Pts',(13.1614405240649,-0.141964170879043,
3.31187324159358));
#59849=CARTESIAN_POINT('Ctrl Pts',(13.2091563601277,0.502019708508231,3.50842246418533));
#59850=CARTESIAN_POINT('Ctrl Pts',(13.2568721961906,0.684991165006287,4.15639490180834));
#59851=CARTESIAN_POINT('Ctrl Pts',(13.3045880322534,0.238924694735218,4.66074749465585));
#59852=CARTESIAN_POINT('Ctrl Pts',(13.3523038683163,-0.426549999040181,
4.55832549625387));
#59853=CARTESIAN_POINT('Ctrl Pts',(13.4000197043791,-0.700317265381609,
3.94318460369993));
#59854=CARTESIAN_POINT('Ctrl Pts',(13.4477355404419,-0.330972411156884,
3.38021816378559));
#59855=CARTESIAN_POINT('Ctrl Pts',(13.4954513765048,0.342309500898352,3.3864069206363));
#59856=CARTESIAN_POINT('Ctrl Pts',(13.5431672125676,0.70124333116994,3.95606764360979));
#59857=CARTESIAN_POINT('Ctrl Pts',(13.5908830486304,0.416214620412595,4.5660721254426));
#59858=CARTESIAN_POINT('Ctrl Pts',(13.6385988846933,-0.251030380554765,
4.65624386434224));
#59859=CARTESIAN_POINT('Ctrl Pts',(13.6863147207561,-0.687750320459788,
4.14377676500662));
#59860=CARTESIAN_POINT('Ctrl Pts',(13.734030556819,-0.492898558687668,3.49927725007553));
#59861=CARTESIAN_POINT('Ctrl Pts',(13.7817463928818,0.15458953374652,3.31459914100992));
#59862=CARTESIAN_POINT('Ctrl Pts',(13.8294622289446,0.660115678675556,3.75933518700271));
#59863=CARTESIAN_POINT('Ctrl Pts',(13.8771780650075,0.559447438691528,4.42507743387505));
#59864=CARTESIAN_POINT('Ctrl Pts',(13.9248939010703,-0.0549699924482557,
4.7004645325629));
#59865=CARTESIAN_POINT('Ctrl Pts',(13.9726097371331,-0.61890763370075,4.33260427296601));
#59866=CARTESIAN_POINT('Ctrl Pts',(14.020325573196,-0.614492871807821,3.65930839172987));
#59867=CARTESIAN_POINT('Ctrl Pts',(14.0680414092588,-0.0457798505455885,
3.29887485658241));
#59868=CARTESIAN_POINT('Ctrl Pts',(14.1157572453217,0.564973511886205,3.58229532883235));
#59869=CARTESIAN_POINT('Ctrl Pts',(14.1634730813845,0.656903005118004,4.24930042782804));
#59870=CARTESIAN_POINT('Ctrl Pts',(14.2111889174473,0.145588360997982,4.6873691079691));
#59871=CARTESIAN_POINT('Ctrl Pts',(14.2589047535102,-0.499422315191365,
4.49421615972892));
#59872=CARTESIAN_POINT('Ctrl Pts',(14.306620589573,-0.685805794740406,3.8472169075166));
#59873=CARTESIAN_POINT('Ctrl Pts',(14.3543364256359,-0.242403260500786,
3.34052072000184));
#59874=CARTESIAN_POINT('Ctrl Pts',(14.4020522616987,0.423601917710294,3.43943450270243));
#59875=CARTESIAN_POINT('Ctrl Pts',(14.4497680977615,0.700606936934704,4.05312420698026));
#59876=CARTESIAN_POINT('Ctrl Pts',(14.4974839338244,0.334233825748585,4.61802913456711));
#59877=CARTESIAN_POINT('Ctrl Pts',(14.5451997698872,-0.339071350470923,
4.61538839828042));
#59878=CARTESIAN_POINT('Ctrl Pts',(14.59291560595,-0.701002088269634,4.04762702688518));
#59879=CARTESIAN_POINT('Ctrl Pts',(14.6406314420129,-0.419191822106764,
3.43612902386528));
#59880=CARTESIAN_POINT('Ctrl Pts',(14.6883472780757,0.24756874439201,3.34244241450009));
#59881=CARTESIAN_POINT('Ctrl Pts',(14.7360631141386,0.686983123580828,3.85260105372344));
#59882=CARTESIAN_POINT('Ctrl Pts',(14.7837789502014,0.495530329791292,4.49811841333687));
#59883=CARTESIAN_POINT('Ctrl Pts',(14.8314947862642,-0.150975590559777,
4.68620596944608));
#59884=CARTESIAN_POINT('Ctrl Pts',(14.8792106223271,-0.658838303041738,
4.24414002517693));
#59885=CARTESIAN_POINT('Ctrl Pts',(14.9269264583899,-0.561679664310124,
3.57787653921065));
#59886=CARTESIAN_POINT('Ctrl Pts',(14.9746422944528,0.0512780527100071,
3.29925552249156));
#59887=CARTESIAN_POINT('Ctrl Pts',(15.0223581305156,0.617146344912281,3.6641389418082));
#59888=CARTESIAN_POINT('Ctrl Pts',(15.0700739665784,0.616279652564493,4.337448738749));
#59889=CARTESIAN_POINT('Ctrl Pts',(15.1177898026413,0.0494738725853903,
4.70087416658037));
#59890=CARTESIAN_POINT('Ctrl Pts',(15.1655056387041,-0.562764525842253,
4.42067606290572));
#59891=CARTESIAN_POINT('Ctrl Pts',(15.2132214747669,-0.658207600943685,
3.75416465773151));
#59892=CARTESIAN_POINT('Ctrl Pts',(15.2609373108298,-0.14920850827279,3.31340763002542));
#59893=CARTESIAN_POINT('Ctrl Pts',(15.3086531468926,0.496811053413015,3.50315894024854));
#59894=CARTESIAN_POINT('Ctrl Pts',(15.3563689829554,0.686601380328997,4.14916704052379));
#59895=CARTESIAN_POINT('Ctrl Pts',(15.4040848190183,0.245875094968658,4.6581927522561));
#59896=CARTESIAN_POINT('Ctrl Pts',(15.4518006550811,-0.420642073376032,
4.56278993199436));
#59897=CARTESIAN_POINT('Ctrl Pts',(15.499516491144,-0.700877153329261,3.95056845754601));
#59898=CARTESIAN_POINT('Ctrl Pts',(15.5472323272068,-0.337485958999024,
3.3837407291352));
#59899=CARTESIAN_POINT('Ctrl Pts',(15.5949481632696,0.335823784368978,3.38283337152726));
#59900=CARTESIAN_POINT('Ctrl Pts',(15.6426639993325,0.70074137923783,3.94867962517506));
#59901=CARTESIAN_POINT('Ctrl Pts',(15.6903798353953,0.422157383260532,4.56165416869007));
#59902=CARTESIAN_POINT('Ctrl Pts',(15.7380956714582,-0.244100233491204,
4.65885304693675));
#59903=CARTESIAN_POINT('Ctrl Pts',(15.785811507521,-0.686196849863089,4.15101703442422));
#59904=CARTESIAN_POINT('Ctrl Pts',(15.8335273435838,-0.498148340509996,
3.50449975550414));
#59905=CARTESIAN_POINT('Ctrl Pts',(15.8812431796467,0.147357454930898,3.3130079753559));
#59906=CARTESIAN_POINT('Ctrl Pts',(15.9289590157095,0.657542632122849,3.75239154216938));
#59907=CARTESIAN_POINT('Ctrl Pts',(15.9766748517723,0.563896292642505,4.41915776575455));
#59908=CARTESIAN_POINT('Ctrl Pts',(16.0243906878352,-0.0475846890311933,
4.70100496347609));
#59909=CARTESIAN_POINT('Ctrl Pts',(16.072106523898,-0.615367918582998,4.33910851688972));
#59910=CARTESIAN_POINT('Ctrl Pts',(16.1198223599609,-0.618049319847516,
3.66580350138828));
#59911=CARTESIAN_POINT('Ctrl Pts',(16.1675381960237,-0.0531665207849041,
3.29939627283611));
#59912=CARTESIAN_POINT('Ctrl Pts',(16.2152540320865,0.560539912386559,3.57636422711252));
#59913=CARTESIAN_POINT('Ctrl Pts',(16.2629698681494,0.659493918998266,4.24236343010572));
#59914=CARTESIAN_POINT('Ctrl Pts',(16.3106857042122,0.152824512175573,4.68579656599215));
#59915=CARTESIAN_POINT('Ctrl Pts',(16.358401540275,-0.494185995685336,4.49945216299141));
#59916=CARTESIAN_POINT('Ctrl Pts',(16.4061173763379,-0.687377899679438,
3.85445315365633));
#59917=CARTESIAN_POINT('Ctrl Pts',(16.4538332124007,-0.249340101729437,
3.34311205284473));
#59918=CARTESIAN_POINT('Ctrl Pts',(16.5015490484636,0.417670548229327,3.43500126142608));
#59919=CARTESIAN_POINT('Ctrl Pts',(16.5492648845264,0.701127907061643,4.04573750526291));
#59920=CARTESIAN_POINT('Ctrl Pts',(16.5969807205892,0.340728720599694,4.61447229425484));
#59921=CARTESIAN_POINT('Ctrl Pts',(16.6446965566521,-0.3325668927742,4.61892772056098));
#59922=CARTESIAN_POINT('Ctrl Pts',(16.6924123927149,-0.700461211314163,
4.05501229764889));
#59923=CARTESIAN_POINT('Ctrl Pts',(16.7401282287777,-0.425111221523205,
3.4405782353328));
#59924=CARTESIAN_POINT('Ctrl Pts',(16.7878440648406,0.240624944169445,3.3398697873209));
#59925=CARTESIAN_POINT('Ctrl Pts',(16.8355599009034,0.685391521140609,3.84536907102113));
#59926=CARTESIAN_POINT('Ctrl Pts',(16.8832757369663,0.500752518144239,4.49286831610534));
#59927=CARTESIAN_POINT('Ctrl Pts',(16.9309915730291,-0.143735227331884,
4.68775900275617));
#59928=CARTESIAN_POINT('Ctrl Pts',(16.978707409092,-0.656228701898373,4.25107001464348));
#59929=CARTESIAN_POINT('Ctrl Pts',(17.0264232451548,-0.566097262135119,
3.58381956887496));
#59930=CARTESIAN_POINT('Ctrl Pts',(17.0741390812176,0.0438900039728252,
3.29875401676759));
#59931=CARTESIAN_POINT('Ctrl Pts',(17.1218549172805,0.613572404098014,3.65765344111895));
#59932=CARTESIAN_POINT('Ctrl Pts',(17.1695707533433,0.619801824515016,4.33093497816967));
#59933=CARTESIAN_POINT('Ctrl Pts',(17.2172865894061,0.0568576926029748,
4.70031383267802));
#59934=CARTESIAN_POINT('Ctrl Pts',(17.265002425469,-0.558299733294432,4.42658371892475));
#59935=CARTESIAN_POINT('Ctrl Pts',(17.3127182615318,-0.66076192356197,3.76111521224867));
#59936=CARTESIAN_POINT('Ctrl Pts',(17.3604340975947,-0.156436272293483,
3.31501828187956));
#59937=CARTESIAN_POINT('Ctrl Pts',(17.4081499336575,0.491547214903555,3.49795060305896));
#59938=CARTESIAN_POINT('Ctrl Pts',(17.4558657697204,0.688135331228569,4.14192261047223));
#59939=CARTESIAN_POINT('Ctrl Pts',(17.5035816057831,0.252798184563325,4.65556490092881));
#59940=CARTESIAN_POINT('Ctrl Pts',(17.551297441846,-0.414687424786488,4.56719185569987));
#59941=CARTESIAN_POINT('Ctrl Pts',(17.5990132779088,-0.701359191168653,
3.95795780201324));
#59942=CARTESIAN_POINT('Ctrl Pts',(17.6467291139717,-0.343962020502345,
3.38733174564023));
#59943=CARTESIAN_POINT('Ctrl Pts',(17.6944449500345,0.329300766127249,3.37932837435862));
#59944=CARTESIAN_POINT('Ctrl Pts',(17.7421607860974,0.700161592278611,3.94129730716402));
#59945=CARTESIAN_POINT('Ctrl Pts',(17.7898766221602,0.428053254869629,4.55717382605774));
#59946=CARTESIAN_POINT('Ctrl Pts',(17.837592458223,-0.23714297293205,4.66138904726133));
#59947=CARTESIAN_POINT('Ctrl Pts',(17.8853082942859,-0.684567159776581,
4.15824052958626));
#59948=CARTESIAN_POINT('Ctrl Pts',(17.9330241303487,-0.503342790378573,
3.50977729874859));
#59949=CARTESIAN_POINT('Ctrl Pts',(17.9807399664116,0.140109008348428,3.31149311751593));
#59950=CARTESIAN_POINT('Ctrl Pts',(18.0284558024744,0.654896548854854,3.7454754005085));
#59951=CARTESIAN_POINT('Ctrl Pts',(18.0761716385372,0.568282511669218,4.41319153957849));
#59952=CARTESIAN_POINT('Ctrl Pts',(18.1238874746001,-0.040194100132671,
4.70146753008449));
#59953=CARTESIAN_POINT('Ctrl Pts',(18.1716033106629,-0.611759851316993,
4.34557509424858));
#59954=CARTESIAN_POINT('Ctrl Pts',(18.2193191467258,-0.621537117901666,
3.67233573200791));
#59955=CARTESIAN_POINT('Ctrl Pts',(18.2670349827885,-0.0605472855394143,
3.29999550882718));
#59956=CARTESIAN_POINT('Ctrl Pts',(18.3147508188514,0.556044050773433,3.57048018084402));
#59957=CARTESIAN_POINT('Ctrl Pts',(18.3624666549143,0.662011579423562,4.23539951180373));
#59958=CARTESIAN_POINT('Ctrl Pts',(18.4101824909771,0.160043688331546,4.684147848987));
#59959=CARTESIAN_POINT('Ctrl Pts',(18.4578983270399,-0.488894784343999,
4.50463268947774));
#59960=CARTESIAN_POINT('Ctrl Pts',(18.5056141631028,-0.68887365394326,3.86170556644909));
#59961=CARTESIAN_POINT('Ctrl Pts',(18.5533299991656,-0.256249247442801,
3.34577634968359));
#59962=CARTESIAN_POINT('Ctrl Pts',(18.6010458352284,0.41169278588589,3.4306307775285));
#59963=CARTESIAN_POINT('Ctrl Pts',(18.6487616712913,0.701570999227752,4.03834572324048));
#59964=CARTESIAN_POINT('Ctrl Pts',(18.6964775073541,0.347185768921481,4.6108472012761));
#59965=CARTESIAN_POINT('Ctrl Pts',(18.744193343417,-0.326025495125306,4.62239829528727));
#59966=CARTESIAN_POINT('Ctrl Pts',(18.7919091794798,-0.699842530451103,
4.06239145790787));
#59967=CARTESIAN_POINT('Ctrl Pts',(18.8396250155426,-0.430983401602837,
3.44508958471478));
#59968=CARTESIAN_POINT('Ctrl Pts',(18.8873408516055,0.233654416470602,3.33737048427408));
#59969=CARTESIAN_POINT('Ctrl Pts',(18.9350566876683,0.683723788661416,3.83815426398688));
#59970=CARTESIAN_POINT('Ctrl Pts',(18.9827725237312,0.505919085286118,4.48756347340344));
#59971=CARTESIAN_POINT('Ctrl Pts',(19.030488359794,-0.136478898681533,4.68923564305365));
#59972=CARTESIAN_POINT('Ctrl Pts',(19.0782041958568,-0.653546209976322,
4.2579721164561));
#59973=CARTESIAN_POINT('Ctrl Pts',(19.1259200319197,-0.570451980578726,
3.58980882586423));
#59974=CARTESIAN_POINT('Ctrl Pts',(19.1736358679825,0.0364970801727598,
3.29833040216201));
#59975=CARTESIAN_POINT('Ctrl Pts',(19.2213517040453,0.609930310515188,3.65120596658116));
#59976=CARTESIAN_POINT('Ctrl Pts',(19.2690675401082,0.623255151928734,4.32438445905389));
#59977=CARTESIAN_POINT('Ctrl Pts',(19.316783376171,0.0642351969327414,4.69967571095415));
#59978=CARTESIAN_POINT('Ctrl Pts',(19.3644992122339,-0.553772927074266,
4.43244399258532));
#59979=CARTESIAN_POINT('Ctrl Pts',(19.4122150482967,-0.663242852612724,
3.76809229994096));
#59980=CARTESIAN_POINT('Ctrl Pts',(19.4599308843595,-0.163646658734412,
3.3167050201661));
#59981=CARTESIAN_POINT('Ctrl Pts',(19.5076467204224,0.486228775054438,3.49279802752061));
#59982=CARTESIAN_POINT('Ctrl Pts',(19.5553625564852,0.689592852244711,4.13466242315333));
#59983=CARTESIAN_POINT('Ctrl Pts',(19.6030783925481,0.259693185238344,4.65286421968052));
#59984=CARTESIAN_POINT('Ctrl Pts',(19.6507942286109,-0.408686697131164,
4.57153080275077));
#59985=CARTESIAN_POINT('Ctrl Pts',(19.6985100646738,-0.701763358503738,
3.96535177039745));
#59986=CARTESIAN_POINT('Ctrl Pts',(19.7462259007365,-0.350399813749482,
3.39099090115443));
#59987=CARTESIAN_POINT('Ctrl Pts',(19.7939417367994,0.322741052541778,3.37589215469092));
#59988=CARTESIAN_POINT('Ctrl Pts',(19.8416575728622,0.699504257835039,3.93392181877779));
#59989=CARTESIAN_POINT('Ctrl Pts',(19.8893734089251,0.433901159015506,4.55263101135276));
#59990=CARTESIAN_POINT('Ctrl Pts',(19.9370892449879,-0.23015857608315,4.663852686053));
#59991=CARTESIAN_POINT('Ctrl Pts',(19.9848050810507,-0.682862933423436,
4.16544436654047));
#59992=CARTESIAN_POINT('Ctrl Pts',(20.0325209171136,-0.508478494849655,
3.51511322409123));
#59993=CARTESIAN_POINT('Ctrl Pts',(20.0802367531764,0.132839643288252,3.31004731418368));
#59994=CARTESIAN_POINT('Ctrl Pts',(20.1279525892393,0.652187835720725,3.73860154375571));
#59995=CARTESIAN_POINT('Ctrl Pts',(20.1756684253021,0.572586513039731,4.4071529569233));
#59996=CARTESIAN_POINT('Ctrl Pts',(20.2233842613649,-0.0327629883405684,
4.70190215105461));
#59997=CARTESIAN_POINT('Ctrl Pts',(20.2711000974278,-0.608151935097038,
4.35190888358257));
#59998=CARTESIAN_POINT('Ctrl Pts',(20.3188159334906,-0.624827148513498,
3.67908301574286));
#59999=CARTESIAN_POINT('Ctrl Pts',(20.3665317695535,-0.0681655280739813,
3.30033184185188));
#60000=CARTESIAN_POINT('Ctrl Pts',(20.4142476056163,0.551956769749184,3.56531418539817));
#60001=CARTESIAN_POINT('Ctrl Pts',(20.4540108023353,0.644905999548395,4.11665253813788));
#60002=CARTESIAN_POINT('Ctrl Pts',(20.4858213597105,0.416382673412033,4.45708139504444));
#60003=CARTESIAN_POINT('Ctrl Pts',(20.509679277742,0.148137151166912,4.60177085628536));
#60004=CARTESIAN_POINT('Ctrl Pts',(20.5335371957734,-0.159214575149101,
4.59858486262053));
#60005=CARTESIAN_POINT('Ctrl Pts',(20.5573951138048,-0.426074836374489,
4.44942877587387));
#60006=CARTESIAN_POINT('Ctrl Pts',(20.5812530318362,-0.589577924844292,
4.19016123618585));
#60007=CARTESIAN_POINT('Ctrl Pts',(20.6051109498677,-0.608473233900696,
3.88450759853215));
#60008=CARTESIAN_POINT('Ctrl Pts',(20.6289688678991,-0.478813304308425,
3.60703485797333));
#60009=CARTESIAN_POINT('Ctrl Pts',(20.6528267859305,-0.231947052182395,
3.42568465323223));
#60010=CARTESIAN_POINT('Ctrl Pts',(20.6766847039619,0.0715712039811096,
3.38475332414555));
#60011=CARTESIAN_POINT('Ctrl Pts',(20.7005426219933,0.357622970648114,3.49427550111266));
#60012=CARTESIAN_POINT('Ctrl Pts',(20.7244005400248,0.556207844932749,3.72745636179159));
#60013=CARTESIAN_POINT('Ctrl Pts',(20.7482584580561,0.618794460414918,4.02728407199912));
#60014=CARTESIAN_POINT('Ctrl Pts',(20.7721163760876,0.530063832205264,4.32043875618714));
#60015=CARTESIAN_POINT('Ctrl Pts',(20.7959742941189,0.311720881859749,4.53523813880796));
#60016=CARTESIAN_POINT('Ctrl Pts',(20.8198322121505,0.01715224242355,4.619156844639));
#60017=CARTESIAN_POINT('Ctrl Pts',(20.8436901301818,-0.281609823618225,
4.55167503361081));
#60018=CARTESIAN_POINT('Ctrl Pts',(20.8675480482133,-0.511511021444125,
4.34929354512778));
#60019=CARTESIAN_POINT('Ctrl Pts',(20.8914059662447,-0.616333626991818,
4.06150032559224));
#60020=CARTESIAN_POINT('Ctrl Pts',(20.9152638842761,-0.570445985619195,
3.75866857192897));
#60021=CARTESIAN_POINT('Ctrl Pts',(20.9391218023075,-0.385068702031786,
3.51484894167474));
#60022=CARTESIAN_POINT('Ctrl Pts',(20.9629797203389,-0.105531663562905,
3.38966195221662));
#60023=CARTESIAN_POINT('Ctrl Pts',(20.9868376383704,0.199810758127152,3.41371924506628));
#60024=CARTESIAN_POINT('Ctrl Pts',(21.0106955564018,0.456293997792742,3.58113815016051));
#60025=CARTESIAN_POINT('Ctrl Pts',(21.0345534744332,0.60120093052663,3.85098018832832));
#60026=CARTESIAN_POINT('Ctrl Pts',(21.0584113924646,0.599097856858477,4.15726162902184));
#60027=CARTESIAN_POINT('Ctrl Pts',(21.082269310496,0.450499039416452,4.42508831804098));
#60028=CARTESIAN_POINT('Ctrl Pts',(21.1061272285275,0.191740934787398,4.58896933394457));
#60029=CARTESIAN_POINT('Ctrl Pts',(21.1299851465589,-0.113903050943465,
4.60883130459215));
#60030=CARTESIAN_POINT('Ctrl Pts',(21.1538430645903,-0.391694638258801,
4.47981743698434));
#60031=CARTESIAN_POINT('Ctrl Pts',(21.1777009826217,-0.573706216867813,
4.23347513609622));
#60032=CARTESIAN_POINT('Ctrl Pts',(21.2015589006531,-0.615430998064313,
3.9300418046833));
#60033=CARTESIAN_POINT('Ctrl Pts',(21.2254168186846,-0.506666136201032,
3.64371515765586));
#60034=CARTESIAN_POINT('Ctrl Pts',(21.2492747367159,-0.27400760274365,3.44450985958179));
#60035=CARTESIAN_POINT('Ctrl Pts',(21.2731326547474,0.0256532534100022,
3.38113703208972));
#60036=CARTESIAN_POINT('Ctrl Pts',(21.2969905727788,0.319041190319967,3.46909305773936));
#60037=CARTESIAN_POINT('Ctrl Pts',(21.3208484908102,0.534414865691478,3.68687029238709));
#60038=CARTESIAN_POINT('Ctrl Pts',(21.3447064088416,0.619109549231529,3.98121627002784));
#60039=CARTESIAN_POINT('Ctrl Pts',(21.3685643268731,0.552415083779586,4.28015538130547));
#60040=CARTESIAN_POINT('Ctrl Pts',(21.3924222449044,0.350640082858436,4.51058887057447));
#60041=CARTESIAN_POINT('Ctrl Pts',(21.4162801629359,0.0631240304344945,
4.61616947282646));
#60042=CARTESIAN_POINT('Ctrl Pts',(21.4401380809673,-0.239827566894842,
4.57107985485291));
#60043=CARTESIAN_POINT('Ctrl Pts',(21.4639959989987,-0.484134791346583,
4.38634565646493));
#60044=CARTESIAN_POINT('Ctrl Pts',(21.4878539170302,-0.610057871747176,
4.10713942122688));
#60045=CARTESIAN_POINT('Ctrl Pts',(21.5117118350615,-0.586805184862796,
3.80173467907963));
#60046=CARTESIAN_POINT('Ctrl Pts',(21.535569753093,-0.420062646027161,3.5448112085363));
#60047=CARTESIAN_POINT('Ctrl Pts',(21.5594276711244,-0.150603347961132,
3.39919379659958));
#60048=CARTESIAN_POINT('Ctrl Pts',(21.5832855891558,0.155682571034224,3.40048986702667));
#60049=CARTESIAN_POINT('Ctrl Pts',(21.6071435071872,0.423899860703612,3.54838249529388));
#60050=CARTESIAN_POINT('Ctrl Pts',(21.6310014252187,0.588462087630599,3.80670790527556));
#60051=CARTESIAN_POINT('Ctrl Pts',(21.6548593432501,0.609129304746478,4.11229849758833));
#60052=CARTESIAN_POINT('Ctrl Pts',(21.6787172612815,0.480847814502724,4.39042904829107));
#60053=CARTESIAN_POINT('Ctrl Pts',(21.7025751793129,0.234985935581564,4.57308906161293));
#60054=CARTESIAN_POINT('Ctrl Pts',(21.7264330973443,-0.0683364054776661,
4.61561318873779));
#60055=CARTESIAN_POINT('Ctrl Pts',(21.7502910153758,-0.35494863395129,4.5076031222497));
#60056=CARTESIAN_POINT('Ctrl Pts',(21.7741489334072,-0.554766252817153,
4.2754702655401));
#60057=CARTESIAN_POINT('Ctrl Pts',(21.7980068514386,-0.618928411339905,
3.9759774252466));
#60058=CARTESIAN_POINT('Ctrl Pts',(21.82186476947,-0.531745714018629,3.68235875884208));
#60059=CARTESIAN_POINT('Ctrl Pts',(21.8457226875014,-0.314536705157368,
3.46641202827438));
#60060=CARTESIAN_POINT('Ctrl Pts',(21.8695806055329,-0.0204149040773093,
3.3809420914381));
#60061=CARTESIAN_POINT('Ctrl Pts',(21.8934385235643,0.278698897140474,3.44684867604406));
#60062=CARTESIAN_POINT('Ctrl Pts',(21.9172964415957,0.509663226401888,3.6480158268968));
#60063=CARTESIAN_POINT('Ctrl Pts',(21.9411543596271,0.616001013860485,3.93525269592965));
#60064=CARTESIAN_POINT('Ctrl Pts',(21.9650122776585,0.571709773899469,4.23832204448885));
#60065=CARTESIAN_POINT('Ctrl Pts',(21.98887019569,0.387619921158457,4.48311516140836));
#60066=CARTESIAN_POINT('Ctrl Pts',(22.0127281137213,0.108746439139576,4.60977346157076));
#60067=CARTESIAN_POINT('Ctrl Pts',(22.0365860317528,-0.196718509442517,
4.5873255404835));
#60068=CARTESIAN_POINT('Ctrl Pts',(22.0604439497842,-0.454080423961193,
4.42126052632156));
#60069=CARTESIAN_POINT('Ctrl Pts',(22.0843018678156,-0.600407305919173,
4.15218583856754));
#60070=CARTESIAN_POINT('Ctrl Pts',(22.1081597858471,-0.599918246812857,
3.84589756782496));
#60071=CARTESIAN_POINT('Ctrl Pts',(22.1320177038785,-0.452732834916613,
3.57729153941473));
#60072=CARTESIAN_POINT('Ctrl Pts',(22.1558756219099,-0.194841912687001,
3.41204924396571));
#60073=CARTESIAN_POINT('Ctrl Pts',(22.1797335399413,0.110693164578993,3.39057692382254));
#60074=CARTESIAN_POINT('Ctrl Pts',(22.2035914579728,0.389160747889314,3.51812514615901));
#60075=CARTESIAN_POINT('Ctrl Pts',(22.2274493760041,0.572467927805029,3.76350489626149));
#60076=CARTESIAN_POINT('Ctrl Pts',(22.2513072940356,0.615791105677536,4.06671414123586));
#60077=CARTESIAN_POINT('Ctrl Pts',(22.2751652120669,0.508536584364246,4.35360996140145));
#60078=CARTESIAN_POINT('Ctrl Pts',(22.2990231300984,0.276931015980992,4.55403851389998));
#60079=CARTESIAN_POINT('Ctrl Pts',(22.3228810481298,-0.0223917293827815,
4.61898955797298));
#60080=CARTESIAN_POINT('Ctrl Pts',(22.3467389661613,-0.31623908674035,4.53258079431836));
#60081=CARTESIAN_POINT('Ctrl Pts',(22.3705968841927,-0.532757373651304,
4.31594151899069));
#60082=CARTESIAN_POINT('Ctrl Pts',(22.3944548022241,-0.619001969851995,
4.02204593667267));
#60083=CARTESIAN_POINT('Ctrl Pts',(22.4183127202555,-0.553883724721699,
3.72275952141814));
#60084=CARTESIAN_POINT('Ctrl Pts',(22.4421706382869,-0.35332581843718,3.49126595675675));
#60085=CARTESIAN_POINT('Ctrl Pts',(22.4660285563184,-0.0663701307507445,
3.38417172009386));
#60086=CARTESIAN_POINT('Ctrl Pts',(22.4898864743497,0.236814872379406,3.42766427875767));
#60087=CARTESIAN_POINT('Ctrl Pts',(22.5137443923812,0.482092168510832,3.61110849992699));
#60088=CARTESIAN_POINT('Ctrl Pts',(22.5376023104126,0.609484835267769,3.88964730767638));
#60089=CARTESIAN_POINT('Ctrl Pts',(22.561460228444,0.587841786482003,4.19517031382209));
#60090=CARTESIAN_POINT('Ctrl Pts',(22.5853181464754,0.422455543015367,4.45296893898932));
#60091=CARTESIAN_POINT('Ctrl Pts',(22.6091760645069,0.153767157666155,4.60000417439789));
#60092=CARTESIAN_POINT('Ctrl Pts',(22.6330339825383,-0.152521006364708,
4.60032232020799));
#60093=CARTESIAN_POINT('Ctrl Pts',(22.6568919005697,-0.421514535902825,
4.45384478734481));
#60094=CARTESIAN_POINT('Ctrl Pts',(22.6807498186011,-0.587434568575047,
4.19639082134502));
#60095=CARTESIAN_POINT('Ctrl Pts',(22.7046077366325,-0.60971407867596,3.89091209973551));
#60096=CARTESIAN_POINT('Ctrl Pts',(22.728465654664,-0.482895786937606,3.61211183522625));
#60097=CARTESIAN_POINT('Ctrl Pts',(22.7523235726954,-0.23800784887647,3.4281541921173));
#60098=CARTESIAN_POINT('Ctrl Pts',(22.7761814907268,0.0651013135850054,
3.38404091701771));
#60099=CARTESIAN_POINT('Ctrl Pts',(22.8000394087582,0.352249768808992,3.49052260401466));
#60100=CARTESIAN_POINT('Ctrl Pts',(22.8238973267896,0.553345940411564,3.72163220123786));
#60101=CARTESIAN_POINT('Ctrl Pts',(22.8398026054772,0.597082876783669,3.92101540361374));
#60102=CARTESIAN_POINT('Ctrl Pts',(22.847755244821,0.593766187829899,4.01991291515446));
#60103=CARTESIAN_POINT('',(22.8,0.337479661717902,3.51106003648017));
#60104=CARTESIAN_POINT('Ctrl Pts',(22.8,0.337504360408405,3.51101527402275));
#60105=CARTESIAN_POINT('Ctrl Pts',(22.8,0.337610992569967,3.51114843896934));
#60106=CARTESIAN_POINT('Ctrl Pts',(22.8,0.337717562131928,3.51128164981369));
#60107=CARTESIAN_POINT('Ctrl Pts',(22.8,0.337824069051012,3.51141490653789));
#60108=CARTESIAN_POINT('Ctrl Pts',(22.8,0.354145371784291,3.53183539523119));
#60109=CARTESIAN_POINT('Ctrl Pts',(22.8,0.368999739942303,3.55333386321799));
#60110=CARTESIAN_POINT('Ctrl Pts',(22.8,0.382262544471458,3.57576050230915));
#60111=CARTESIAN_POINT('Ctrl Pts',(22.8,0.395177725624396,3.59759933027929));
#60112=CARTESIAN_POINT('Ctrl Pts',(22.8,0.406583379369087,3.62031953557487));
#60113=CARTESIAN_POINT('Ctrl Pts',(22.8,0.416319965152677,3.64376476659274));
#60114=CARTESIAN_POINT('Ctrl Pts',(22.8,0.420499854003763,3.65382973822867));
#60115=CARTESIAN_POINT('Ctrl Pts',(22.8,0.424371599987778,3.66402799385056));
#60116=CARTESIAN_POINT('Ctrl Pts',(22.8,0.42792023461967,3.67434527679585));
#60117=CARTESIAN_POINT('Ctrl Pts',(22.8,0.430015882150509,3.68043815216119));
#60118=CARTESIAN_POINT('Ctrl Pts',(22.8,0.431995626466768,3.68656321156818));
#60119=CARTESIAN_POINT('Ctrl Pts',(22.8,0.433857425300493,3.69271766785326));
#60120=CARTESIAN_POINT('Ctrl Pts',(22.8,0.440667704273582,3.71523007009016));
#60121=CARTESIAN_POINT('Ctrl Pts',(22.8,0.445903532435623,3.73813926926309));
#60122=CARTESIAN_POINT('Ctrl Pts',(22.8,0.449441836754149,3.76130640751661));
#60123=CARTESIAN_POINT('Ctrl Pts',(22.8,0.450038513826676,3.76521316594877));
#60124=CARTESIAN_POINT('Ctrl Pts',(22.8,0.450586822418701,3.76912718643627));
#60125=CARTESIAN_POINT('Ctrl Pts',(22.8,0.451086059471329,3.77304770583064));
#60126=CARTESIAN_POINT('Ctrl Pts',(22.8,0.453684096906641,3.79345015011803));
#60127=CARTESIAN_POINT('Ctrl Pts',(22.8,0.454954433743694,3.81403106227893));
#60128=CARTESIAN_POINT('Ctrl Pts',(22.8,0.45484641916779,3.83463783350426));
#60129=CARTESIAN_POINT('Ctrl Pts',(22.8,0.454808390965019,3.84189276616533));
#60130=CARTESIAN_POINT('Ctrl Pts',(22.8,0.454599381710613,3.84915061719132));
#60131=CARTESIAN_POINT('Ctrl Pts',(22.8,0.454216814112443,3.8564037154462));
#60132=CARTESIAN_POINT('Ctrl Pts',(22.8,0.453866695925276,3.86304160538904));
#60133=CARTESIAN_POINT('Ctrl Pts',(22.8,0.453371644107099,3.86966645154658));
#60134=CARTESIAN_POINT('Ctrl Pts',(22.8,0.452731182295137,3.87626933737115));
#60135=CARTESIAN_POINT('Ctrl Pts',(22.8,0.450713457978438,3.89707120727158));
#60136=CARTESIAN_POINT('Ctrl Pts',(22.8,0.447253508643,3.9176725514372));
#60137=CARTESIAN_POINT('Ctrl Pts',(22.8,0.442312061254715,3.9379035771693));
#60138=CARTESIAN_POINT('Ctrl Pts',(22.8,0.437564183511961,3.95734209977996));
#60139=CARTESIAN_POINT('Ctrl Pts',(22.8,0.431447509288203,3.97643919003209));
#60140=CARTESIAN_POINT('Ctrl Pts',(22.8,0.423915075143768,3.9949978423605));
#60141=CARTESIAN_POINT('Ctrl Pts',(22.8,0.421325190817866,4.00137888225459));
#60142=CARTESIAN_POINT('Ctrl Pts',(22.8,0.418567902041021,4.00769582483512));
#60143=CARTESIAN_POINT('Ctrl Pts',(22.8,0.415641328671541,4.01393920819689));
#60144=CARTESIAN_POINT('Ctrl Pts',(22.6211545887425,-1.51173456864708E-7,
4.59404872180247));
#60145=CARTESIAN_POINT('Ctrl Pts',(22.6251143866744,-0.0492822808754852,
4.59404929162283));
#60146=CARTESIAN_POINT('Ctrl Pts',(22.6290741846063,-0.0985642856931001,
4.58798571459226));
#60147=CARTESIAN_POINT('Ctrl Pts',(22.6330339825383,-0.14630523394925,4.57585637376244));
#60148=CARTESIAN_POINT('Ctrl Pts',(22.6409866218821,-0.242185516210759,
4.55149647592026));
#60149=CARTESIAN_POINT('Ctrl Pts',(22.6489392612259,-0.331850026056775,
4.50267063163255));
#60150=CARTESIAN_POINT('Ctrl Pts',(22.6568919005697,-0.404335619758509,
4.43534871515538));
#60151=CARTESIAN_POINT('Ctrl Pts',(22.6648445399135,-0.476821213460227,
4.36802679867822));
#60152=CARTESIAN_POINT('Ctrl Pts',(22.6727971792573,-0.532127891017642,
4.28220881001161));
#60153=CARTESIAN_POINT('Ctrl Pts',(22.6807498186011,-0.563494481479829,
4.18838669541007));
#60154=CARTESIAN_POINT('Ctrl Pts',(22.6887024579449,-0.594861071942019,
4.09456458080851));
#60155=CARTESIAN_POINT('Ctrl Pts',(22.6966550972887,-0.602287575308989,
3.99273834027202));
#60156=CARTESIAN_POINT('Ctrl Pts',(22.7046077366325,-0.584864445036083,
3.89535850925222));
#60157=CARTESIAN_POINT('Ctrl Pts',(22.7125603759763,-0.567441314763176,
3.79797867823242));
#60158=CARTESIAN_POINT('Ctrl Pts',(22.7205130153201,-0.525168550850394,
3.70504525672934));
#60159=CARTESIAN_POINT('Ctrl Pts',(22.7284656546639,-0.463217512550482,
3.62791893879298));
#60160=CARTESIAN_POINT('Ctrl Pts',(22.7364182940078,-0.401266474250563,
3.5507926208566));
#60161=CARTESIAN_POINT('Ctrl Pts',(22.7443709333516,-0.319637161563486,
3.48947340648693));
#60162=CARTESIAN_POINT('Ctrl Pts',(22.7523235726954,-0.228304311476372,
3.45146158678551));
#60163=CARTESIAN_POINT('Ctrl Pts',(22.7602762120392,-0.136971461389268,
3.41344976708409));
#60164=CARTESIAN_POINT('Ctrl Pts',(22.768228851383,-0.0359350739021178,
3.3987453420509));
#60165=CARTESIAN_POINT('Ctrl Pts',(22.7761814907268,0.062441195712126,3.40914007736714));
#60166=CARTESIAN_POINT('Ctrl Pts',(22.7841209938178,0.160654966376612,3.41951764255099));
#60167=CARTESIAN_POINT('Ctrl Pts',(22.7920604969089,0.256217399931083,3.45491151845628));
#60168=CARTESIAN_POINT('Ctrl Pts',(22.8,0.337504360408238,3.51101527402264));
#60169=CARTESIAN_POINT('Ctrl Pts',(4.,-0.219914231356244,4.35301468169996));
#60170=CARTESIAN_POINT('Ctrl Pts',(4.00793950309107,-0.278596966840389,
4.31645650682028));
#60171=CARTESIAN_POINT('Ctrl Pts',(4.02383164552594,-0.377405665439666,
4.21337674819164));
#60172=CARTESIAN_POINT('Ctrl Pts',(4.04767642730463,-0.433534992178268,
4.00656196868444));
#60173=CARTESIAN_POINT('Ctrl Pts',(4.07153434533603,-0.383670022685343,
3.79803920418254));
#60174=CARTESIAN_POINT('Ctrl Pts',(4.09539226336747,-0.239994733226421,
3.63889579340969));
#60175=CARTESIAN_POINT('Ctrl Pts',(4.11925018139887,-0.0376302499649443,
3.56805514133307));
#60176=CARTESIAN_POINT('Ctrl Pts',(4.1431080994303,0.173933765839147,3.60283521426327));
#60177=CARTESIAN_POINT('Ctrl Pts',(4.16696601746172,0.342967344134064,3.73473372141871));
#60178=CARTESIAN_POINT('Ctrl Pts',(4.19082393549313,0.428135478754777,3.93149662217858));
#60179=CARTESIAN_POINT('Ctrl Pts',(4.21468185352456,0.40861313688017,4.1450106963618));
#60180=CARTESIAN_POINT('Ctrl Pts',(4.23853977155597,0.289173588337559,4.32306558264197));
#60181=CARTESIAN_POINT('Ctrl Pts',(4.25811226835493,0.13317859508208,4.40432939198872));
#60182=CARTESIAN_POINT('Ctrl Pts',(4.26973212581007,0.0319512750557707,
4.41584666103033));
#60183=CARTESIAN_POINT('Ctrl Pts',(4.2733993439214,2.51014653359152E-6,
4.41583996132385));
#60184=CARTESIAN_POINT('Origin',(3.42660065607856,0.,4.));
#60185=CARTESIAN_POINT('Ctrl Pts',(4.,-0.219892372743211,3.64701365460636));
#60186=CARTESIAN_POINT('Ctrl Pts',(4.00795263934381,-0.161099076858729,
3.61038844940468));
#60187=CARTESIAN_POINT('Ctrl Pts',(4.02385791803142,-0.0249198690254346,
3.56711791692558));
#60188=CARTESIAN_POINT('Ctrl Pts',(4.04771583606284,0.185569069288609,3.60813812632505));
#60189=CARTESIAN_POINT('Ctrl Pts',(4.07157375409426,0.350624105231944,3.74494568050885));
#60190=CARTESIAN_POINT('Ctrl Pts',(4.09543167212568,0.429971014252744,3.94413788601839));
#60191=CARTESIAN_POINT('Ctrl Pts',(4.1192895901571,0.40416308778273,4.15698104289539));
#60192=CARTESIAN_POINT('Ctrl Pts',(4.14314750818851,0.279534313346206,4.3314427366163));
#60193=CARTESIAN_POINT('Ctrl Pts',(4.16225119682902,0.125004509401131,4.40624063703925));
#60194=CARTESIAN_POINT('Ctrl Pts',(4.1734022461257,0.0278694809177792,4.41585864517498));
#60195=CARTESIAN_POINT('Ctrl Pts',(4.17660065607858,5.88453344126799E-6,
4.41584444980552));
#60196=CARTESIAN_POINT('Ctrl Pts',(3.95224475517896,-0.314128184302177,
3.49573985500833));
#60197=CARTESIAN_POINT('Ctrl Pts',(3.96019739452277,-0.230138771413741,
3.44341876234755));
#60198=CARTESIAN_POINT('Ctrl Pts',(3.97610267321038,-0.0355993848822847,
3.38160445914153));
#60199=CARTESIAN_POINT('Ctrl Pts',(3.9999605912418,0.265095483172694,3.44020405374152));
#60200=CARTESIAN_POINT('Ctrl Pts',(4.02381850927322,0.500885556761892,3.63564106712445));
#60201=CARTESIAN_POINT('Ctrl Pts',(4.04767642730465,0.614236921112272,3.92019793948569));
#60202=CARTESIAN_POINT('Ctrl Pts',(4.07153434533605,0.577368897990231,4.22425593648149));
#60203=CARTESIAN_POINT('Ctrl Pts',(4.09539226336749,0.399329932212592,4.47348393104611));
#60204=CARTESIAN_POINT('Ctrl Pts',(4.11925018139889,0.123637843932736,4.60692867011962));
#60205=CARTESIAN_POINT('Ctrl Pts',(4.14310809943032,-0.182283847264271,
4.59196468982869));
#60206=CARTESIAN_POINT('Ctrl Pts',(4.16696601746173,-0.443633876576525,
4.43224822622665));
#60207=CARTESIAN_POINT('Ctrl Pts',(4.19082393549315,-0.596502436238336,
4.16683582239239));
#60208=CARTESIAN_POINT('Ctrl Pts',(4.21468185352458,-0.603510379797736,
3.86062723727387));
#60209=CARTESIAN_POINT('Ctrl Pts',(4.23853977155598,-0.462943343075553,
3.58849923641164));
#60210=CARTESIAN_POINT('Ctrl Pts',(4.26239768958742,-0.209174182705692,
3.41699430327496));
#60211=CARTESIAN_POINT('Ctrl Pts',(4.28625560761882,0.0957438341235747,
3.38805018506757));
#60212=CARTESIAN_POINT('Ctrl Pts',(4.31011352565025,0.377249837899377,3.50874444390425));
#60213=CARTESIAN_POINT('Ctrl Pts',(4.33397144368167,0.566508000142931,3.7495640793295));
#60214=CARTESIAN_POINT('Ctrl Pts',(4.35782936171309,0.617239514437223,4.05162211295782));
#60215=CARTESIAN_POINT('Ctrl Pts',(4.3816872797445,0.517039159770137,4.34105713706075));
#60216=CARTESIAN_POINT('Ctrl Pts',(4.40554519777592,0.290408643717306,4.54709439922074));
#60217=CARTESIAN_POINT('Ctrl Pts',(4.42940311580735,-0.00723469473045889,
4.61935217913086));
#60218=CARTESIAN_POINT('Ctrl Pts',(4.45326103383876,-0.303108954077165,
4.54016147994594));
#60219=CARTESIAN_POINT('Ctrl Pts',(4.47711895187019,-0.524864817190473,
4.3288865854667));
#60220=CARTESIAN_POINT('Ctrl Pts',(4.5009768699016,-0.618276935702851,4.03718996201469));
#60221=CARTESIAN_POINT('Ctrl Pts',(4.52483478793302,-0.560503501787052,
3.7363993798876));
#60222=CARTESIAN_POINT('Ctrl Pts',(4.54869270596444,-0.365671693940747,
3.50006632967672));
#60223=CARTESIAN_POINT('Ctrl Pts',(4.57255062399586,-0.0814231961944085,
3.38598067979976));
#60224=CARTESIAN_POINT('Ctrl Pts',(4.59640854202727,0.222735490926488,3.42203947925158));
#60225=CARTESIAN_POINT('Ctrl Pts',(4.6202664600587,0.472429283332598,3.59942536936051));
#60226=CARTESIAN_POINT('Ctrl Pts',(4.64412437809011,0.606601247243452,3.87476266809168));
#60227=CARTESIAN_POINT('Ctrl Pts',(4.66798229612153,0.592442682719785,4.18072390587243));
#60228=CARTESIAN_POINT('Ctrl Pts',(4.69184021415295,0.433415744455024,4.44249322584619));
#60229=CARTESIAN_POINT('Ctrl Pts',(4.71569813218437,0.168406850663934,4.59606089882753));
#60230=CARTESIAN_POINT('Ctrl Pts',(4.7395560502158,-0.1377821054254,4.60387544567241));
#60231=CARTESIAN_POINT('Ctrl Pts',(4.7634139682472,-0.410279583628813,4.46402599681362));
#60232=CARTESIAN_POINT('Ctrl Pts',(4.78727188627863,-0.582452527843622,
4.21070955191949));
#60233=CARTESIAN_POINT('Ctrl Pts',(4.81112980431005,-0.612199963312297,
3.9058688819681));
#60234=CARTESIAN_POINT('Ctrl Pts',(4.83498772234147,-0.492247831758966,
3.62404583445569));
#60235=CARTESIAN_POINT('Ctrl Pts',(4.85884564037289,-0.251927696778831,
3.4341538212047));
#60236=CARTESIAN_POINT('Ctrl Pts',(4.88270355840431,0.0499956224363984,
3.38262661200963));
#60237=CARTESIAN_POINT('Ctrl Pts',(4.90656147643572,0.339693650112522,3.48206401309162));
#60238=CARTESIAN_POINT('Ctrl Pts',(4.93041939446714,0.546327327266884,3.70815087126575));
#60239=CARTESIAN_POINT('Ctrl Pts',(4.95427731249857,0.619369091246891,4.00560279122603));
#60240=CARTESIAN_POINT('Ctrl Pts',(4.97813523052998,0.540958241141728,4.3016846761146));
#60241=CARTESIAN_POINT('Ctrl Pts',(5.00199314856141,0.330268365670778,4.52399643996756));
#60242=CARTESIAN_POINT('Ctrl Pts',(5.02585106659282,0.0388188784636707,
4.61817680087201));
#60243=CARTESIAN_POINT('Ctrl Pts',(5.04970898462424,-0.262122881932824,
4.56119609516527));
#60244=CARTESIAN_POINT('Ctrl Pts',(5.07356690265566,-0.498968457612796,
4.36698765751594));
#60245=CARTESIAN_POINT('Ctrl Pts',(5.09742482068708,-0.613802653778546,
4.08304074106085));
#60246=CARTESIAN_POINT('Ctrl Pts',(5.12128273871849,-0.578545381446849,
3.77878810143205));
#60247=CARTESIAN_POINT('Ctrl Pts',(5.14514065674992,-0.40181800409162,3.52862779669421));
#60248=CARTESIAN_POINT('Ctrl Pts',(5.16899857478133,-0.126835179433317,
3.39373083558568));
#60249=CARTESIAN_POINT('Ctrl Pts',(5.19285649281276,0.179162301517353,3.4070831996169));
#60250=CARTESIAN_POINT('Ctrl Pts',(5.21671441084417,0.441349719463922,3.56541987207117));
#60251=CARTESIAN_POINT('Ctrl Pts',(5.24057232887559,0.595615108876583,3.83002322352904));
#60252=CARTESIAN_POINT('Ctrl Pts',(5.26443024690701,0.604236379939102,4.13619052690848));
#60253=CARTESIAN_POINT('Ctrl Pts',(5.28828816493843,0.465105397037983,4.40905553670335));
#60254=CARTESIAN_POINT('Ctrl Pts',(5.31214608296985,0.21224347534444,4.58189532532512));
#60255=CARTESIAN_POINT('Ctrl Pts',(5.33600400100126,-0.0925177574670201,
4.61244585639451));
#60256=CARTESIAN_POINT('Ctrl Pts',(5.35986191903269,-0.37465587844466,4.49323669288525));
#60257=CARTESIAN_POINT('Ctrl Pts',(5.3837198370641,-0.565180431721392,4.25341772246777));
#60258=CARTESIAN_POINT('Ctrl Pts',(5.40757775509553,-0.617502974236318,
3.95163121594683));
#60259=CARTESIAN_POINT('Ctrl Pts',(5.43143567312694,-0.518829219107294,
3.66167219466597));
#60260=CARTESIAN_POINT('Ctrl Pts',(5.45529359115837,-0.293287587282116,
3.45444353765392));
#60261=CARTESIAN_POINT('Ctrl Pts',(5.47915150918978,0.00397084862654925,
3.38061829634467));
#60262=CARTESIAN_POINT('Ctrl Pts',(5.50300942722121,0.300258303883157,3.45824875319892));
#60263=CARTESIAN_POINT('Ctrl Pts',(5.52686734525262,0.523124424966688,3.66835214690199));
#60264=CARTESIAN_POINT('Ctrl Pts',(5.55072526328404,0.618072374525773,3.95955247459688));
#60265=CARTESIAN_POINT('Ctrl Pts',(5.57458318131546,0.561884792553919,4.26064332401524));
#60266=CARTESIAN_POINT('Ctrl Pts',(5.59844109934688,0.368301073379394,4.49799978094171));
#60267=CARTESIAN_POINT('Ctrl Pts',(5.62229901737829,0.0846577094226282,
4.61358172616469));
#60268=CARTESIAN_POINT('Ctrl Pts',(5.64615693540972,-0.219686770477705,
4.57912622575047));
#60269=CARTESIAN_POINT('Ctrl Pts',(5.67001485344113,-0.470311850924231,
4.40305858798173));
#60270=CARTESIAN_POINT('Ctrl Pts',(5.69387277147256,-0.605932872639677,
4.12843214650112));
#60271=CARTESIAN_POINT('Ctrl Pts',(5.71773068950397,-0.593386801983745,
3.82240054650545));
#60272=CARTESIAN_POINT('Ctrl Pts',(5.74158860753539,-0.435741494202748,
3.55979685111874));
#60273=CARTESIAN_POINT('Ctrl Pts',(5.76544652556682,-0.171545522688555,
3.40483481554927));
#60274=CARTESIAN_POINT('Ctrl Pts',(5.78930444359822,0.134598003740687,3.39540688139736));
#60275=CARTESIAN_POINT('Ctrl Pts',(5.81316236162965,0.407828648458881,3.53381843004554));
#60276=CARTESIAN_POINT('Ctrl Pts',(5.83702027966106,0.58133408605803,3.78622407765735));
#60277=CARTESIAN_POINT('Ctrl Pts',(5.86087819769249,0.612687492198482,4.09090374899912));
#60278=CARTESIAN_POINT('Ctrl Pts',(5.8847361157239,0.494222140250734,4.3733550009975));
#60279=CARTESIAN_POINT('Ctrl Pts',(5.90859403375532,0.254905969192102,4.56451074097759));
#60280=CARTESIAN_POINT('Ctrl Pts',(5.93245195178675,-0.0467415727364197,
4.61762831145024));
#60281=CARTESIAN_POINT('Ctrl Pts',(5.95630986981815,-0.336959681931401,
4.51971877801409));
#60282=CARTESIAN_POINT('Ctrl Pts',(5.98016778784959,-0.544781677596122,
4.29472414464893));
#60283=CARTESIAN_POINT('Ctrl Pts',(6.00402570588099,-0.61939026621187,3.99766086682344));
#60284=CARTESIAN_POINT('Ctrl Pts',(6.02788362391242,-0.542540019317823,
3.70117063377655));
#60285=CARTESIAN_POINT('Ctrl Pts',(6.05174154194384,-0.333025929677459,
3.47775031355921));
#60286=CARTESIAN_POINT('Ctrl Pts',(6.07559945997526,-0.042074208138152,
3.38203805739984));
#60287=CARTESIAN_POINT('Ctrl Pts',(6.09945737800668,0.259158778028439,3.43742717299816));
#60288=CARTESIAN_POINT('Ctrl Pts',(6.12331529603809,0.497033648893269,3.63039418124561));
#60289=CARTESIAN_POINT('Ctrl Pts',(6.14717321406952,0.613345206175343,3.91371436613889));
#60290=CARTESIAN_POINT('Ctrl Pts',(6.17103113210093,0.579724447951105,4.21818191418763));
#60291=CARTESIAN_POINT('Ctrl Pts',(6.19488905013236,0.40425597056565,4.46920707734689));
#60292=CARTESIAN_POINT('Ctrl Pts',(6.21874696816377,0.13010450107023,4.60567007851858));
#60293=CARTESIAN_POINT('Ctrl Pts',(6.24260488619519,-0.176179318911185,
4.59370602015056));
#60294=CARTESIAN_POINT('Ctrl Pts',(6.26646280422661,-0.438782409775579,
4.43717629804221));
#60295=CARTESIAN_POINT('Ctrl Pts',(6.29032072225803,-0.595217424383659,
4.17259489198797));
#60296=CARTESIAN_POINT('Ctrl Pts',(6.31417864028945,-0.604035436411749,
3.86794272465182));
#60297=CARTESIAN_POINT('Ctrl Pts',(6.34598919766468,-0.423477061217623,
3.4998212904071));
#60298=CARTESIAN_POINT('Ctrl Pts',(6.3857523943837,0.100470573235224,3.30464850830547));
#60299=CARTESIAN_POINT('Ctrl Pts',(6.43346823044655,0.640013163212275,3.70919899990029));
#60300=CARTESIAN_POINT('Ctrl Pts',(6.48118406650937,0.590335835129396,4.3806576914582));
#60301=CARTESIAN_POINT('Ctrl Pts',(6.52889990257223,-0.000686065451295705,
4.70262946694599));
#60302=CARTESIAN_POINT('Ctrl Pts',(6.57661573863505,-0.591483599613884,
4.37932465573422));
#60303=CARTESIAN_POINT('Ctrl Pts',(6.6243315746979,-0.638898060441451,3.70770201230499));
#60304=CARTESIAN_POINT('Ctrl Pts',(6.67204741076074,-0.0997162142428727,
3.30448953810453));
#60305=CARTESIAN_POINT('Ctrl Pts',(6.71976324682356,0.531096731682035,3.53998115137447));
#60306=CARTESIAN_POINT('Ctrl Pts',(6.76747908288643,0.674163513320998,4.19791190586338));
#60307=CARTESIAN_POINT('Ctrl Pts',(6.81519491894923,0.19815244237474,4.67409883091767));
#60308=CARTESIAN_POINT('Ctrl Pts',(6.86291075501209,-0.459834002450772,
4.53124951681343));
#60309=CARTESIAN_POINT('Ctrl Pts',(6.91062659107492,-0.695543074258338,
3.90054607923755));
#60310=CARTESIAN_POINT('Ctrl Pts',(6.95834242713776,-0.292526745343327,
3.36117245204842));
#60311=CARTESIAN_POINT('Ctrl Pts',(7.00605826320061,0.379122722467859,3.40844412700009));
#60312=CARTESIAN_POINT('Ctrl Pts',(7.05377409926343,0.702617257610868,3.99895059076549));
#60313=CARTESIAN_POINT('Ctrl Pts',(7.10148993532628,0.380887926283931,4.59042078110798));
#60314=CARTESIAN_POINT('Ctrl Pts',(7.14920577138911,-0.290616845661789,
4.63969846327979));
#60315=CARTESIAN_POINT('Ctrl Pts',(7.19692160745196,-0.695243592084394,
4.10153121423426));
#60316=CARTESIAN_POINT('Ctrl Pts',(7.24463744351478,-0.461417505508394,
3.47012628326466));
#60317=CARTESIAN_POINT('Ctrl Pts',(7.29235327957764,0.196135405489393,3.32531254251214));
#60318=CARTESIAN_POINT('Ctrl Pts',(7.34006911564046,0.673574140181709,3.80007467379138));
#60319=CARTESIAN_POINT('Ctrl Pts',(7.38778495170331,0.532459385890787,4.45843130921146));
#60320=CARTESIAN_POINT('Ctrl Pts',(7.43550078776614,-0.0976210197556089,
4.69580341906706));
#60321=CARTESIAN_POINT('Ctrl Pts',(7.48321662382899,-0.638054538563543,
4.29420854311633));
#60322=CARTESIAN_POINT('Ctrl Pts',(7.53093245989182,-0.592552758097988,
3.62243743491725));
#60323=CARTESIAN_POINT('Ctrl Pts',(7.57864829595465,-0.00290066162856385,
3.29738783984629));
#60324=CARTESIAN_POINT('Ctrl Pts',(7.6263641320175,0.589415156704478,3.61755780248734));
#60325=CARTESIAN_POINT('Ctrl Pts',(7.67407996808033,0.64046196749915,4.28893031975233));
#60326=CARTESIAN_POINT('Ctrl Pts',(7.72179580414318,0.103362698669259,4.69497367861456));
#60327=CARTESIAN_POINT('Ctrl Pts',(7.769511640206,-0.528656126737314,4.46281201486565));
#60328=CARTESIAN_POINT('Ctrl Pts',(7.81722747626886,-0.675201896567852,
3.80564295658466));
#60329=CARTESIAN_POINT('Ctrl Pts',(7.86494331233168,-0.201699375449268,
3.32695496184095));
#60330=CARTESIAN_POINT('Ctrl Pts',(7.91265914839452,0.457026785680635,3.46633458176699));
#60331=CARTESIAN_POINT('Ctrl Pts',(7.96037498445737,0.696058217263005,4.09578736675475));
#60332=CARTESIAN_POINT('Ctrl Pts',(8.0080908205202,0.295888677698302,4.63727713897333));
#60333=CARTESIAN_POINT('Ctrl Pts',(8.05580665658303,-0.375999987428149,
4.59354550870361));
#60334=CARTESIAN_POINT('Ctrl Pts',(8.10352249264589,-0.702602078596463,
4.00475190491975));
#60335=CARTESIAN_POINT('Ctrl Pts',(8.1512383287087,-0.383993870066737,3.41159455373064));
#60336=CARTESIAN_POINT('Ctrl Pts',(8.19895416477156,0.287241817850264,3.35877897763223));
#60337=CARTESIAN_POINT('Ctrl Pts',(8.24667000083438,0.694698924651979,3.89480653282778));
#60338=CARTESIAN_POINT('Ctrl Pts',(8.29438583689724,0.464203319628796,4.52743486753713));
#60339=CARTESIAN_POINT('Ctrl Pts',(8.34210167296006,-0.192577336495663,
4.67571164775853));
#60340=CARTESIAN_POINT('Ctrl Pts',(8.3898175090229,-0.672511261332963,4.20347202468314));
#60341=CARTESIAN_POINT('Ctrl Pts',(8.43753334508575,-0.534867746972347,
3.54438091052171));
#60342=CARTESIAN_POINT('Ctrl Pts',(8.48524918114857,0.0939530494311211,
3.303691816829));
#60343=CARTESIAN_POINT('Ctrl Pts',(8.53296501721143,0.636495314888509,3.70243324182078));
#60344=CARTESIAN_POINT('Ctrl Pts',(8.58068085327425,0.594534138944492,4.37443479950165));
#60345=CARTESIAN_POINT('Ctrl Pts',(8.6283966893371,0.00660311512414562,
4.7025871193802));
#60346=CARTESIAN_POINT('Ctrl Pts',(8.67611252539993,-0.58739165091669,4.3855428768395));
#60347=CARTESIAN_POINT('Ctrl Pts',(8.72382836146277,-0.64197562573843,3.71444867815739));
#60348=CARTESIAN_POINT('Ctrl Pts',(8.77154419752561,-0.107023505379864,
3.30558065209521));
#60349=CARTESIAN_POINT('Ctrl Pts',(8.81926003358845,0.526209946737336,3.53440859822909));
#60350=CARTESIAN_POINT('Ctrl Pts',(8.86697586965128,0.676216707984864,4.19079629265377));
#60351=CARTESIAN_POINT('Ctrl Pts',(8.91469170571413,0.20524326135842,4.67197281575615));
#60352=CARTESIAN_POINT('Ctrl Pts',(8.96240754177695,-0.45420823024697,4.53606636251889));
#60353=CARTESIAN_POINT('Ctrl Pts',(9.0101233778398,-0.69655331512461,3.90788192013928));
#60354=CARTESIAN_POINT('Ctrl Pts',(9.05783921390263,-0.299242772872918,
3.36429092791464));
#60355=CARTESIAN_POINT('Ctrl Pts',(9.10555504996548,0.37286701214988,3.40448135822736));
#60356=CARTESIAN_POINT('Ctrl Pts',(9.15327088602831,0.702567282619003,3.99154572051203));
#60357=CARTESIAN_POINT('Ctrl Pts',(9.20098672209116,0.387089207071907,4.58637377773631));
#60358=CARTESIAN_POINT('Ctrl Pts',(9.24870255815397,-0.28385884346236,4.64272577234503));
#60359=CARTESIAN_POINT('Ctrl Pts',(9.29641839421684,-0.694134950315416,
4.10885280060212));
#60360=CARTESIAN_POINT('Ctrl Pts',(9.34413423027966,-0.46697625165475,3.47501862715065));
#60361=CARTESIAN_POINT('Ctrl Pts',(9.39185006634251,0.189013924253689,3.32328292626348));
#60362=CARTESIAN_POINT('Ctrl Pts',(9.43956590240535,0.671429705166911,3.79298692681914));
#60363=CARTESIAN_POINT('Ctrl Pts',(9.48728173846818,0.537261256551386,4.45279421778236));
#60364=CARTESIAN_POINT('Ctrl Pts',(9.53499757453101,-0.090282470782305,
4.69679361142145));
#60365=CARTESIAN_POINT('Ctrl Pts',(9.58271341059386,-0.634918416022234,
4.30091671014441));
#60366=CARTESIAN_POINT('Ctrl Pts',(9.63042924665669,-0.596499010353368,
3.62870336374299));
#60367=CARTESIAN_POINT('Ctrl Pts',(9.67814508271953,-0.0103053851599677,
3.29745743154951));
#60368=CARTESIAN_POINT('Ctrl Pts',(9.72586091878236,0.585351833794561,3.61136714997101));
#60369=CARTESIAN_POINT('Ctrl Pts',(9.77357675484522,0.643471456979869,4.28216439445919));
#60370=CARTESIAN_POINT('Ctrl Pts',(9.82129259090803,0.110681340139534,4.69384573385819));
#60371=CARTESIAN_POINT('Ctrl Pts',(9.8690084269709,-0.523749154402255,4.46835785966634));
#60372=CARTESIAN_POINT('Ctrl Pts',(9.91672426303372,-0.677212741539845,
3.81276975633088));
#60373=CARTESIAN_POINT('Ctrl Pts',(9.96444009909655,-0.208781447863971,
3.32911806666439));
#60374=CARTESIAN_POINT('Ctrl Pts',(10.0121559351594,0.451377061900895,3.4615475792254));
#60375=CARTESIAN_POINT('Ctrl Pts',(10.0598717712222,0.697029070393332,4.08844623493918));
#60376=CARTESIAN_POINT('Ctrl Pts',(10.1075876072851,0.302588558372737,4.63412335218805));
#60377=CARTESIAN_POINT('Ctrl Pts',(10.1553034433479,-0.369723682724971,
4.5974752378807));
#60378=CARTESIAN_POINT('Ctrl Pts',(10.2030192794108,-0.702512977046242,
4.01215641928927));
#60379=CARTESIAN_POINT('Ctrl Pts',(10.2507351154736,-0.390173794994359,
3.41567417381395));
#60380=CARTESIAN_POINT('Ctrl Pts',(10.2984509515364,0.280467986596366,3.3557873255338));
#60381=CARTESIAN_POINT('Ctrl Pts',(10.3461667875993,0.693551700540965,3.8874908887021));
#60382=CARTESIAN_POINT('Ctrl Pts',(10.3938826236621,0.469736216214169,4.52251329995044));
#60383=CARTESIAN_POINT('Ctrl Pts',(10.441598459725,-0.185445263282835,4.67770370795377));
#60384=CARTESIAN_POINT('Ctrl Pts',(10.4893142957878,-0.670329504065059,
4.21054837313121));
#60385=CARTESIAN_POINT('Ctrl Pts',(10.5370301318506,-0.539639846919137,
3.55004322755915));
#60386=CARTESIAN_POINT('Ctrl Pts',(10.5847459679134,0.0866093850789692,
3.30274030959437));
#60387=CARTESIAN_POINT('Ctrl Pts',(10.6324618039763,0.633323886102378,3.69574169404847));
#60388=CARTESIAN_POINT('Ctrl Pts',(10.6801776400391,0.598447317577389,4.36814816247366));
#60389=CARTESIAN_POINT('Ctrl Pts',(10.727893476102,0.0140073690254923,4.70247850861168));
#60390=CARTESIAN_POINT('Ctrl Pts',(10.7756093121648,-0.583295762033595,
4.39171203127037));
#60391=CARTESIAN_POINT('Ctrl Pts',(10.8233251482277,-0.644949419658282,
3.72123036834915));
#60392=CARTESIAN_POINT('Ctrl Pts',(10.8710409842905,-0.114336101388361,
3.30674714759503));
#60393=CARTESIAN_POINT('Ctrl Pts',(10.9187568203533,0.521273818073547,3.52888868827067));
#60394=CARTESIAN_POINT('Ctrl Pts',(10.9664726564162,0.678189969569843,4.18365899548663));
#60395=CARTESIAN_POINT('Ctrl Pts',(11.014188492479,0.212313836716152,4.66977242119035));
#60396=CARTESIAN_POINT('Ctrl Pts',(11.0619043285418,-0.44853335926228,4.54082352674158));
#60397=CARTESIAN_POINT('Ctrl Pts',(11.1096201646047,-0.697485469857315,
3.91522806604643));
#60398=CARTESIAN_POINT('Ctrl Pts',(11.1573360006675,-0.305925941288932,
3.36747997668469));
#60399=CARTESIAN_POINT('Ctrl Pts',(11.2050518367303,0.36657008644075,3.40058475730499));
#60400=CARTESIAN_POINT('Ctrl Pts',(11.2527676727932,0.702439163386103,3.98414177848112));
#60401=CARTESIAN_POINT('Ctrl Pts',(11.300483508856,0.393247548178179,4.58226164848818));
#60402=CARTESIAN_POINT('Ctrl Pts',(11.3481993449189,-0.277069341413063,
4.64568168744144));
#60403=CARTESIAN_POINT('Ctrl Pts',(11.3959151809817,-0.692949191524882,
4.11616229772746));
#60404=CARTESIAN_POINT('Ctrl Pts',(11.4436310170446,-0.47248313666557,3.47996928262364));
#60405=CARTESIAN_POINT('Ctrl Pts',(11.4913468531074,0.181871452681271,3.32132847698764));
#60406=CARTESIAN_POINT('Ctrl Pts',(11.5390626891702,0.669210688578896,3.78592217363756));
#60407=CARTESIAN_POINT('Ctrl Pts',(11.586778525233,0.54200345202451,4.44710683224685));
#60408=CARTESIAN_POINT('Ctrl Pts',(11.6344943612959,-0.082933894319074,
4.69770640718098));
#60409=CARTESIAN_POINT('Ctrl Pts',(11.6822101973587,-0.631711769407458,
4.30759145280778));
#60410=CARTESIAN_POINT('Ctrl Pts',(11.7299260334216,-0.600379006513997,
3.63501053441836));
#60411=CARTESIAN_POINT('Ctrl Pts',(11.7776418694844,-0.0177089639202829,
3.29760505835735));
#60412=CARTESIAN_POINT('Ctrl Pts',(11.8253577055473,0.581223492728864,3.60521966494218));
#60413=CARTESIAN_POINT('Ctrl Pts',(11.8730735416101,0.646409472732109,4.27536712768685));
#60414=CARTESIAN_POINT('Ctrl Pts',(11.9207893776729,0.11798768763725,4.69264072000881));
#60415=CARTESIAN_POINT('Ctrl Pts',(11.9685052137358,-0.518784006488825,
4.4738516814993));
#60416=CARTESIAN_POINT('Ctrl Pts',(12.0162210497986,-0.679148364938221,
3.81991735272367));
#60417=CARTESIAN_POINT('Ctrl Pts',(12.0639368858614,-0.215840329824027,
3.33135568986959));
#60418=CARTESIAN_POINT('Ctrl Pts',(12.1116527219243,0.445677201297934,3.45682038542343));
#60419=CARTESIAN_POINT('Ctrl Pts',(12.1593685579871,0.697922500842799,4.08109527893561));
#60420=CARTESIAN_POINT('Ctrl Pts',(12.2070843940499,0.309254828945687,4.63089912998995));
#60421=CARTESIAN_POINT('Ctrl Pts',(12.2548002301128,-0.36340631086944,4.60133860234362));
#60422=CARTESIAN_POINT('Ctrl Pts',(12.3025160661756,-0.702345843688318,
4.0195595833814));
#60423=CARTESIAN_POINT('Ctrl Pts',(12.3502319022385,-0.396310381268302,
3.41981869803717));
#60424=CARTESIAN_POINT('Ctrl Pts',(12.3979477383013,0.273663002289436,3.35286722952223));
#60425=CARTESIAN_POINT('Ctrl Pts',(12.4456635743641,0.69232743999824,3.88018774155459));
#60426=CARTESIAN_POINT('Ctrl Pts',(12.493379410427,0.475216936729713,4.51753369406595));
#60427=CARTESIAN_POINT('Ctrl Pts',(12.5410952464898,-0.178292591690169,
4.67962049203707));
#60428=CARTESIAN_POINT('Ctrl Pts',(12.5888110825527,-0.66807328977682,4.21760133486514));
#60429=CARTESIAN_POINT('Ctrl Pts',(12.6365269186155,-0.544352006232531,
3.55575552365962));
#60430=CARTESIAN_POINT('Ctrl Pts',(12.6842427546784,0.0792561005673328,
3.3018662506574));
#60431=CARTESIAN_POINT('Ctrl Pts',(12.7319585907411,0.630082110704352,3.68908394184497));
#60432=CARTESIAN_POINT('Ctrl Pts',(12.779674426804,0.60229402352211,4.36182063329482));
#60433=CARTESIAN_POINT('Ctrl Pts',(12.8273902628668,0.0214100670547408,
4.70229186986395));
#60434=CARTESIAN_POINT('Ctrl Pts',(12.8751060989297,-0.579135083425219,
4.39783767618763));
#60435=CARTESIAN_POINT('Ctrl Pts',(12.9228219349925,-0.647851575657132,
3.7280430229487));
#60436=CARTESIAN_POINT('Ctrl Pts',(12.9705377710554,-0.121635997485283,
3.30799064633195));
#60437=CARTESIAN_POINT('Ctrl Pts',(13.0182536071182,0.516279788787698,3.52342110712114));
#60438=CARTESIAN_POINT('Ctrl Pts',(13.065969443181,0.68008790103128,4.17650129834983));
#60439=CARTESIAN_POINT('Ctrl Pts',(13.1136852792439,0.219360829260397,4.66749763148232));
#60440=CARTESIAN_POINT('Ctrl Pts',(13.1614011153067,-0.44280866732052,4.54552061885334));
#60441=CARTESIAN_POINT('Ctrl Pts',(13.2091169513696,-0.698340151213866,
3.92258362801769));
#60442=CARTESIAN_POINT('Ctrl Pts',(13.2568327874324,-0.31257512890311,3.37073928277739));
#60443=CARTESIAN_POINT('Ctrl Pts',(13.3045486234952,0.36023244386594,3.39675473658331));
#60444=CARTESIAN_POINT('Ctrl Pts',(13.3522644595581,0.702233020544282,3.97673959790624));
#60445=CARTESIAN_POINT('Ctrl Pts',(13.3999802956209,0.39936220921291,4.57808484437918));
#60446=CARTESIAN_POINT('Ctrl Pts',(13.4476961316837,-0.270249063816132,
4.64856588328003));
#60447=CARTESIAN_POINT('Ctrl Pts',(13.4954119677466,-0.691686463226468,
4.123458892096));
#60448=CARTESIAN_POINT('Ctrl Pts',(13.5431278038094,-0.47793754049168,3.48497770064095));
#60449=CARTESIAN_POINT('Ctrl Pts',(13.5908436398723,0.174708779690948,3.31944941132403));
#60450=CARTESIAN_POINT('Ctrl Pts',(13.6385594759351,0.666917339243262,3.77888119920505));
#60451=CARTESIAN_POINT('Ctrl Pts',(13.6862753119979,0.54668544432619,4.44136978420615));
#60452=CARTESIAN_POINT('Ctrl Pts',(13.7339911480608,-0.075576105952426,
4.69854170502367));
#60453=CARTESIAN_POINT('Ctrl Pts',(13.7817069841236,-0.62843495524706,4.31423202967224));
#60454=CARTESIAN_POINT('Ctrl Pts',(13.8294228201864,-0.604192315423611,
3.64135824639153));
#60455=CARTESIAN_POINT('Ctrl Pts',(13.8771386562493,-0.025110575652917,
3.29783070386218));
#60456=CARTESIAN_POINT('Ctrl Pts',(13.9248544923121,0.577030592115723,3.59911603023956));
#60457=CARTESIAN_POINT('Ctrl Pts',(13.972570328375,0.649275688387581,4.26853927444071));
#60458=CARTESIAN_POINT('Ctrl Pts',(14.0202861644378,0.125280929622514,4.69135877091509));
#60459=CARTESIAN_POINT('Ctrl Pts',(14.0680020005006,-0.513761234509794,
4.47929287013608));
#60460=CARTESIAN_POINT('Ctrl Pts',(14.1157178365635,-0.681008551759042,
3.82708495184235));
#60461=CARTESIAN_POINT('Ctrl Pts',(14.1634336726263,-0.222875237264486,
3.33366758291179));
#60462=CARTESIAN_POINT('Ctrl Pts',(14.2111495086891,0.439927836986373,3.45215352543546));
#60463=CARTESIAN_POINT('Ctrl Pts',(14.258865344752,0.698738409372782,4.07373531525328));
#60464=CARTESIAN_POINT('Ctrl Pts',(14.3065811808148,0.315886748959774,4.62760483051036));
#60465=CARTESIAN_POINT('Ctrl Pts',(14.3542970168777,-0.357048573565392,
4.60513517296818));
#60466=CARTESIAN_POINT('Ctrl Pts',(14.4020128529405,-0.702100697086982,
4.02696057488784));
#60467=CARTESIAN_POINT('Ctrl Pts',(14.4497286890033,-0.402402947265751,
3.42402766604624));
#60468=CARTESIAN_POINT('Ctrl Pts',(14.4974445250662,0.266827620794843,3.35001901394789));
#60469=CARTESIAN_POINT('Ctrl Pts',(14.545160361129,0.691026279008849,3.87289790258421));
#60470=CARTESIAN_POINT('Ctrl Pts',(14.5928761971919,0.480644872403009,4.51249660299459));
#60471=CARTESIAN_POINT('Ctrl Pts',(14.6405920332547,-0.171120116202498,
4.6814617871012));
#60472=CARTESIAN_POINT('Ctrl Pts',(14.6883078693176,-0.665742869077823,
4.22463012647536));
#60473=CARTESIAN_POINT('Ctrl Pts',(14.7360237053803,-0.549003701508229,
3.56151716432844));
#60474=CARTESIAN_POINT('Ctrl Pts',(14.7837395414432,0.0718940126641393,
3.30106973710437));
#60475=CARTESIAN_POINT('Ctrl Pts',(14.831455377506,0.626770348775451,3.68246072472179));
#60476=CARTESIAN_POINT('Ctrl Pts',(14.8791712135689,0.606073829504824,4.35545291479698));
#60477=CARTESIAN_POINT('Ctrl Pts',(14.9268870496317,0.0288103869553486,
4.70202722386799));
#60478=CARTESIAN_POINT('Ctrl Pts',(14.9746028856946,-0.574910077240004,
4.4039191311837));
#60479=CARTESIAN_POINT('Ctrl Pts',(15.0223187217574,-0.650681771377263,
3.73488588523872));
#60480=CARTESIAN_POINT('Ctrl Pts',(15.0700345578202,-0.128922382832804,
3.30931101018402));
#60481=CARTESIAN_POINT('Ctrl Pts',(15.1177503938831,0.511228413592865,3.51800646209349));
#60482=CARTESIAN_POINT('Ctrl Pts',(15.1654662299459,0.681910291555949,4.16932399628639));
#60483=CARTESIAN_POINT('Ctrl Pts',(15.2131820660088,0.226383456244684,4.6651486993049));
#60484=CARTESIAN_POINT('Ctrl Pts',(15.2608979020716,-0.437034790293287,
4.55015711712348));
#60485=CARTESIAN_POINT('Ctrl Pts',(15.3086137381344,-0.699117264260319,
3.92994778903219));
#60486=CARTESIAN_POINT('Ctrl Pts',(15.3563295741972,-0.319189597155267,
3.37406848416447));
#60487=CARTESIAN_POINT('Ctrl Pts',(15.4040454102601,0.353854788380711,3.39299172148285));
#60488=CARTESIAN_POINT('Ctrl Pts',(15.4517612463229,0.70194887699091,3.96934000098645));
#60489=CARTESIAN_POINT('Ctrl Pts',(15.4994770823858,0.40543251098856,4.57384382934891));
#60490=CARTESIAN_POINT('Ctrl Pts',(15.5471929184486,-0.263398768235635,
4.65137803949801));
#60491=CARTESIAN_POINT('Ctrl Pts',(15.5949087545115,-0.690346905678043,
4.13074177323664));
#60492=CARTESIAN_POINT('Ctrl Pts',(15.6426245905743,-0.483338857283784,
3.4900433248913));
#60493=CARTESIAN_POINT('Ctrl Pts',(15.6903404266371,0.167526700878456,3.31764593799033));
#60494=CARTESIAN_POINT('Ctrl Pts',(15.7380562627,0.664549911894371,3.77186478559966));
#60495=CARTESIAN_POINT('Ctrl Pts',(15.7857720987628,0.551306713402943,4.43558371090429));
#60496=CARTESIAN_POINT('Ctrl Pts',(15.8334879348256,-0.0682099229505586,
4.69929941216862));
#60497=CARTESIAN_POINT('Ctrl Pts',(15.8812037708885,-0.625088337514006,
4.32083770313399));
#60498=CARTESIAN_POINT('Ctrl Pts',(15.9289196069513,-0.607938513517956,
3.64774579458877));
#60499=CARTESIAN_POINT('Ctrl Pts',(15.9766354430142,-0.0325093982219456,
3.29813434300035));
#60500=CARTESIAN_POINT('Ctrl Pts',(16.024351279077,0.572773597682653,3.59305692382598));
#60501=CARTESIAN_POINT('Ctrl Pts',(16.0720671151399,0.652069785580651,4.2616815931263));
#60502=CARTESIAN_POINT('Ctrl Pts',(16.1197829512026,0.132560255996602,4.69000002896988));
#60503=CARTESIAN_POINT('Ctrl Pts',(16.1674987872655,-0.508681396370837,
4.48468082119526));
#60504=CARTESIAN_POINT('Ctrl Pts',(16.2152146233283,-0.682793095381579,
3.83427175754402));
#60505=CARTESIAN_POINT('Ctrl Pts',(16.2629304593912,-0.229885388781225,
3.33605348899688));
#60506=CARTESIAN_POINT('Ctrl Pts',(16.310646295454,0.434129607578297,3.44754751763412));
#60507=CARTESIAN_POINT('Ctrl Pts',(16.3583621315168,0.699476705356048,4.06636716140204));
#60508=CARTESIAN_POINT('Ctrl Pts',(16.4060779675797,0.322483581772784,4.62424081966442));
#60509=CARTESIAN_POINT('Ctrl Pts',(16.4537938036425,-0.350651177000141,
4.60886452804932));
#60510=CARTESIAN_POINT('Ctrl Pts',(16.5015096397054,-0.701777564471952,
4.03435857174156));
#60511=CARTESIAN_POINT('Ctrl Pts',(16.5492254757682,-0.408450816253369,
3.42830061032894));
#60512=CARTESIAN_POINT('Ctrl Pts',(16.596941311831,0.259962601354342,3.34724299517707));
#60513=CARTESIAN_POINT('Ctrl Pts',(16.6446571478939,0.689648362099571,3.86562218151166));
#60514=CARTESIAN_POINT('Ctrl Pts',(16.6923729839567,0.486019420324727,4.50740258623259));
#60515=CARTESIAN_POINT('Ctrl Pts',(16.7400888200196,-0.163928633504336,
4.6832273886238));
#60516=CARTESIAN_POINT('Ctrl Pts',(16.7878046560824,-0.663338500820136,
4.23163396723712));
#60517=CARTESIAN_POINT('Ctrl Pts',(16.8355204921452,-0.553594416058007,
3.56732750958986));
#60518=CARTESIAN_POINT('Ctrl Pts',(16.8832363282081,0.064523939115192,3.30035085740826));
#60519=CARTESIAN_POINT('Ctrl Pts',(16.9309521642709,0.623388968170475,3.67587277835446));
#60520=CARTESIAN_POINT('Ctrl Pts',(16.9786680003338,0.609786315682611,4.34904571427615));
#60521=CARTESIAN_POINT('Ctrl Pts',(17.0263838363966,0.0362075067348799,
4.70168460001938));
#60522=CARTESIAN_POINT('Ctrl Pts',(17.0740996724594,-0.570621212771584,
4.40995572075944));
#60523=CARTESIAN_POINT('Ctrl Pts',(17.1218155085223,-0.653439692453966,
3.74175819514654));
#60524=CARTESIAN_POINT('Ctrl Pts',(17.1695313445851,-0.136194448093839,
3.31070809249149));
#60525=CARTESIAN_POINT('Ctrl Pts',(17.2172471806479,0.50612025357182,3.51264535462077));
#60526=CARTESIAN_POINT('Ctrl Pts',(17.2649630167108,0.683656938721366,4.16212788651693));
#60527=CARTESIAN_POINT('Ctrl Pts',(17.3126788527736,0.233380937628925,4.66272588556639));
#60528=CARTESIAN_POINT('Ctrl Pts',(17.3603946888365,-0.431212369515449,
4.55473250655174));
#60529=CARTESIAN_POINT('Ctrl Pts',(17.4081105248993,-0.699816722678643,
3.93731973111387));
#60530=CARTESIAN_POINT('Ctrl Pts',(17.4558263609621,-0.325768611341644,
3.37746721105403));
#60531=CARTESIAN_POINT('Ctrl Pts',(17.503542197025,0.347437828384778,3.38929612998149));
#60532=CARTESIAN_POINT('Ctrl Pts',(17.5512580330878,0.701586764287296,3.96194380963385));
#60533=CARTESIAN_POINT('Ctrl Pts',(17.5989738691507,0.411457779244836,4.56953907446917));
#60534=CARTESIAN_POINT('Ctrl Pts',(17.6466897052135,-0.256519215569882,
4.65411784373439));
#60535=CARTESIAN_POINT('Ctrl Pts',(17.6944055412764,-0.688930667671302,
4.13801013220155));
#60536=CARTESIAN_POINT('Ctrl Pts',(17.7421213773391,-0.488686487089258,
3.49516559270919));
#60537=CARTESIAN_POINT('Ctrl Pts',(17.789837213402,0.160326013994967,3.3159182573078));
#60538=CARTESIAN_POINT('Ctrl Pts',(17.8375530494648,0.662108669494809,3.76487371217125));
#60539=CARTESIAN_POINT('Ctrl Pts',(17.8852688855277,0.555866745946156,4.42974925503083));
#60540=CARTESIAN_POINT('Ctrl Pts',(17.9329847215905,-0.060836163514142,
4.69997944445332));
#60541=CARTESIAN_POINT('Ctrl Pts',(17.9807005576534,-0.621672287934692,
4.32740773946617));
#60542=CARTESIAN_POINT('Ctrl Pts',(18.0284163937162,-0.611617184687133,
3.65417246951162));
#60543=CARTESIAN_POINT('Ctrl Pts',(18.0761322297791,-0.0399046098013318,
3.29851594204507));
#60544=CARTESIAN_POINT('Ctrl Pts',(18.1238480658419,0.568452982276385,3.58704301871817));
#60545=CARTESIAN_POINT('Ctrl Pts',(18.1715639019047,0.65479145395626,4.25479484546229));
#60546=CARTESIAN_POINT('Ctrl Pts',(18.2192797379675,0.139824858206545,4.68856464509573));
#60547=CARTESIAN_POINT('Ctrl Pts',(18.2669955740304,-0.503545056316242,
4.49001493620888));
#60548=CARTESIAN_POINT('Ctrl Pts',(18.3147114100932,-0.684501797587214,
3.84147697155243));
#60549=CARTESIAN_POINT('Ctrl Pts',(18.3624272461561,-0.236870005719869,
3.33851314310973));
#60550=CARTESIAN_POINT('Ctrl Pts',(18.4101430822189,0.42828315711354,3.44300287363294));
#60551=CARTESIAN_POINT('Ctrl Pts',(18.4578589182817,0.70013730678616,4.05899163580144));
#60552=CARTESIAN_POINT('Ctrl Pts',(18.5055747543446,0.32904459463985,4.62080747111051));
#60553=CARTESIAN_POINT('Ctrl Pts',(18.5532905904074,-0.34421483176614,4.61252625334797));
#60554=CARTESIAN_POINT('Ctrl Pts',(18.6010064264702,-0.701376481735239,
4.0417527522082));
#60555=CARTESIAN_POINT('Ctrl Pts',(18.6487222625331,-0.414453316462639,
3.43263705626685));
#60556=CARTESIAN_POINT('Ctrl Pts',(18.6964380985959,0.253068706501803,3.34453948155689));
#60557=CARTESIAN_POINT('Ctrl Pts',(18.7441539346588,0.68819384232267,3.85836138648927));
#60558=CARTESIAN_POINT('Ctrl Pts',(18.7918697707216,0.491339983515996,4.50225220959958));
#60559=CARTESIAN_POINT('Ctrl Pts',(18.8395856067844,-0.156718942392259,
4.68491710048942));
#60560=CARTESIAN_POINT('Ctrl Pts',(18.8873014428473,-0.660860452068119,
4.23861207919858));
#60561=CARTESIAN_POINT('Ctrl Pts',(18.9350172789101,-0.558123639969822,
3.57318591405529));
#60562=CARTESIAN_POINT('Ctrl Pts',(18.9827331149729,0.0571466985584877,
3.29970969142451));
#60563=CARTESIAN_POINT('Ctrl Pts',(19.0304489510358,0.619938344467307,3.66932083449001));
#60564=CARTESIAN_POINT('Ctrl Pts',(19.0781647870986,0.613431069708698,4.3425997434341));
#60565=CARTESIAN_POINT('Ctrl Pts',(19.1258806231615,0.0436006047213211,
4.70126403633668));
#60566=CARTESIAN_POINT('Ctrl Pts',(19.1735964592243,-0.566268966340429,
4.41594677447179));
#60567=CARTESIAN_POINT('Ctrl Pts',(19.2213122952871,-0.656125032675529,
3.74865918919138));
#60568=CARTESIAN_POINT('Ctrl Pts',(19.26902813135,-0.143451385285705,3.31218173833215));
#60569=CARTESIAN_POINT('Ctrl Pts',(19.3167439674128,0.500955875668841,3.50733837970023));
#60570=CARTESIAN_POINT('Ctrl Pts',(19.3644598034757,0.68532764936022,4.15491376927485));
#60571=CARTESIAN_POINT('Ctrl Pts',(19.4121756395385,0.240352494576274,4.66022945763735));
#60572=CARTESIAN_POINT('Ctrl Pts',(19.4598914756013,-0.425342048711971,
4.55924628221868));
#60573=CARTESIAN_POINT('Ctrl Pts',(19.5076073116642,-0.700438454444525,
3.94469862920436));
#60574=CARTESIAN_POINT('Ctrl Pts',(19.555323147727,-0.332311429993836,3.3809350976725));
#60575=CARTESIAN_POINT('Ctrl Pts',(19.6030389837899,0.340982256434611,3.38566835039883));
#60576=CARTESIAN_POINT('Ctrl Pts',(19.6507548198527,0.701146760813864,3.95455188724214));
#60577=CARTESIAN_POINT('Ctrl Pts',(19.6984706559155,0.417437272672218,4.56517097885182));
#60578=CARTESIAN_POINT('Ctrl Pts',(19.7461864919784,-0.249611033919464,
4.6567851409082));
#60579=CARTESIAN_POINT('Ctrl Pts',(19.7939023280412,-0.687438163400574,
4.14526287985386));
#60580=CARTESIAN_POINT('Ctrl Pts',(19.841618164104,-0.493979350866992,3.5003444672369));
#60581=CARTESIAN_POINT('Ctrl Pts',(19.8893340001669,0.153106602982307,3.31426555646693));
#60582=CARTESIAN_POINT('Ctrl Pts',(19.9370498362297,0.659595612567133,3.75791065255607));
#60583=CARTESIAN_POINT('Ctrl Pts',(19.9847656722925,0.560361770063263,4.42386348253578));
#60584=CARTESIAN_POINT('Ctrl Pts',(20.0324815083554,-0.0534494809679074,
4.70058849011268));
#60585=CARTESIAN_POINT('Ctrl Pts',(20.0801973444182,-0.618198828117398,
4.33392863744107));
#60586=CARTESIAN_POINT('Ctrl Pts',(20.1279131804811,-0.615205937201001,
3.66066167313574));
#60587=CARTESIAN_POINT('Ctrl Pts',(20.1756290165439,-0.0473369003220797,
3.29892991724937));
#60588=CARTESIAN_POINT('Ctrl Pts',(20.2233448526068,0.564147630203746,3.58116102158214));
#60589=CARTESIAN_POINT('Ctrl Pts',(20.2710606886696,0.657292163719816,4.24771695100806));
#60590=CARTESIAN_POINT('Ctrl Pts',(20.3187765247324,0.147355317357748,4.68736342730055));
#60591=CARTESIAN_POINT('Ctrl Pts',(20.3664923607953,-0.498896366832293,
4.49468216892218));
#60592=CARTESIAN_POINT('Ctrl Pts',(20.4062555575143,-0.653992183610565,
3.9575054511282));
#60593=CARTESIAN_POINT('Ctrl Pts',(20.4380661148895,-0.465699721472375,
3.59327933193152));
#60594=CARTESIAN_POINT('Ctrl Pts',(20.461924032921,-0.215665100260693,3.41899970433759));
#60595=CARTESIAN_POINT('Ctrl Pts',(20.4857819509523,0.0900520562992202,
3.38718375849312));
#60596=CARTESIAN_POINT('Ctrl Pts',(20.5096398689838,0.372154449079436,3.50499792242313));
#60597=CARTESIAN_POINT('Ctrl Pts',(20.5334977870152,0.564103623124681,3.74397162737493));
#60598=CARTESIAN_POINT('Ctrl Pts',(20.5573557050466,0.61766411855396,4.04548854604559));
#60599=CARTESIAN_POINT('Ctrl Pts',(20.581213623078,0.520427284318709,4.33591550271974));
#60600=CARTESIAN_POINT('Ctrl Pts',(20.6050715411094,0.295805552416038,4.5441843692251));
#60601=CARTESIAN_POINT('Ctrl Pts',(20.6289294591409,-0.00108183093298003,
4.61939465531364));
#60602=CARTESIAN_POINT('Ctrl Pts',(20.6527873771723,-0.297740088546312,
4.543141139652));
#60603=CARTESIAN_POINT('Ctrl Pts',(20.6766452952037,-0.521574030203058,
4.33407743490148));
#60604=CARTESIAN_POINT('Ctrl Pts',(20.7005032132351,-0.617878846294169,
4.04332131262121));
#60605=CARTESIAN_POINT('Ctrl Pts',(20.7243611312665,-0.563090193646282,
3.74197268265107));
#60606=CARTESIAN_POINT('Ctrl Pts',(20.748219049298,-0.370613436173077,3.50371837193987));
#60607=CARTESIAN_POINT('Ctrl Pts',(20.7720769673294,-0.0875101228827464,
3.38681864340431));
#60608=CARTESIAN_POINT('Ctrl Pts',(20.7959348853608,0.216991017820888,3.41985835035499));
#60609=CARTESIAN_POINT('Ctrl Pts',(20.8197928033922,0.468432357761717,3.59475855107288));
#60610=CARTESIAN_POINT('Ctrl Pts',(20.8436507214236,0.605329007232586,3.86875129405724));
#60611=CARTESIAN_POINT('Ctrl Pts',(20.8675086394551,0.594206341669864,4.17483793696784));
#60612=CARTESIAN_POINT('Ctrl Pts',(20.8913665574864,0.437783978244149,4.43817193323088));
#60613=CARTESIAN_POINT('Ctrl Pts',(20.9152244755179,0.174311539695801,4.5943609607934));
#60614=CARTESIAN_POINT('Ctrl Pts',(20.9390823935493,-0.13178483570001,4.60521254097096));
#60615=CARTESIAN_POINT('Ctrl Pts',(20.9629403115808,-0.405656219889506,
4.46807317049539));
#60616=CARTESIAN_POINT('Ctrl Pts',(20.9867982296121,-0.580333613298163,
4.21647715910241));
#60617=CARTESIAN_POINT('Ctrl Pts',(21.0106561476436,-0.613103627724174,
3.91194658594648));
#60618=CARTESIAN_POINT('Ctrl Pts',(21.034514065675,-0.495953105920446,3.62894747086441));
#60619=CARTESIAN_POINT('Ctrl Pts',(21.0583719837064,-0.257528539509485,
3.43668080652407));
#60620=CARTESIAN_POINT('Ctrl Pts',(21.0822299017379,0.0438687693677006,
3.38216102944232));
#60621=CARTESIAN_POINT('Ctrl Pts',(21.1060878197692,0.334538969374667,3.47871971028568));
#60622=CARTESIAN_POINT('Ctrl Pts',(21.1299457378007,0.543405278604256,3.7027456213393));
#60623=CARTESIAN_POINT('Ctrl Pts',(21.153803655832,0.619394195209021,3.99945832503004));
#60624=CARTESIAN_POINT('Ctrl Pts',(21.1776615738635,0.543924359096133,4.29630348300169));
#60625=CARTESIAN_POINT('Ctrl Pts',(21.2015194918949,0.33545020099803,4.52069436823682));
#60626=CARTESIAN_POINT('Ctrl Pts',(21.2253774099264,0.0449493312674926,
4.61776129700707));
#60627=CARTESIAN_POINT('Ctrl Pts',(21.2492353279577,-0.256542874348706,
4.56376876117982));
#60628=CARTESIAN_POINT('Ctrl Pts',(21.2730932459892,-0.495303359101402,
4.37191940649105));
#60629=CARTESIAN_POINT('Ctrl Pts',(21.2969511640206,-0.612948680759938,
4.08912562603418));
#60630=CARTESIAN_POINT('Ctrl Pts',(21.320809082052,-0.580711353586496,3.78453820227854));
#60631=CARTESIAN_POINT('Ctrl Pts',(21.3446670000834,-0.406474282201139,
3.53263705712739));
#60632=CARTESIAN_POINT('Ctrl Pts',(21.3685249181149,-0.132843176680646,
3.39501888221951));
#60633=CARTESIAN_POINT('Ctrl Pts',(21.3923828361463,0.17327170411384,3.40533506996376));
#60634=CARTESIAN_POINT('Ctrl Pts',(21.4162407541777,0.437016933425986,3.56106303144932));
#60635=CARTESIAN_POINT('Ctrl Pts',(21.4400986722091,0.593899618413251,3.82412303814848));
#60636=CARTESIAN_POINT('Ctrl Pts',(21.4639565902405,0.605557669197671,4.13018975281259));
#60637=CARTESIAN_POINT('Ctrl Pts',(21.4878145082719,0.469140374803543,4.40442152661638));
#60638=CARTESIAN_POINT('Ctrl Pts',(21.5116724263034,0.218005479642704,4.57976122094124));
#60639=CARTESIAN_POINT('Ctrl Pts',(21.5355303443348,-0.0864376936408111,
4.61333350436739));
#60640=CARTESIAN_POINT('Ctrl Pts',(21.5593882623662,-0.369744496313637,
4.49692903910649));
#60641=CARTESIAN_POINT('Ctrl Pts',(21.5832461803976,-0.562638697999917,
4.2590118877088));
#60642=CARTESIAN_POINT('Ctrl Pts',(21.607104098429,-0.617952412054802,3.95775927442416));
#60643=CARTESIAN_POINT('Ctrl Pts',(21.6309620164605,-0.522159928676552,
3.66683566915707));
#60644=CARTESIAN_POINT('Ctrl Pts',(21.6548199344919,-0.298685119385998,
3.45737981799522));
#60645=CARTESIAN_POINT('Ctrl Pts',(21.6786778525233,-0.00217366238626178,
3.38060938201055));
#60646=CARTESIAN_POINT('Ctrl Pts',(21.7025357705547,0.294869314276287,3.45529682398599));
#60647=CARTESIAN_POINT('Ctrl Pts',(21.7263936885862,0.519808711519421,3.66317902991346));
#60648=CARTESIAN_POINT('Ctrl Pts',(21.7502516066175,0.617640719491047,3.95342313784609));
#60649=CARTESIAN_POINT('Ctrl Pts',(21.774109524649,0.564442747351711,4.25505655730362));
#60650=CARTESIAN_POINT('Ctrl Pts',(21.7979674426804,0.373223148373148,4.49432170089927));
#60651=CARTESIAN_POINT('Ctrl Pts',(21.8218253607118,0.0907403232229101,
4.61271172357229));
#60652=CARTESIAN_POINT('Ctrl Pts',(21.8456832787432,-0.213930982672105,
4.58127703989962));
#60653=CARTESIAN_POINT('Ctrl Pts',(21.8695411967746,-0.466290335940828,
4.40770428630285));
#60654=CARTESIAN_POINT('Ctrl Pts',(21.8933991148061,-0.604629000578284,
4.13443672906324));
#60655=CARTESIAN_POINT('Ctrl Pts',(21.9172570328375,-0.595119404811066,
3.82829572958469));
#60656=CARTESIAN_POINT('Ctrl Pts',(21.9411149508689,-0.440086903840403,
3.56414110135311));
#60657=CARTESIAN_POINT('Ctrl Pts',(21.9649728689003,-0.177441167154219,
3.40656584639871));
#60658=CARTESIAN_POINT('Ctrl Pts',(21.9888307869318,0.128593768301574,3.39410140682164));
#60659=CARTESIAN_POINT('Ctrl Pts',(22.0126887049631,0.403184024583593,3.52979567762293));
#60660=CARTESIAN_POINT('Ctrl Pts',(22.0365466229946,0.579184804342829,3.7804677133541));
#60661=CARTESIAN_POINT('Ctrl Pts',(22.060404541026,0.613559122762511,4.08482137310942));
#60662=CARTESIAN_POINT('Ctrl Pts',(22.0842624590574,0.497901522652627,4.36843389665204));
#60663=CARTESIAN_POINT('Ctrl Pts',(22.1081203770888,0.260493437687466,4.56195429652472));
#60664=CARTESIAN_POINT('Ctrl Pts',(22.1319782951203,-0.0406123884881684,
4.61806156357065));
#60665=CARTESIAN_POINT('Ctrl Pts',(22.1558362131517,-0.33178737942464,4.52303594266224));
#60666=CARTESIAN_POINT('Ctrl Pts',(22.1796941311831,-0.541831318374727,
4.30011378656432));
#60667=CARTESIAN_POINT('Ctrl Pts',(22.2035520492145,-0.619382740812877,
4.00380563470766));
#60668=CARTESIAN_POINT('Ctrl Pts',(22.2274099672459,-0.545478211438426,
3.70656690151735));
#60669=CARTESIAN_POINT('Ctrl Pts',(22.2512678852774,-0.338189400908512,
3.48108055383335));
#60670=CARTESIAN_POINT('Ctrl Pts',(22.2751258033088,-0.0482040696311437,
3.38248414587532));
#60671=CARTESIAN_POINT('Ctrl Pts',(22.2989837213402,0.253568469476171,3.43488718493857));
#60672=CARTESIAN_POINT('Ctrl Pts',(22.3228416393716,0.493336611197201,3.62547570084914));
#60673=CARTESIAN_POINT('Ctrl Pts',(22.346699557403,0.612470512379129,3.90764560936005));
#60674=CARTESIAN_POINT('Ctrl Pts',(22.3705574754344,0.581838691587799,4.21239868278141));
#60675=CARTESIAN_POINT('Ctrl Pts',(22.3944153934659,0.408931458591185,4.46521449128699));
#60676=CARTESIAN_POINT('Ctrl Pts',(22.4182733114973,0.13602935083686,4.60427268703701));
#60677=CARTESIAN_POINT('Ctrl Pts',(22.4421312295287,-0.170135649772668,
4.59556974592947));
#60678=CARTESIAN_POINT('Ctrl Pts',(22.4659891475601,-0.434697828443077,
4.44123378804823));
#60679=CARTESIAN_POINT('Ctrl Pts',(22.4898470655916,-0.592964587096883,
4.17900413283907));
#60680=CARTESIAN_POINT('Ctrl Pts',(22.513704983623,-0.606235276705168,3.87300312362118));
#60681=CARTESIAN_POINT('Ctrl Pts',(22.5375629016543,-0.471265070143009,
3.59805624874041));
#60682=CARTESIAN_POINT('Ctrl Pts',(22.5614208196858,-0.22105744785653,3.4213956854475));
#60683=CARTESIAN_POINT('Ctrl Pts',(22.5852787377172,0.0832042338527798,
3.38621941950615));
#60684=CARTESIAN_POINT('Ctrl Pts',(22.6091366557487,0.36712117327337,3.50112963696785));
#60685=CARTESIAN_POINT('Ctrl Pts',(22.63299457378,0.561265174232679,3.7380264683998));
#60686=CARTESIAN_POINT('Ctrl Pts',(22.6568524918115,0.618167971965146,4.03898443479498));
#60687=CARTESIAN_POINT('Ctrl Pts',(22.6807104098429,0.523905402647805,4.33040686810369));
#60688=CARTESIAN_POINT('Ctrl Pts',(22.7045683278744,0.301545895245711,4.54104106792393));
#60689=CARTESIAN_POINT('Ctrl Pts',(22.7284262459057,0.00542710047790416,
4.61936606261506));
#60690=CARTESIAN_POINT('Ctrl Pts',(22.7522841639372,-0.291974666000346,
4.54625809930836));
#60691=CARTESIAN_POINT('Ctrl Pts',(22.7761420819686,-0.518067845615496,
4.33953802216683));
#60692=CARTESIAN_POINT('Ctrl Pts',(22.7920473606562,-0.584213376873476,
4.14642833911731));
#60693=CARTESIAN_POINT('Ctrl Pts',(22.8,-0.592174260192535,4.04779597854866));
#60694=CARTESIAN_POINT('Ctrl Pts',(3.96816317011931,-0.282716247115855,
3.54616445487434));
#60695=CARTESIAN_POINT('Ctrl Pts',(3.97611580946312,-0.207125539895404,
3.49907532469992));
#60696=CARTESIAN_POINT('Ctrl Pts',(3.99202108815073,-0.0320395462633344,
3.44344227840288));
#60697=CARTESIAN_POINT('Ctrl Pts',(4.01587900618214,0.238586678544665,3.49618207793602));
#60698=CARTESIAN_POINT('Ctrl Pts',(4.03973692421357,0.450798406251909,3.67207593825259));
#60699=CARTESIAN_POINT('Ctrl Pts',(4.06359484224498,0.552814952159096,3.92817792166325));
#60700=CARTESIAN_POINT('Ctrl Pts',(4.0874527602764,0.519633627921064,4.20183097195279));
#60701=CARTESIAN_POINT('Ctrl Pts',(4.11131067830782,0.359398059257131,4.42613686623617));
#60702=CARTESIAN_POINT('Ctrl Pts',(4.13516859633924,0.11127440638865,4.54623750576341));
#60703=CARTESIAN_POINT('Ctrl Pts',(4.15902651437066,-0.164055973910312,
4.53276988152218));
#60704=CARTESIAN_POINT('Ctrl Pts',(4.18288443240208,-0.399271733473279,
4.38902461621758));
#60705=CARTESIAN_POINT('Ctrl Pts',(4.2067423504335,-0.536853866020863,4.15015270818839));
#60706=CARTESIAN_POINT('Ctrl Pts',(4.23060026846491,-0.543161034884179,
3.87456412255522));
#60707=CARTESIAN_POINT('Ctrl Pts',(4.25445818649634,-0.416650307492554,
3.62964815836115));
#60708=CARTESIAN_POINT('Ctrl Pts',(4.27831610452775,-0.188257351244862,
3.47529323740438));
#60709=CARTESIAN_POINT('Ctrl Pts',(4.30217402255918,0.0861697193074588,
3.44924344981891));
#60710=CARTESIAN_POINT('Ctrl Pts',(4.32603194059059,0.339525912432458,3.55786862136322));
#60711=CARTESIAN_POINT('Ctrl Pts',(4.34988985862202,0.509858789389686,3.77460696883261));
#60712=CARTESIAN_POINT('Ctrl Pts',(4.37374777665342,0.555517294574929,4.0464600464808));
#60713=CARTESIAN_POINT('Ctrl Pts',(4.39760569468486,0.465336694276122,4.30695238014399));
#60714=CARTESIAN_POINT('Ctrl Pts',(4.42146361271626,0.261368594047533,4.4923864940975));
#60715=CARTESIAN_POINT('Ctrl Pts',(4.4453215307477,-0.00651124555331369,
4.55741869872598));
#60716=CARTESIAN_POINT('Ctrl Pts',(4.4691794487791,-0.272798909000308,4.48614684730087));
#60717=CARTESIAN_POINT('Ctrl Pts',(4.49303736681053,-0.472379807908186,
4.29599884956661));
#60718=CARTESIAN_POINT('Ctrl Pts',(4.51689528484195,-0.55645097662433,4.03347107014466));
#60719=CARTESIAN_POINT('Ctrl Pts',(4.54075320287336,-0.504454724024634,
3.76275870240323));
#60720=CARTESIAN_POINT('Ctrl Pts',(4.56461112090479,-0.329105550388866,
3.55005829421323));
#60721=CARTESIAN_POINT('Ctrl Pts',(4.5884690389362,-0.0732811049967102,
3.44738088927219));
#60722=CARTESIAN_POINT('Ctrl Pts',(4.61232695696762,0.200462566687888,3.47983390993684));
#60723=CARTESIAN_POINT('Ctrl Pts',(4.63618487499904,0.425187680335341,3.63948170866684));
#60724=CARTESIAN_POINT('Ctrl Pts',(4.66004279303046,0.54594282425631,3.88728604994618));
#60725=CARTESIAN_POINT('Ctrl Pts',(4.68390071106188,0.533200076465109,4.16265202228146));
#60726=CARTESIAN_POINT('Ctrl Pts',(4.7077586290933,0.390075385898422,4.39824514461603));
#60727=CARTESIAN_POINT('Ctrl Pts',(4.73161654712472,0.151566638040082,4.53645648111246));
#60728=CARTESIAN_POINT('Ctrl Pts',(4.75547446515614,-0.124004281411749,
4.54348959519552));
#60729=CARTESIAN_POINT('Ctrl Pts',(4.77933238318755,-0.369252776249408,
4.41762469889406));
#60730=CARTESIAN_POINT('Ctrl Pts',(4.80319030121898,-0.524208909050512,
4.18963918784455));
#60731=CARTESIAN_POINT('Ctrl Pts',(4.82704821925039,-0.550981684424725,
3.91528172969931));
#60732=CARTESIAN_POINT('Ctrl Pts',(4.85090613728181,-0.443024429517375,
3.66164019632193));
#60733=CARTESIAN_POINT('Ctrl Pts',(4.87476405531323,-0.226735633849849,
3.49073685167984));
#60734=CARTESIAN_POINT('Ctrl Pts',(4.89862197334465,0.0449962004486201,
3.44436221885167));
#60735=CARTESIAN_POINT('Ctrl Pts',(4.92247989137607,0.305725238065515,3.53385615878353));
#60736=CARTESIAN_POINT('Ctrl Pts',(4.94633780940749,0.491696127187109,3.73733496539613));
#60737=CARTESIAN_POINT('Ctrl Pts',(4.9701957274389,0.557433919677865,4.00504252782125));
#60738=CARTESIAN_POINT('Ctrl Pts',(4.99405364547033,0.486863934612277,4.27151705483839));
#60739=CARTESIAN_POINT('Ctrl Pts',(5.01791156350174,0.297242455626679,4.47159826597145));
#60740=CARTESIAN_POINT('Ctrl Pts',(5.04176948153317,0.0349370995184326,
4.55636085499566));
#60741=CARTESIAN_POINT('Ctrl Pts',(5.06562739956458,-0.235911329089554,
4.505078060008));
#60742=CARTESIAN_POINT('Ctrl Pts',(5.08948531759601,-0.449073011639563,
4.33028992129829));
#60743=CARTESIAN_POINT('Ctrl Pts',(5.11334323562741,-0.552424110340463,
4.07473689991432));
#60744=CARTESIAN_POINT('Ctrl Pts',(5.13720115365885,-0.520692466332485,
3.80090867070902));
#60745=CARTESIAN_POINT('Ctrl Pts',(5.16105907169026,-0.361637330928202,
3.57576369465428));
#60746=CARTESIAN_POINT('Ctrl Pts',(5.18491698972168,-0.114152017308863,
3.45435605122152));
#60747=CARTESIAN_POINT('Ctrl Pts',(5.2087749077531,0.161246573981014,3.46637321630784));
#60748=CARTESIAN_POINT('Ctrl Pts',(5.23263282578452,0.397215985664045,3.60887666570863));
#60749=CARTESIAN_POINT('Ctrl Pts',(5.25649074381594,0.536055268906009,3.84702042432939));
#60750=CARTESIAN_POINT('Ctrl Pts',(5.28034866184735,0.543814437048104,4.12257185628156));
#60751=CARTESIAN_POINT('Ctrl Pts',(5.30420657987878,0.418596162124088,4.3681511305826));
#60752=CARTESIAN_POINT('Ctrl Pts',(5.32806449791019,0.191019723230217,4.5237074252207));
#60753=CARTESIAN_POINT('Ctrl Pts',(5.35192241594161,-0.0832662412662402,
4.55120298888854));
#60754=CARTESIAN_POINT('Ctrl Pts',(5.37578033397303,-0.337191341646214,
4.44391440730515));
#60755=CARTESIAN_POINT('Ctrl Pts',(5.39963825200445,-0.508663974085987,
4.22807666114996));
#60756=CARTESIAN_POINT('Ctrl Pts',(5.42349617003587,-0.555754409133215,
3.95646795866016));
#60757=CARTESIAN_POINT('Ctrl Pts',(5.4473540880673,-0.466947752701331,3.69550402606682));
#60758=CARTESIAN_POINT('Ctrl Pts',(5.47121200609871,-0.263959651332346,
3.50899765340418));
#60759=CARTESIAN_POINT('Ctrl Pts',(5.49506992413013,0.00357377490351851,
3.44255472911916));
#60760=CARTESIAN_POINT('Ctrl Pts',(5.51892784216155,0.270233315828591,3.51242235806964));
#60761=CARTESIAN_POINT('Ctrl Pts',(5.54278576019296,0.470813450024345,3.70151600181885));
#60762=CARTESIAN_POINT('Ctrl Pts',(5.56664367822439,0.556266870991092,3.96359711366712));
#60763=CARTESIAN_POINT('Ctrl Pts',(5.5905015962558,0.505697889589837,4.23457972281303));
#60764=CARTESIAN_POINT('Ctrl Pts',(5.61435951428722,0.331471999260015,4.4482011999181));
#60765=CARTESIAN_POINT('Ctrl Pts',(5.63821743231864,0.0761921759760934,
4.55222527486821));
#60766=CARTESIAN_POINT('Ctrl Pts',(5.66207535035006,-0.197718709731212,
4.52121522783523));
#60767=CARTESIAN_POINT('Ctrl Pts',(5.68593326838148,-0.423281985227643,
4.3627538599096));
#60768=CARTESIAN_POINT('Ctrl Pts',(5.70979118641289,-0.545341285237878,
4.11558929214995));
#60769=CARTESIAN_POINT('Ctrl Pts',(5.73364910444432,-0.534049786451273,
3.84015999362387));
#60770=CARTESIAN_POINT('Ctrl Pts',(5.75750702247573,-0.392168567195948,
3.6038159310769));
#60771=CARTESIAN_POINT('Ctrl Pts',(5.78136494050716,-0.154391451667357,
3.46434966433946));
#60772=CARTESIAN_POINT('Ctrl Pts',(5.80522285853857,0.121138580962943,3.45586449715393));
#60773=CARTESIAN_POINT('Ctrl Pts',(5.82908077656999,0.367046927720705,3.58043527923202));
#60774=CARTESIAN_POINT('Ctrl Pts',(5.85293869460141,0.523202308305842,3.80760107017232));
#60775=CARTESIAN_POINT('Ctrl Pts',(5.87679661263283,0.551420461789987,4.08181362911724));
#60776=CARTESIAN_POINT('Ctrl Pts',(5.90065453066425,0.44480131269862,4.33602054829434));
#60777=CARTESIAN_POINT('Ctrl Pts',(5.92451244869567,0.229416087376931,4.50806125053784));
#60778=CARTESIAN_POINT('Ctrl Pts',(5.94837036672709,-0.042067546589846,
4.55586721297736));
#60779=CARTESIAN_POINT('Ctrl Pts',(5.97222828475851,-0.30326465903273,4.46774835821298));
#60780=CARTESIAN_POINT('Ctrl Pts',(5.99608620278993,-0.490305038147314,
4.26525255699254));
#60781=CARTESIAN_POINT('Ctrl Pts',(6.01994412082133,-0.557452977205748,
3.99789477357902));
#60782=CARTESIAN_POINT('Ctrl Pts',(6.04380203885278,-0.488287539408226,
3.73105273207384));
#60783=CARTESIAN_POINT('Ctrl Pts',(6.06765995688417,-0.299724270968661,
3.52997381710292));
#60784=CARTESIAN_POINT('Ctrl Pts',(6.09151787491561,-0.0378669053578504,
3.44383251805177));
#60785=CARTESIAN_POINT('Ctrl Pts',(6.11537579294702,0.233243627260218,3.49368287747685));
#60786=CARTESIAN_POINT('Ctrl Pts',(6.13923371097844,0.447331678364145,3.6673537262422));
#60787=CARTESIAN_POINT('Ctrl Pts',(6.16309162900986,0.552012406214274,3.92234268746235));
#60788=CARTESIAN_POINT('Ctrl Pts',(6.18694954704127,0.521753629494025,4.19636433484848));
#60789=CARTESIAN_POINT('Ctrl Pts',(6.2108074650727,0.363831507594212,4.42228768590875));
#60790=CARTESIAN_POINT('Ctrl Pts',(6.23466538310411,0.117094415953721,4.54510476979165));
#60791=CARTESIAN_POINT('Ctrl Pts',(6.25852330113554,-0.158561881267111,
4.53433708369694));
#60792=CARTESIAN_POINT('Ctrl Pts',(6.28238121916695,-0.394905399742298,
4.39345989467659));
#60793=CARTESIAN_POINT('Ctrl Pts',(6.30623913719837,-0.535697351746728,
4.1553358869807));
#60794=CARTESIAN_POINT('Ctrl Pts',(6.33009705522979,-0.543633587309765,
3.88114808171798));
#60795=CARTESIAN_POINT('Ctrl Pts',(6.36190761260502,-0.381130543103143,
3.54983775818315));
#60796=CARTESIAN_POINT('Ctrl Pts',(6.40167080932404,0.0904237977681596,
3.37418170676098));
#60797=CARTESIAN_POINT('Ctrl Pts',(6.4493866453869,0.576013642360818,3.73827828410759));
#60798=CARTESIAN_POINT('Ctrl Pts',(6.49710248144972,0.531303907723303,4.34259299019566));
#60799=CARTESIAN_POINT('Ctrl Pts',(6.54481831751257,-0.000617460830772086,
4.63236849138271));
#60800=CARTESIAN_POINT('Ctrl Pts',(6.5925341535754,-0.532336898979176,4.34139325430452));
#60801=CARTESIAN_POINT('Ctrl Pts',(6.64024998963824,-0.575010046738857,
3.73693099107234));
#60802=CARTESIAN_POINT('Ctrl Pts',(6.68796582570108,-0.0897448725589052,
3.37403863313417));
#60803=CARTESIAN_POINT('Ctrl Pts',(6.73568166176391,0.477988548433368,3.58598174571673));
#60804=CARTESIAN_POINT('Ctrl Pts',(6.78339749782676,0.606749053262868,4.17812127049189));
#60805=CARTESIAN_POINT('Ctrl Pts',(6.83111333388958,0.178337754027021,4.60669083891839));
#60806=CARTESIAN_POINT('Ctrl Pts',(6.87882916995244,-0.413851892207341,
4.47812605548031));
#60807=CARTESIAN_POINT('Ctrl Pts',(6.92654500601527,-0.625990718083913,
3.91049119230943));
#60808=CARTESIAN_POINT('Ctrl Pts',(6.97426084207811,-0.263274891453005,
3.42505341469988));
#60809=CARTESIAN_POINT('Ctrl Pts',(7.02197667814094,0.341211513798207,3.46759805477058));
#60810=CARTESIAN_POINT('Ctrl Pts',(7.06969251420378,0.63235750294684,3.99905552874491));
#60811=CARTESIAN_POINT('Ctrl Pts',(7.11740835026662,0.342800202184808,4.53138035934227));
#60812=CARTESIAN_POINT('Ctrl Pts',(7.16512418632946,-0.261555976381552,
4.57573041153878));
#60813=CARTESIAN_POINT('Ctrl Pts',(7.2128400223923,-0.625721183287191,4.0913783776429));
#60814=CARTESIAN_POINT('Ctrl Pts',(7.26055585845514,-0.41527704940159,3.52311216844965));
#60815=CARTESIAN_POINT('Ctrl Pts',(7.30827169451797,0.176522415171576,3.39277939551711));
#60816=CARTESIAN_POINT('Ctrl Pts',(7.35598753058081,0.606218615784068,3.8200666455489));
#60817=CARTESIAN_POINT('Ctrl Pts',(7.40370336664364,0.479214941044062,4.4125894643569));
#60818=CARTESIAN_POINT('Ctrl Pts',(7.4514192027065,-0.0878591916424711,
4.62622502914213));
#60819=CARTESIAN_POINT('Ctrl Pts',(7.49913503876932,-0.574250874682306,
4.26478851416677));
#60820=CARTESIAN_POINT('Ctrl Pts',(7.54685087483217,-0.53329914461431,3.6601926322252));
#60821=CARTESIAN_POINT('Ctrl Pts',(7.594566710895,-0.00261060360317682,
3.36764708477891));
#60822=CARTESIAN_POINT('Ctrl Pts',(7.64228254695784,0.530475294557976,3.65580094934904));
#60823=CARTESIAN_POINT('Ctrl Pts',(7.68999838302067,0.576417567478113,4.26003809833172));
#60824=CARTESIAN_POINT('Ctrl Pts',(7.73771421908353,0.093026718772369,4.62547826040714));
#60825=CARTESIAN_POINT('Ctrl Pts',(7.78543005514634,-0.475791997136335,
4.41653211173522));
#60826=CARTESIAN_POINT('Ctrl Pts',(7.8331458912092,-0.607683601098078,3.82507811568403));
#60827=CARTESIAN_POINT('Ctrl Pts',(7.88086172727203,-0.181530003744534,
3.39425757752065));
#60828=CARTESIAN_POINT('Ctrl Pts',(7.92857756333487,0.411325389238953,3.51969962646458));
#60829=CARTESIAN_POINT('Ctrl Pts',(7.97629339939771,0.626454348233276,4.08620889879763));
#60830=CARTESIAN_POINT('Ctrl Pts',(8.02400923546054,0.266300640003926,4.57355121287022));
#60831=CARTESIAN_POINT('Ctrl Pts',(8.07172507152339,-0.338401043502061,
4.5341926229444));
#60832=CARTESIAN_POINT('Ctrl Pts',(8.11944090758622,-0.632343841791292,
4.00427672775865));
#60833=CARTESIAN_POINT('Ctrl Pts',(8.16715674364906,-0.345595560302635,
3.47043344766624));
#60834=CARTESIAN_POINT('Ctrl Pts',(8.2148725797119,0.258518441882999,3.42289928101069));
#60835=CARTESIAN_POINT('Ctrl Pts',(8.26258841577473,0.625230981070026,3.90532558443901));
#60836=CARTESIAN_POINT('Ctrl Pts',(8.31030425183758,0.417784289925175,4.47469286043008));
#60837=CARTESIAN_POINT('Ctrl Pts',(8.35802008790041,-0.173320143095541,
4.60814237859973));
#60838=CARTESIAN_POINT('Ctrl Pts',(8.40573592396325,-0.605262021838435,
4.18312539302794));
#60839=CARTESIAN_POINT('Ctrl Pts',(8.45345176002609,-0.481382472773795,
3.58994154129225));
#60840=CARTESIAN_POINT('Ctrl Pts',(8.50116759608892,0.0845580080604409,
3.37332068174828));
#60841=CARTESIAN_POINT('Ctrl Pts',(8.54888343215178,0.572847569000584,3.73218908285563));
#60842=CARTESIAN_POINT('Ctrl Pts',(8.59659926821459,0.535082392934658,4.33699236997728));
#60843=CARTESIAN_POINT('Ctrl Pts',(8.64431510427745,0.00594282213592907,
4.6323303784547));
#60844=CARTESIAN_POINT('Ctrl Pts',(8.69203094034027,-0.528654133672296,
4.34698967074364));
#60845=CARTESIAN_POINT('Ctrl Pts',(8.73974677640312,-0.577779864139828,
3.74300300926635));
#60846=CARTESIAN_POINT('Ctrl Pts',(8.78746261246595,-0.0963214550818077,
3.37502063878676));
#60847=CARTESIAN_POINT('Ctrl Pts',(8.8351784485288,0.473590428273928,3.58096643225285));
#60848=CARTESIAN_POINT('Ctrl Pts',(8.88289428459164,0.608596934220305,4.17171719864135));
#60849=CARTESIAN_POINT('Ctrl Pts',(8.93061012065447,0.184719511004659,4.60477741930878));
#60850=CARTESIAN_POINT('Ctrl Pts',(8.97832595671731,-0.408788681441581,
4.48246123012823));
#60851=CARTESIAN_POINT('Ctrl Pts',(9.02604179278014,-0.626899937697651,
3.91709346970068));
#60852=CARTESIAN_POINT('Ctrl Pts',(9.07375762884299,-0.269319335070538,
3.42786005172794));
#60853=CARTESIAN_POINT('Ctrl Pts',(9.12147346490582,0.335581356962483,3.46403155175812));
#60854=CARTESIAN_POINT('Ctrl Pts',(9.16918930096866,0.632312525313962,3.99239112474344));
#60855=CARTESIAN_POINT('Ctrl Pts',(9.21690513703149,0.348381372290835,4.52773804495445));
#60856=CARTESIAN_POINT('Ctrl Pts',(9.26462097309434,-0.255473755443411,
4.5784549981902));
#60857=CARTESIAN_POINT('Ctrl Pts',(9.31233680915717,-0.624723402584967,
4.09796782591368));
#60858=CARTESIAN_POINT('Ctrl Pts',(9.36005264522002,-0.420279936527615,
3.52751529167185));
#60859=CARTESIAN_POINT('Ctrl Pts',(9.40776848128285,0.170113062081096,3.39095273519949));
#60860=CARTESIAN_POINT('Ctrl Pts',(9.45548431734569,0.604288618254829,3.81368765339017));
#60861=CARTESIAN_POINT('Ctrl Pts',(9.50320015340853,0.483536638109595,4.40751606625661));
#60862=CARTESIAN_POINT('Ctrl Pts',(9.55091598947137,-0.0812544769791981,
4.62711620503893));
#60863=CARTESIAN_POINT('Ctrl Pts',(9.5986318255342,-0.571428355597161,4.27082588331087));
#60864=CARTESIAN_POINT('Ctrl Pts',(9.64634766159704,-0.536850782714826,
3.66583198574659));
#60865=CARTESIAN_POINT('Ctrl Pts',(9.69406349765987,-0.0092748755543832,
3.36770971750703));
#60866=CARTESIAN_POINT('Ctrl Pts',(9.74177933372272,0.52681829253995,3.65022934471732));
#60867=CARTESIAN_POINT('Ctrl Pts',(9.78949516978555,0.579126116453474,4.253948746587));
#60868=CARTESIAN_POINT('Ctrl Pts',(9.83721100584839,0.099613516627068,4.62446310696212));
#60869=CARTESIAN_POINT('Ctrl Pts',(9.88492684191123,-0.471375708268938,
4.42152338761395));
#60870=CARTESIAN_POINT('Ctrl Pts',(9.93264267797408,-0.609493367214024,
3.83149225544889));
#60871=CARTESIAN_POINT('Ctrl Pts',(9.9803585140369,-0.187903888785556,3.39620437793004));
#60872=CARTESIAN_POINT('Ctrl Pts',(10.0280743500997,0.406240621987656,3.51539131074786));
#60873=CARTESIAN_POINT('Ctrl Pts',(10.0757901861626,0.627328118774167,4.07960185956908));
#60874=CARTESIAN_POINT('Ctrl Pts',(10.1235060222254,0.27233055140652,4.57071279591595));
#60875=CARTESIAN_POINT('Ctrl Pts',(10.1712218582883,-0.332752351661881,
4.5377293902281));
#60876=CARTESIAN_POINT('Ctrl Pts',(10.2189376943511,-0.632263650146131,
4.01094081146358));
#60877=CARTESIAN_POINT('Ctrl Pts',(10.2666535304139,-0.351157510074434,
3.47410511718603));
#60878=CARTESIAN_POINT('Ctrl Pts',(10.3143693664768,0.252421974751429,3.42020678572945));
#60879=CARTESIAN_POINT('Ctrl Pts',(10.3620852025396,0.624198476151732,3.89874148420283));
#60880=CARTESIAN_POINT('Ctrl Pts',(10.4098010386024,0.422763912373798,4.47026343579529));
#60881=CARTESIAN_POINT('Ctrl Pts',(10.4575168746653,-0.166901257195935,
4.60993523836389));
#60882=CARTESIAN_POINT('Ctrl Pts',(10.5052327107281,-0.603298434176698,
4.18949412648294));
#60883=CARTESIAN_POINT('Ctrl Pts',(10.552948546791,-0.485677376113382,3.5950376425108));
#60884=CARTESIAN_POINT('Ctrl Pts',(10.6006643828538,0.0779486895418537,
3.3724643225678));
#60885=CARTESIAN_POINT('Ctrl Pts',(10.6483802189166,0.569993274196054,3.72616667108832));
#60886=CARTESIAN_POINT('Ctrl Pts',(10.6960960549795,0.538604264682155,4.3313343790158));
#60887=CARTESIAN_POINT('Ctrl Pts',(10.7438118910423,0.0126066714187673,
4.63223262845832));
#60888=CARTESIAN_POINT('Ctrl Pts',(10.7915277271052,-0.524967822187051,
4.35254192703816));
#60889=CARTESIAN_POINT('Ctrl Pts',(10.839243563168,-0.580456287010268,3.74910654946403));
#60890=CARTESIAN_POINT('Ctrl Pts',(10.8869593992308,-0.102902812003948,
3.37607048800905));
#60891=CARTESIAN_POINT('Ctrl Pts',(10.9346752352937,0.469147898628881,3.5759984978049));
#60892=CARTESIAN_POINT('Ctrl Pts',(10.9823910713565,0.610372875182502,4.16529361116822));
#60893=CARTESIAN_POINT('Ctrl Pts',(11.0301069074193,0.191083048662156,4.60279705802663));
#60894=CARTESIAN_POINT('Ctrl Pts',(11.0778227434822,-0.403681281635282,
4.48674269127424));
#60895=CARTESIAN_POINT('Ctrl Pts',(11.125538579545,-0.627738879572117,3.92370502162571));
#60896=CARTESIAN_POINT('Ctrl Pts',(11.1732544156079,-0.275334205393669,
3.43073020456744));
#60897=CARTESIAN_POINT('Ctrl Pts',(11.2209702516707,0.329914106159097,3.46052459999659));
#60898=CARTESIAN_POINT('Ctrl Pts',(11.2686860877335,0.632197217644931,3.98572755614488));
#60899=CARTESIAN_POINT('Ctrl Pts',(11.3164019237964,0.353923896562866,4.52403711709511));
#60900=CARTESIAN_POINT('Ctrl Pts',(11.3641177598592,-0.24936318455202,4.58111533006939));
#60901=CARTESIAN_POINT('Ctrl Pts',(11.411833595922,-0.623656216347001,4.10454639383227));
#60902=CARTESIAN_POINT('Ctrl Pts',(11.4595494319849,-0.425236148486169,
3.53197089548594));
#60903=CARTESIAN_POINT('Ctrl Pts',(11.5072652680477,0.163684817628688,3.3891937253683));
#60904=CARTESIAN_POINT('Ctrl Pts',(11.5549811041106,0.602291497100466,3.80732935570755));
#60905=CARTESIAN_POINT('Ctrl Pts',(11.6026969401734,0.487804627338989,4.40239740331947));
#60906=CARTESIAN_POINT('Ctrl Pts',(11.6504127762363,-0.0746407375468588,
4.62793772378323));
#60907=CARTESIAN_POINT('Ctrl Pts',(11.6981286122991,-0.568542364648052,
4.276833170433));
#60908=CARTESIAN_POINT('Ctrl Pts',(11.7458444483619,-0.540342790144192,
3.67150845704832));
#60909=CARTESIAN_POINT('Ctrl Pts',(11.7935602844247,-0.0159381172083995,
3.36784258204823));
#60910=CARTESIAN_POINT('Ctrl Pts',(11.8412761204876,0.523102773999324,3.64469659094542));
#60911=CARTESIAN_POINT('Ctrl Pts',(11.8889919565504,0.581770338872691,4.24783118742311));
#60912=CARTESIAN_POINT('Ctrl Pts',(11.9367077926133,0.106189249871976,4.62337859111715));
#60913=CARTESIAN_POINT('Ctrl Pts',(11.9844236286761,-0.466907061217805,
4.4264678426758));
#60914=CARTESIAN_POINT('Ctrl Pts',(12.0321394647389,-0.611235433702689,
3.83792511225401));
#60915=CARTESIAN_POINT('Ctrl Pts',(12.0798553008018,-0.19425690235234,3.39821824509208));
#60916=CARTESIAN_POINT('Ctrl Pts',(12.1275711368646,0.401110731454808,3.51113682306459));
#60917=CARTESIAN_POINT('Ctrl Pts',(12.1752869729275,0.628132208685083,4.07298597854376));
#60918=CARTESIAN_POINT('Ctrl Pts',(12.2230028089903,0.27833021362349,4.56781098689255));
#60919=CARTESIAN_POINT('Ctrl Pts',(12.2707186450531,-0.327066699269377,
4.54120642908287));
#60920=CARTESIAN_POINT('Ctrl Pts',(12.3184344811159,-0.632113229655128,
4.01760367991507));
#60921=CARTESIAN_POINT('Ctrl Pts',(12.3661503171788,-0.356680454936339,
3.47783520061383));
#60922=CARTESIAN_POINT('Ctrl Pts',(12.4138661532416,0.246297469784735,3.4175786911271));
#60923=CARTESIAN_POINT('Ctrl Pts',(12.4615819893045,0.623096638228782,3.89216863128209));
#60924=CARTESIAN_POINT('Ctrl Pts',(12.5092978253673,0.427696576213203,4.46578177652963));
#60925=CARTESIAN_POINT('Ctrl Pts',(12.5570136614302,-0.16046383269669,4.61166034941614));
#60926=CARTESIAN_POINT('Ctrl Pts',(12.604729497493,-0.601267834987779,4.1958418118296));
#60927=CARTESIAN_POINT('Ctrl Pts',(12.6524453335558,-0.489918332714758,
3.60017872502631));
#60928=CARTESIAN_POINT('Ctrl Pts',(12.7001611696187,0.0713307128527425,
3.37167766707246));
#60929=CARTESIAN_POINT('Ctrl Pts',(12.7478770056815,0.56707566724347,3.72017467542775));
#60930=CARTESIAN_POINT('Ctrl Pts',(12.7955928417444,0.542066310823814,4.32563958500381));
#60931=CARTESIAN_POINT('Ctrl Pts',(12.8433086778072,0.0192691204123526,
4.63206465306178));
#60932=CARTESIAN_POINT('Ctrl Pts',(12.89102451387,-0.521223199767296,4.35805502464836));
#60933=CARTESIAN_POINT('Ctrl Pts',(12.9387403499329,-0.583068235550835,
3.7552379577156));
#60934=CARTESIAN_POINT('Ctrl Pts',(12.9864561859957,-0.109472738970043,
3.37718964036075));
#60935=CARTESIAN_POINT('Ctrl Pts',(13.0341720220585,0.464653258261548,3.57107765943178));
#60936=CARTESIAN_POINT('Ctrl Pts',(13.0818878581214,0.612081018822183,4.15885166366515));
#60937=CARTESIAN_POINT('Ctrl Pts',(13.1296036941842,0.197425361721354,4.6007497409078));
#60938=CARTESIAN_POINT('Ctrl Pts',(13.177319530247,-0.398529042827853,4.49097008735187));
#60939=CARTESIAN_POINT('Ctrl Pts',(13.2250353663099,-0.628508095190705,
3.93032504803489));
#60940=CARTESIAN_POINT('Ctrl Pts',(13.2727512023727,-0.281318492899819,
3.4336635891944));
#60941=CARTESIAN_POINT('Ctrl Pts',(13.3204670384356,0.324210210062374,3.45707757060249));
#60942=CARTESIAN_POINT('Ctrl Pts',(13.3681828744984,0.632011688508986,3.97906557286167));
#60943=CARTESIAN_POINT('Ctrl Pts',(13.4158987105612,0.359427108647973,4.52027798167956));
#60944=CARTESIAN_POINT('Ctrl Pts',(13.4636145466241,-0.243224915581421,
4.58371111441534));
#60945=CARTESIAN_POINT('Ctrl Pts',(13.5113303826869,-0.622519757336015,
4.11111334923356));
#60946=CARTESIAN_POINT('Ctrl Pts',(13.5590462187498,-0.430145127231255,
3.53647848575196));
#60947=CARTESIAN_POINT('Ctrl Pts',(13.6067620548126,0.157238391843492,3.38750256099959));
#60948=CARTESIAN_POINT('Ctrl Pts',(13.6544778908755,0.600227476264717,3.8009924589658));
#60949=CARTESIAN_POINT('Ctrl Pts',(13.7021937269383,0.492018433545193,4.39723404398833));
#60950=CARTESIAN_POINT('Ctrl Pts',(13.7499095630011,-0.0680187073756014,
4.62868949418496));
#60951=CARTESIAN_POINT('Ctrl Pts',(13.797625399064,-0.565593222711038,4.28280970824024));
#60952=CARTESIAN_POINT('Ctrl Pts',(13.8453412351268,-0.543774778860562,
3.67722141563181));
#60953=CARTESIAN_POINT('Ctrl Pts',(13.8930570711896,-0.0225995885319848,
3.36804566363559));
#60954=CARTESIAN_POINT('Ctrl Pts',(13.9407729072525,0.519329151684885,3.63920330259016));
#60955=CARTESIAN_POINT('Ctrl Pts',(13.9884887433153,0.584349941003394,4.24168610034696));
#60956=CARTESIAN_POINT('Ctrl Pts',(14.0362045793781,0.112753188118911,4.62222483333648));
#60957=CARTESIAN_POINT('Ctrl Pts',(14.083920415441,-0.462386552345973,4.43136492771341));
#60958=CARTESIAN_POINT('Ctrl Pts',(14.1316362515038,-0.612909607059929,
3.84437597156854));
#60959=CARTESIAN_POINT('Ctrl Pts',(14.1793520875667,-0.200588338784227,
3.40029895531576));
#60960=CARTESIAN_POINT('Ctrl Pts',(14.2270679236295,0.395936287445344,3.50693663598317));
#60961=CARTESIAN_POINT('Ctrl Pts',(14.2747837596923,0.628866528650988,4.06636199058228));
#60962=CARTESIAN_POINT('Ctrl Pts',(14.3224995957552,0.284298960241116,4.5648461081192));
#60963=CARTESIAN_POINT('Ctrl Pts',(14.370215431818,-0.321344717859966,4.54462335329573));
#60964=CARTESIAN_POINT('Ctrl Pts',(14.4179312678809,-0.631892597026201,
4.02426459303334));
#60965=CARTESIAN_POINT('Ctrl Pts',(14.4656471039437,-0.362163781425906,
3.48162328362967));
#60966=CARTESIAN_POINT('Ctrl Pts',(14.5133629400065,0.240145607263868,3.41501528911991));
#60967=CARTESIAN_POINT('Ctrl Pts',(14.5610787760693,0.6219255896881,3.8856077557581));
#60968=CARTESIAN_POINT('Ctrl Pts',(14.6087946121322,0.432581733546503,4.46124838043455));
#60969=CARTESIAN_POINT('Ctrl Pts',(14.656510448195,-0.154008584636381,4.61331752013935));
#60970=CARTESIAN_POINT('Ctrl Pts',(14.7042262842579,-0.599170449821005,
4.20216774399712));
#60971=CARTESIAN_POINT('Ctrl Pts',(14.7519421203207,-0.494104871512583,
3.60536421779174));
#60972=CARTESIAN_POINT('Ctrl Pts',(14.7996579563836,0.0647048130865326,
3.37096080264023));
#60973=CARTESIAN_POINT('Ctrl Pts',(14.8473737924464,0.564095072216763,3.71421376143635));
#60974=CARTESIAN_POINT('Ctrl Pts',(14.8950896285093,0.545468146811986,4.319908620492));
#60975=CARTESIAN_POINT('Ctrl Pts',(14.942805464572,0.0259294290834894,4.63182647092298));
#60976=CARTESIAN_POINT('Ctrl Pts',(14.9905213006349,-0.517420682347921,
4.36352835120552));
#60977=CARTESIAN_POINT('Ctrl Pts',(15.0382371366977,-0.585615419638682,
3.76139655297334));
#60978=CARTESIAN_POINT('Ctrl Pts',(15.0859529727606,-0.116030506223773,
3.3783779715317));
#60979=CARTESIAN_POINT('Ctrl Pts',(15.1336688088234,0.460107006415252,3.56620446371685));
#60980=CARTESIAN_POINT('Ctrl Pts',(15.1813846448862,0.613721175406852,4.15239207167311));
#60981=CARTESIAN_POINT('Ctrl Pts',(15.2291004809491,0.203745745708236,4.59863569535852));
#60982=CARTESIAN_POINT('Ctrl Pts',(15.2768163170119,-0.393332537305518,
4.49514294880206));
#60983=CARTESIAN_POINT('Ctrl Pts',(15.3245321530748,-0.629207499112597,
3.93695281360709));
#60984=CARTESIAN_POINT('Ctrl Pts',(15.3722479891376,-0.287271532882751,
3.43665987978239));
#60985=CARTESIAN_POINT('Ctrl Pts',(15.4199638252004,0.318470302234025,3.45369084645546));
#60986=CARTESIAN_POINT('Ctrl Pts',(15.4676796612633,0.631755958513824,3.97240591487529));
#60987=CARTESIAN_POINT('Ctrl Pts',(15.5153954973261,0.364890397275464,4.51646105625472));
#60988=CARTESIAN_POINT('Ctrl Pts',(15.563111333389,-0.237059630341402,4.58624206290064));
#60989=CARTESIAN_POINT('Ctrl Pts',(15.6108271694518,-0.621314151784485,
4.11766796269128));
#60990=CARTESIAN_POINT('Ctrl Pts',(15.6585430055147,-0.435006327496808,
3.54103756178819));
#60991=CARTESIAN_POINT('Ctrl Pts',(15.7062588415774,0.150774500763906,3.38587942993986));
#60992=CARTESIAN_POINT('Ctrl Pts',(15.7539746776403,0.598096785009218,3.79467766703735));
#60993=CARTESIAN_POINT('Ctrl Pts',(15.8016905137032,0.496177588678611,4.39202656178461));
#60994=CARTESIAN_POINT('Ctrl Pts',(15.849406349766,-0.0613891220090978,
4.62937143274106));
#60995=CARTESIAN_POINT('Ctrl Pts',(15.8971221858288,-0.562581257362808,
4.28875483288714));
#60996=CARTESIAN_POINT('Ctrl Pts',(15.9448380218917,-0.547146367654922,
3.68297022692873));
#60997=CARTESIAN_POINT('Ctrl Pts',(15.9925538579545,-0.0292585496004989,
3.36831893971177));
#60998=CARTESIAN_POINT('Ctrl Pts',(16.0402696940173,0.515497844752703,3.63375008981994));
#60999=CARTESIAN_POINT('Ctrl Pts',(16.0879855300802,0.586864636315616,4.23551416792571));
#61000=CARTESIAN_POINT('Ctrl Pts',(16.135701366143,0.119304602276749,4.62100196177401));
#61001=CARTESIAN_POINT('Ctrl Pts',(16.1834172022059,-0.457814683770117,
4.43621409878185));
#61002=CARTESIAN_POINT('Ctrl Pts',(16.2311330382687,-0.614515701326505,
3.85084411686165));
#61003=CARTESIAN_POINT('Ctrl Pts',(16.2788488743316,-0.206897494815317,
3.40244627748567));
#61004=CARTESIAN_POINT('Ctrl Pts',(16.3265647103943,0.390717864711932,3.50279121604045));
#61005=CARTESIAN_POINT('Ctrl Pts',(16.3742805464572,0.629530997107116,4.05973063144581));
#61006=CARTESIAN_POINT('Ctrl Pts',(16.42199638252,0.290236128279341,4.56181848892059));
#61007=CARTESIAN_POINT('Ctrl Pts',(16.4697122185829,-0.315587043004215,
4.54797978333095));
#61008=CARTESIAN_POINT('Ctrl Pts',(16.5174280546457,-0.631601776766168,
4.03092281095576));
#61009=CARTESIAN_POINT('Ctrl Pts',(16.5651438907086,-0.367606880481235,
3.48546894547127));
#61010=CARTESIAN_POINT('Ctrl Pts',(16.6128597267714,0.233967070508539,3.41251686443844));
#61011=CARTESIAN_POINT('Ctrl Pts',(16.6605755628343,0.620685460604191,3.87905958638177));
#61012=CARTESIAN_POINT('Ctrl Pts',(16.7082913988971,0.437418841753611,4.45666375105816));
#61013=CARTESIAN_POINT('Ctrl Pts',(16.7560072349599,-0.147536230033309,
4.61490656646286));
#61014=CARTESIAN_POINT('Ctrl Pts',(16.8037230710227,-0.597006511643959,
4.20847122033102));
#61015=CARTESIAN_POINT('Ctrl Pts',(16.8514389070856,-0.498236527486006,
3.61059354482716));
#61016=CARTESIAN_POINT('Ctrl Pts',(16.8991547431484,0.058071726216741,3.37031380889701));
#61017=CARTESIAN_POINT('Ctrl Pts',(16.9468705792113,0.561051820186282,3.70828459122417));
#61018=CARTESIAN_POINT('Ctrl Pts',(16.9945864152741,0.548809394786867,4.31414212204871));
#61019=CARTESIAN_POINT('Ctrl Pts',(17.0423022513369,0.0325868576366809,
4.63151810849805));
#61020=CARTESIAN_POINT('Ctrl Pts',(17.0900180873998,-0.513560692294518,
4.3689612987585));
#61021=CARTESIAN_POINT('Ctrl Pts',(17.1377339234626,-0.588097556344686,
3.76758165116972));
#61022=CARTESIAN_POINT('Ctrl Pts',(17.1854497595255,-0.122575385359494,
3.37963534952775));
#61023=CARTESIAN_POINT('Ctrl Pts',(17.2331655955883,0.455509648066065,3.56137945195155));
#61024=CARTESIAN_POINT('Ctrl Pts',(17.2808814316511,0.615293162755707,4.14591555269289));
#61025=CARTESIAN_POINT('Ctrl Pts',(17.328597267714,0.210043498584534,4.59645515619697));
#61026=CARTESIAN_POINT('Ctrl Pts',(17.3763131037768,-0.388092342271454,
4.49926081212312));
#61027=CARTESIAN_POINT('Ctrl Pts',(17.4240289398397,-0.629837013651323,
3.94358758216158));
#61028=CARTESIAN_POINT('Ctrl Pts',(17.4717447759025,-0.293192664107019,
3.43971874351766));
#61029=CARTESIAN_POINT('Ctrl Pts',(17.5194606119653,0.312695020235776,3.45036480373676));
#61030=CARTESIAN_POINT('Ctrl Pts',(17.5671764480282,0.631430056064715,3.96574932190893));
#61031=CARTESIAN_POINT('Ctrl Pts',(17.614892284091,0.370313155609181,4.51258676478657));
#61032=CARTESIAN_POINT('Ctrl Pts',(17.6626081201539,-0.230868013642575,
4.58870789439952));
#61033=CARTESIAN_POINT('Ctrl Pts',(17.7103239562166,-0.620039533605355,
4.12420950615009));
#61034=CARTESIAN_POINT('Ctrl Pts',(17.7580397922796,-0.43981920932378,3.54564761719411));
#61035=CARTESIAN_POINT('Ctrl Pts',(17.8057556283423,0.144293862368219,3.38432451247882));
#61036=CARTESIAN_POINT('Ctrl Pts',(17.8534714644052,0.595899660001039,3.78838568133928));
#61037=CARTESIAN_POINT('Ctrl Pts',(17.901187300468,0.500281630760053,4.38677553513073));
#61038=CARTESIAN_POINT('Ctrl Pts',(17.9489031365309,-0.0547527178302441,
4.62998346370502));
#61039=CARTESIAN_POINT('Ctrl Pts',(17.9966189725937,-0.559506803158163,
4.29466788401745));
#61040=CARTESIAN_POINT('Ctrl Pts',(18.0443348086565,-0.550457182027191,
3.68875425238845));
#61041=CARTESIAN_POINT('Ctrl Pts',(18.0920506447194,-0.0359142607682062,
3.36866237992255));
#61042=CARTESIAN_POINT('Ctrl Pts',(18.1397664807822,0.511609278766163,3.62833755835171));
#61043=CARTESIAN_POINT('Ctrl Pts',(18.187482316845,0.589314145488933,4.22931607570827));
#61044=CARTESIAN_POINT('Ctrl Pts',(18.2351981529079,0.12584276464555,4.61971011226051));
#61045=CARTESIAN_POINT('Ctrl Pts',(18.2829139889707,-0.453191963311679,
4.44101481725822));
#61046=CARTESIAN_POINT('Ctrl Pts',(18.3306298250336,-0.616053538105107,
3.85732882968247));
#61047=CARTESIAN_POINT('Ctrl Pts',(18.3783456610964,-0.213183669654489,
3.40465997308746));
#61048=CARTESIAN_POINT('Ctrl Pts',(18.4260614971592,0.385456042892229,3.49870102369));
#61049=CARTESIAN_POINT('Ctrl Pts',(18.4737773332221,0.630125540247444,4.05309263771424));
#61050=CARTESIAN_POINT('Ctrl Pts',(18.5214931692849,0.296141058265729,4.55872846559028));
#61051=CARTESIAN_POINT('Ctrl Pts',(18.5692090053478,-0.309794314237323,
4.55127534637221));
#61052=CARTESIAN_POINT('Ctrl Pts',(18.6169248414106,-0.631240801177943,
4.0375775941191));
#61053=CARTESIAN_POINT('Ctrl Pts',(18.6646406774734,-0.373009147508776,
3.4893717589807));
#61054=CARTESIAN_POINT('Ctrl Pts',(18.7123565135363,0.227762545801372,3.41008369459593));
#61055=CARTESIAN_POINT('Ctrl Pts',(18.7600723495991,0.619376388724522,3.87252485049244));
#61056=CARTESIAN_POINT('Ctrl Pts',(18.8077881856619,0.442207363551868,4.45202839763978));
#61057=CARTESIAN_POINT('Ctrl Pts',(18.8555040217248,-0.141047487806633,
4.61642731188217));
#61058=CARTESIAN_POINT('Ctrl Pts',(18.9032198577876,-0.594776260815313,
4.21475154067248));
#61059=CARTESIAN_POINT('Ctrl Pts',(18.9509356938505,-0.502312841712761,
3.615866125281));
#61060=CARTESIAN_POINT('Ctrl Pts',(18.9986515299133,0.0514321890198641,
3.36973675771293));
#61061=CARTESIAN_POINT('Ctrl Pts',(19.0463673659762,0.557946249173174,3.70238782336559));
#61062=CARTESIAN_POINT('Ctrl Pts',(19.0940832020389,0.552089683635207,4.30834073020757));
#61063=CARTESIAN_POINT('Ctrl Pts',(19.1417990381018,0.0392406665648073,
4.63113960000379));
#61064=CARTESIAN_POINT('Ctrl Pts',(19.1895148741646,-0.509643658296843,
4.3743532639067));
#61065=CARTESIAN_POINT('Ctrl Pts',(19.2372307102275,-0.590514370077448,
3.77379256516987));
#61066=CARTESIAN_POINT('Ctrl Pts',(19.2849465462903,-0.129106649190522,
3.38096163491845));
#61067=CARTESIAN_POINT('Ctrl Pts',(19.3326623823532,0.450861693465423,3.55660315963506));
#61068=CARTESIAN_POINT('Ctrl Pts',(19.380378218416,0.616796807017627,4.1394228269368));
#61069=CARTESIAN_POINT('Ctrl Pts',(19.4280940544789,0.216317919394901,4.59420836405745));
#61070=CARTESIAN_POINT('Ctrl Pts',(19.4758098905416,-0.382809037079938,
4.50332322288615));
#61071=CARTESIAN_POINT('Ctrl Pts',(19.5235257266046,-0.630396573984801,
3.95022861114352));
#61072=CARTESIAN_POINT('Ctrl Pts',(19.5712415626673,-0.299081219248977,
3.44283985120298));
#61073=CARTESIAN_POINT('Ctrl Pts',(19.6189573987302,0.306884987370396,3.44709979193512));
#61074=CARTESIAN_POINT('Ctrl Pts',(19.666673234793,0.631034051704256,3.95909657101937));
#61075=CARTESIAN_POINT('Ctrl Pts',(19.7143890708559,0.375694716468479,4.50865546647685));
#61076=CARTESIAN_POINT('Ctrl Pts',(19.7621049069187,-0.224650630777236,
4.59110846933868));
#61077=CARTESIAN_POINT('Ctrl Pts',(19.8098207429815,-0.618696275574682,
4.13073699938377));
#61078=CARTESIAN_POINT('Ctrl Pts',(19.8575365790444,-0.44458280157215,3.55030861879767));
#61079=CARTESIAN_POINT('Ctrl Pts',(19.9052524151072,0.13779637220375,3.3828370770856));
#61080=CARTESIAN_POINT('Ctrl Pts',(19.9529682511701,0.593637901716091,3.7821189081517));
#61081=CARTESIAN_POINT('Ctrl Pts',(20.0006840872329,0.504327165075627,4.38147832337345));
#61082=CARTESIAN_POINT('Ctrl Pts',(20.0483999232957,-0.0481046828163007,
4.63053160650705));
#61083=CARTESIAN_POINT('Ctrl Pts',(20.0961157593586,-0.556380679578279,
4.30053671048834));
#61084=CARTESIAN_POINT('Ctrl Pts',(20.1438315954214,-0.553687069357429,
3.69459455385474));
#61085=CARTESIAN_POINT('Ctrl Pts',(20.1915474314843,-0.0426033430871586,
3.36903495876776));
#61086=CARTESIAN_POINT('Ctrl Pts',(20.2392632675471,0.507734449822709,3.62304374442814));
#61087=CARTESIAN_POINT('Ctrl Pts',(20.2869791036099,0.591564791291533,4.22294595084339));
#61088=CARTESIAN_POINT('Ctrl Pts',(20.3346949396728,0.132620199007312,4.618629012875));
#61089=CARTESIAN_POINT('Ctrl Pts',(20.3824107757356,-0.449008129734859,
4.44521533979349));
#61090=CARTESIAN_POINT('Ctrl Pts',(20.4221739724547,-0.588594799935545,
3.96175478680276));
#61091=CARTESIAN_POINT('Ctrl Pts',(20.4539845298298,-0.419131055782338,
3.63395025773895));
#61092=CARTESIAN_POINT('Ctrl Pts',(20.4778424478613,-0.194099195253748,
3.47709810398663));
#61093=CARTESIAN_POINT('Ctrl Pts',(20.5017003658927,0.0810471032980313,
3.44846366347126));
#61094=CARTESIAN_POINT('Ctrl Pts',(20.5255582839241,0.334940048200093,3.55449674151986));
#61095=CARTESIAN_POINT('Ctrl Pts',(20.5494162019556,0.507694843328107,3.76957374638464));
#61096=CARTESIAN_POINT('Ctrl Pts',(20.5732741199869,0.555899439471162,4.04093981905292));
#61097=CARTESIAN_POINT('Ctrl Pts',(20.5971320380184,0.468386015874758,4.30232489481291));
#61098=CARTESIAN_POINT('Ctrl Pts',(20.6209899560498,0.266225827016684,4.48976745893774));
#61099=CARTESIAN_POINT('Ctrl Pts',(20.6448478740812,-0.000973650874560818,
4.55745692740964));
#61100=CARTESIAN_POINT('Ctrl Pts',(20.6687057921126,-0.267966914960919,
4.48882854939535));
#61101=CARTESIAN_POINT('Ctrl Pts',(20.6925637101441,-0.469418090387657,
4.30067062862012));
#61102=CARTESIAN_POINT('Ctrl Pts',(20.7164216281755,-0.556092695039732,
4.03898930289119));
#61103=CARTESIAN_POINT('Ctrl Pts',(20.7402795462069,-0.506782753954552,
3.7677746905255));
#61104=CARTESIAN_POINT('Ctrl Pts',(20.7641374642383,-0.333553132261349,
3.55334514249538));
#61105=CARTESIAN_POINT('Ctrl Pts',(20.7879953822697,-0.0787593560922578,
3.44813505886707));
#61106=CARTESIAN_POINT('Ctrl Pts',(20.8118533003012,0.19529252477751,3.47787088781106));
#61107=CARTESIAN_POINT('Ctrl Pts',(20.8357112183325,0.421590436108717,3.63528155911584));
#61108=CARTESIAN_POINT('Ctrl Pts',(20.859569136364,0.544797804677434,3.8818757964511));
#61109=CARTESIAN_POINT('Ctrl Pts',(20.8834270543954,0.534787374467886,4.15735463375504));
#61110=CARTESIAN_POINT('Ctrl Pts',(20.9072849724269,0.394006808563119,4.39435596913946));
#61111=CARTESIAN_POINT('Ctrl Pts',(20.9311428904582,0.156880874733563,4.53492653211281));
#61112=CARTESIAN_POINT('Ctrl Pts',(20.9550008084897,-0.118606721834374,
4.54469298471526));
#61113=CARTESIAN_POINT('Ctrl Pts',(20.9788587265211,-0.365091735913813,
4.42126716656144));
#61114=CARTESIAN_POINT('Ctrl Pts',(21.0027166445525,-0.522301880015273,
4.19483005048941));
#61115=CARTESIAN_POINT('Ctrl Pts',(21.0265745625839,-0.55179498493052,3.92075168033001));
#61116=CARTESIAN_POINT('Ctrl Pts',(21.0504324806153,-0.446359186657349,
3.66605168284066));
#61117=CARTESIAN_POINT('Ctrl Pts',(21.0742903986468,-0.231776408019839,
3.49301114555638));
#61118=CARTESIAN_POINT('Ctrl Pts',(21.0981483166782,0.0394820154987394,
3.44394319323497));
#61119=CARTESIAN_POINT('Ctrl Pts',(21.1220062347096,0.301086010940692,3.5308462768762));
#61120=CARTESIAN_POINT('Ctrl Pts',(21.145864152741,0.489066275193333,3.73247022529863));
#61121=CARTESIAN_POINT('Ctrl Pts',(21.1697220707724,0.557456513314207,3.9995124910074));
#61122=CARTESIAN_POINT('Ctrl Pts',(21.1935799888039,0.489533449092281,4.26667396594056));
#61123=CARTESIAN_POINT('Ctrl Pts',(21.2174379068352,0.30190612195814,4.46862639215028));
#61124=CARTESIAN_POINT('Ctrl Pts',(21.2412958248667,0.0404545242400231,
4.55598690035157));
#61125=CARTESIAN_POINT('Ctrl Pts',(21.2651537428981,-0.230889306609896,
4.50739346663836));
#61126=CARTESIAN_POINT('Ctrl Pts',(21.2890116609295,-0.445774412697373,
4.33472850921124));
#61127=CARTESIAN_POINT('Ctrl Pts',(21.312869578961,-0.551655532228011,4.08021331346062));
#61128=CARTESIAN_POINT('Ctrl Pts',(21.3367274969923,-0.522641847334507,
3.80608377760199));
#61129=CARTESIAN_POINT('Ctrl Pts',(21.3605854150238,-0.365827994289322,
3.57937204029158));
#61130=CARTESIAN_POINT('Ctrl Pts',(21.3844433330552,-0.119559231686077,
3.45551529680541));
#61131=CARTESIAN_POINT('Ctrl Pts',(21.4083012510867,0.155945019792583,3.46479989471587));
#61132=CARTESIAN_POINT('Ctrl Pts',(21.432159169118,0.393316466074861,3.60495549692644));
#61133=CARTESIAN_POINT('Ctrl Pts',(21.4560170871495,0.534511322676435,3.84171024093472));
#61134=CARTESIAN_POINT('Ctrl Pts',(21.4798750051809,0.545003601087511,4.11717114276091));
#61135=CARTESIAN_POINT('Ctrl Pts',(21.5037329232123,0.422227653432673,4.36398050850424));
#61136=CARTESIAN_POINT('Ctrl Pts',(21.5275908412437,0.196205543263173,4.52178672528827));
#61137=CARTESIAN_POINT('Ctrl Pts',(21.5514487592751,-0.0777941667658609,
4.5520018745543));
#61138=CARTESIAN_POINT('Ctrl Pts',(21.5753066773066,-0.332771083950078,
4.44723752926263));
#61139=CARTESIAN_POINT('Ctrl Pts',(21.5991645953379,-0.506376406606172,
4.23311142556056));
#61140=CARTESIAN_POINT('Ctrl Pts',(21.6230225133694,-0.556158904430687,
3.96198322848119));
#61141=CARTESIAN_POINT('Ctrl Pts',(21.6468804314008,-0.469945400657515,
3.70015116759423));
#61142=CARTESIAN_POINT('Ctrl Pts',(21.6707383494323,-0.268817445367881,
3.51164031394868));
#61143=CARTESIAN_POINT('Ctrl Pts',(21.6945962674636,-0.00195630224560004,
3.44254670619344));
#61144=CARTESIAN_POINT('Ctrl Pts',(21.7184541854951,0.26538321006433,3.50976561349676));
#61145=CARTESIAN_POINT('Ctrl Pts',(21.7423121035264,0.467829298620023,3.6968601820167));
#61146=CARTESIAN_POINT('Ctrl Pts',(21.766170021558,0.555878380248887,3.95808069339639));
#61147=CARTESIAN_POINT('Ctrl Pts',(21.7900279395893,0.508000056083844,4.22955161709966));
#61148=CARTESIAN_POINT('Ctrl Pts',(21.8138858576208,0.335901880562604,4.44489091756156));
#61149=CARTESIAN_POINT('Ctrl Pts',(21.8377437756521,0.0816665454602928,
4.55144227009437));
#61150=CARTESIAN_POINT('Ctrl Pts',(21.8616016936836,-0.192538484559094,
4.52315096660328));
#61151=CARTESIAN_POINT('Ctrl Pts',(21.885459611715,-0.419662610460766,4.36693500143146));
#61152=CARTESIAN_POINT('Ctrl Pts',(21.9093175297464,-0.544167796724789,
4.12099343330092));
#61153=CARTESIAN_POINT('Ctrl Pts',(21.9331754477779,-0.535609133856441,
3.84546567493331));
#61154=CARTESIAN_POINT('Ctrl Pts',(21.9570333658092,-0.396079448060293,
3.60772576847503));
#61155=CARTESIAN_POINT('Ctrl Pts',(21.9808912838407,-0.159697548225882,
3.46590759696012));
#61156=CARTESIAN_POINT('Ctrl Pts',(22.0047492018721,0.115734752223676,3.45468956637345));
#61157=CARTESIAN_POINT('Ctrl Pts',(22.0286071199035,0.362866753203085,3.5768147907664));
#61158=CARTESIAN_POINT('Ctrl Pts',(22.0524650379349,0.521267948732644,3.80242032615069));
#61159=CARTESIAN_POINT('Ctrl Pts',(22.0763229559664,0.552204931742854,4.07633947375325));
#61160=CARTESIAN_POINT('Ctrl Pts',(22.1001808739978,0.448112767182329,4.33159154057792));
#61161=CARTESIAN_POINT('Ctrl Pts',(22.1240387920292,0.23444482469764,4.5057604433585));
#61162=CARTESIAN_POINT('Ctrl Pts',(22.1478967100606,-0.0365512635718279,
4.55625714110116));
#61163=CARTESIAN_POINT('Ctrl Pts',(22.171754628092,-0.298609572266455,4.47073381570218));
#61164=CARTESIAN_POINT('Ctrl Pts',(22.1956125461234,-0.487649706571227,
4.2701032498363));
#61165=CARTESIAN_POINT('Ctrl Pts',(22.2194704641549,-0.557446204325542,
4.00342508191314));
#61166=CARTESIAN_POINT('Ctrl Pts',(22.2433283821863,-0.490931920559466,
3.73590938817905));
#61167=CARTESIAN_POINT('Ctrl Pts',(22.2671863002177,-0.304371409562025,
3.53297104269219));
#61168=CARTESIAN_POINT('Ctrl Pts',(22.2910442182491,-0.0433837978980346,
3.44423399893113));
#61169=CARTESIAN_POINT('Ctrl Pts',(22.3149021362806,0.228212333880327,3.49139688109763));
#61170=CARTESIAN_POINT('Ctrl Pts',(22.3387600543119,0.444004334066149,3.66292708008725));
#61171=CARTESIAN_POINT('Ctrl Pts',(22.3626179723434,0.551225179343846,3.91688078933633));
#61172=CARTESIAN_POINT('Ctrl Pts',(22.3864758903748,0.523656454698273,4.19115941035881));
#61173=CARTESIAN_POINT('Ctrl Pts',(22.4103338084062,0.368039459933637,4.41869434725418));
#61174=CARTESIAN_POINT('Ctrl Pts',(22.4341917264376,0.122426797365049,4.54384711353805));
#61175=CARTESIAN_POINT('Ctrl Pts',(22.458049644469,-0.153122562087755,4.53601444212637));
#61176=CARTESIAN_POINT('Ctrl Pts',(22.4819075625005,-0.391229265084309,
4.39711164706476));
#61177=CARTESIAN_POINT('Ctrl Pts',(22.5057654805319,-0.533669791868601,
4.16110422172694));
#61178=CARTESIAN_POINT('Ctrl Pts',(22.5296233985633,-0.545613449745194,
3.88570245498666));
#61179=CARTESIAN_POINT('Ctrl Pts',(22.5534813165947,-0.424139885198736,
3.63824949626794));
#61180=CARTESIAN_POINT('Ctrl Pts',(22.5773392346261,-0.198952323217499,
3.47925449370713));
#61181=CARTESIAN_POINT('Ctrl Pts',(22.6011971526576,0.0748840438856019,
3.44759575567767));
#61182=CARTESIAN_POINT('Ctrl Pts',(22.625055070689,0.330410085854462,3.55101527375816));
#61183=CARTESIAN_POINT('Ctrl Pts',(22.6489129887204,0.505140231362423,3.7642230866287));
#61184=CARTESIAN_POINT('Ctrl Pts',(22.6727709067518,0.556352908954721,4.03508610068096));
#61185=CARTESIAN_POINT('Ctrl Pts',(22.6966288247833,0.471516332128332,4.29736710820476));
#61186=CARTESIAN_POINT('Ctrl Pts',(22.7204867428146,0.27139215166714,4.48693847894857));
#61187=CARTESIAN_POINT('Ctrl Pts',(22.7443446608461,0.00488440565515616,
4.55743119390072));
#61188=CARTESIAN_POINT('Ctrl Pts',(22.7682025788775,-0.262778018495442,
4.49163382183027));
#61189=CARTESIAN_POINT('Ctrl Pts',(22.7920604969089,-0.466262514422727,
4.30558517247789));
#61190=CARTESIAN_POINT('Ctrl Pts',(22.8079657755965,-0.525793678117208,
4.1317859159904));
#61191=CARTESIAN_POINT('Ctrl Pts',(22.8159184149403,-0.532958495437544,
4.04301651477895));
#61192=CARTESIAN_POINT('Ctrl Pts',(3.98408158505965,-0.251304309929533,
3.59658905474035));
#61193=CARTESIAN_POINT('Ctrl Pts',(3.99203422440346,-0.184112308377066,
3.5547318870523));
#61194=CARTESIAN_POINT('Ctrl Pts',(4.00793950309107,-0.0284797076443847,
3.50528009766423));
#61195=CARTESIAN_POINT('Ctrl Pts',(4.03179742112249,0.212077873916637,3.55216010213054));
#61196=CARTESIAN_POINT('Ctrl Pts',(4.05565533915392,0.400711255741927,3.70851080938071));
#61197=CARTESIAN_POINT('Ctrl Pts',(4.07951325718533,0.49139298320592,3.93615790384083));
#61198=CARTESIAN_POINT('Ctrl Pts',(4.10337117521676,0.461898357851897,4.17940600742409));
#61199=CARTESIAN_POINT('Ctrl Pts',(4.12722909324816,0.319466186301668,4.37878980142624));
#61200=CARTESIAN_POINT('Ctrl Pts',(4.15108701127959,0.0989109688445654,
4.48554634140719));
#61201=CARTESIAN_POINT('Ctrl Pts',(4.174944929311,-0.145828100556353,4.47357507321567));
#61202=CARTESIAN_POINT('Ctrl Pts',(4.19880284734243,-0.354909590370033,
4.34580100620849));
#61203=CARTESIAN_POINT('Ctrl Pts',(4.22266076537384,-0.477205295803391,
4.13346959398438));
#61204=CARTESIAN_POINT('Ctrl Pts',(4.24651868340526,-0.482811689970624,
3.88850100783657));
#61205=CARTESIAN_POINT('Ctrl Pts',(4.27037660143669,-0.370357271909554,
3.67079708031066));
#61206=CARTESIAN_POINT('Ctrl Pts',(4.2942345194681,-0.167340519784032,3.53359217153378));
#61207=CARTESIAN_POINT('Ctrl Pts',(4.31809243749953,0.0765956044913427,
3.51043671457025));
#61208=CARTESIAN_POINT('Ctrl Pts',(4.34195035553093,0.301801986965541,3.60699279882218));
#61209=CARTESIAN_POINT('Ctrl Pts',(4.36580827356237,0.453209578636439,3.79964985833574));
#61210=CARTESIAN_POINT('Ctrl Pts',(4.38966619159377,0.493795074712635,4.04129798000377));
#61211=CARTESIAN_POINT('Ctrl Pts',(4.4135241096252,0.413634228782107,4.27284762322724));
#61212=CARTESIAN_POINT('Ctrl Pts',(4.43738202765661,0.23232854437776,4.43767858897425));
#61213=CARTESIAN_POINT('Ctrl Pts',(4.46123994568804,-0.00578779637616802,
4.49548521832112));
#61214=CARTESIAN_POINT('Ctrl Pts',(4.48509786371945,-0.242488863923451,
4.43213221465579));
#61215=CARTESIAN_POINT('Ctrl Pts',(4.50895578175088,-0.419894798625899,
4.26311111366653));
#61216=CARTESIAN_POINT('Ctrl Pts',(4.53281369978229,-0.494625017545811,
4.02975217827461));
#61217=CARTESIAN_POINT('Ctrl Pts',(4.55667161781372,-0.448405946262215,
3.78911802491887));
#61218=CARTESIAN_POINT('Ctrl Pts',(4.58052953584513,-0.292539406836986,
3.60005025874973));
#61219=CARTESIAN_POINT('Ctrl Pts',(4.60438745387655,-0.0651390137990107,
3.50878109874461));
#61220=CARTESIAN_POINT('Ctrl Pts',(4.62824537190797,0.178189642449287,3.53762834062211));
#61221=CARTESIAN_POINT('Ctrl Pts',(4.65210328993938,0.377946077338085,3.67953804797316));
#61222=CARTESIAN_POINT('Ctrl Pts',(4.67596120797081,0.485284401269169,3.89980943180067));
#61223=CARTESIAN_POINT('Ctrl Pts',(4.69981912600222,0.473957470210434,4.14458013869048));
#61224=CARTESIAN_POINT('Ctrl Pts',(4.72367704403364,0.34673502734182,4.35399706338589));
#61225=CARTESIAN_POINT('Ctrl Pts',(4.74753496206506,0.134726425416229,4.47685206339739));
#61226=CARTESIAN_POINT('Ctrl Pts',(4.77139288009648,-0.110226457398098,
4.48310374471865));
#61227=CARTESIAN_POINT('Ctrl Pts',(4.7952507981279,-0.328225968870003,4.37122340097448));
#61228=CARTESIAN_POINT('Ctrl Pts',(4.81910871615932,-0.465965290257402,
4.16856882376961));
#61229=CARTESIAN_POINT('Ctrl Pts',(4.84296663419074,-0.489763405537152,
3.92469457743051));
#61230=CARTESIAN_POINT('Ctrl Pts',(4.86682455222216,-0.393801027275785,
3.69923455818817));
#61231=CARTESIAN_POINT('Ctrl Pts',(4.89068247025357,-0.201543570920867,
3.54731988215497));
#61232=CARTESIAN_POINT('Ctrl Pts',(4.914540388285,0.039996778460842,3.50609782569371));
#61233=CARTESIAN_POINT('Ctrl Pts',(4.93839830631641,0.271756826018508,3.58564830447545));
#61234=CARTESIAN_POINT('Ctrl Pts',(4.96225622434784,0.437064927107334,3.76651905952651));
#61235=CARTESIAN_POINT('Ctrl Pts',(4.98611414237925,0.495498748108838,4.00448226441646));
#61236=CARTESIAN_POINT('Ctrl Pts',(5.00997206041068,0.432769628082826,4.24134943356216));
#61237=CARTESIAN_POINT('Ctrl Pts',(5.03382997844209,0.26421654558258,4.41920009197534));
#61238=CARTESIAN_POINT('Ctrl Pts',(5.05768789647352,0.031055320573195,4.49454490911931));
#61239=CARTESIAN_POINT('Ctrl Pts',(5.08154581450493,-0.209699776246285,
4.44896002485074));
#61240=CARTESIAN_POINT('Ctrl Pts',(5.10540373253635,-0.399177565666329,
4.29359218508065));
#61241=CARTESIAN_POINT('Ctrl Pts',(5.12926165056777,-0.491045566902382,
4.06643305876778));
#61242=CARTESIAN_POINT('Ctrl Pts',(5.15311956859918,-0.462839551218119,
3.823029239986));
#61243=CARTESIAN_POINT('Ctrl Pts',(5.17697748663061,-0.321456657764784,
3.62289959261435));
#61244=CARTESIAN_POINT('Ctrl Pts',(5.20083540466202,-0.101468855184408,
3.51498126685736));
#61245=CARTESIAN_POINT('Ctrl Pts',(5.22469332269345,0.143330846444675,3.52566323299877));
#61246=CARTESIAN_POINT('Ctrl Pts',(5.24855124072486,0.353082251864168,3.6523334593461));
#61247=CARTESIAN_POINT('Ctrl Pts',(5.27240915875629,0.476495428935435,3.86401762512973));
#61248=CARTESIAN_POINT('Ctrl Pts',(5.2962670767877,0.483392494157105,4.10895318565465));
#61249=CARTESIAN_POINT('Ctrl Pts',(5.32012499481913,0.372086927210194,4.32724672446184));
#61250=CARTESIAN_POINT('Ctrl Pts',(5.34398291285054,0.169795971115995,4.46551952511629));
#61251=CARTESIAN_POINT('Ctrl Pts',(5.36784083088196,-0.0740147250654609,
4.48996012138256));
#61252=CARTESIAN_POINT('Ctrl Pts',(5.39169874891337,-0.299726804847767,
4.39459212172504));
#61253=CARTESIAN_POINT('Ctrl Pts',(5.4155566669448,-0.452147516450583,4.20273559983216));
#61254=CARTESIAN_POINT('Ctrl Pts',(5.43941458497621,-0.494005844030112,
3.96130470137348));
#61255=CARTESIAN_POINT('Ctrl Pts',(5.46327250300764,-0.415066286295368,
3.72933585746768));
#61256=CARTESIAN_POINT('Ctrl Pts',(5.48713042103905,-0.234631715382576,
3.56355176915442));
#61257=CARTESIAN_POINT('Ctrl Pts',(5.51098833907048,0.00317670118048804,
3.50449116189365));
#61258=CARTESIAN_POINT('Ctrl Pts',(5.53484625710188,0.240208327774024,3.56659596294035));
#61259=CARTESIAN_POINT('Ctrl Pts',(5.55870417513332,0.418502475082003,3.73467985673571));
#61260=CARTESIAN_POINT('Ctrl Pts',(5.58256209316472,0.494461367456411,3.96764175273735));
#61261=CARTESIAN_POINT('Ctrl Pts',(5.60642001119615,0.449510986625754,4.20851612161082));
#61262=CARTESIAN_POINT('Ctrl Pts',(5.63027792922757,0.294642925140636,4.39840261889448));
#61263=CARTESIAN_POINT('Ctrl Pts',(5.65413584725899,0.0677266425295592,
4.49086882357174));
#61264=CARTESIAN_POINT('Ctrl Pts',(5.6779937652904,-0.17575064898472,4.46330422991997));
#61265=CARTESIAN_POINT('Ctrl Pts',(5.70185168332183,-0.376252119531055,
4.32244913183746));
#61266=CARTESIAN_POINT('Ctrl Pts',(5.72570960135325,-0.48474969783608,4.10274643779879));
#61267=CARTESIAN_POINT('Ctrl Pts',(5.74956751938466,-0.474712770918799,
3.85791944074229));
#61268=CARTESIAN_POINT('Ctrl Pts',(5.77342543741608,-0.348595640189148,
3.64783501103505));
#61269=CARTESIAN_POINT('Ctrl Pts',(5.7972833554475,-0.13723738064616,3.52386451312966));
#61270=CARTESIAN_POINT('Ctrl Pts',(5.82114127347893,0.1076791581852,3.5163221129105));
#61271=CARTESIAN_POINT('Ctrl Pts',(5.84499919151033,0.326265206982528,3.62705212841851));
#61272=CARTESIAN_POINT('Ctrl Pts',(5.86885710954176,0.465070530553655,3.82897806268729));
#61273=CARTESIAN_POINT('Ctrl Pts',(5.89271502757317,0.490153431381492,4.07272350923538));
#61274=CARTESIAN_POINT('Ctrl Pts',(5.9165729456046,0.395380485146506,4.29868609559117));
#61275=CARTESIAN_POINT('Ctrl Pts',(5.94043086363601,0.203926205561759,4.45161176009809));
#61276=CARTESIAN_POINT('Ctrl Pts',(5.96428878166744,-0.0373935204432717,
4.49410611450448));
#61277=CARTESIAN_POINT('Ctrl Pts',(5.98814669969885,-0.26956963613406,4.41577793841189));
#61278=CARTESIAN_POINT('Ctrl Pts',(6.01200461773027,-0.435828398698505,
4.23578096933615));
#61279=CARTESIAN_POINT('Ctrl Pts',(6.0358625357617,-0.495515688199628,3.99812868033461));
#61280=CARTESIAN_POINT('Ctrl Pts',(6.0597204537931,-0.434035059498629,3.76093483037113));
#61281=CARTESIAN_POINT('Ctrl Pts',(6.08357837182454,-0.266422612259865,
3.58219732064663));
#61282=CARTESIAN_POINT('Ctrl Pts',(6.10743628985594,-0.0336596025775484,
3.50562697870369));
#61283=CARTESIAN_POINT('Ctrl Pts',(6.13129420788738,0.207328476491996,3.54993858195554));
#61284=CARTESIAN_POINT('Ctrl Pts',(6.15515212591877,0.397629707835022,3.70431327123879));
#61285=CARTESIAN_POINT('Ctrl Pts',(6.17901004395022,0.490679606253205,3.93097100878581));
#61286=CARTESIAN_POINT('Ctrl Pts',(6.20286796198161,0.463782811036945,4.17454675550933));
#61287=CARTESIAN_POINT('Ctrl Pts',(6.22672588001306,0.323407044622774,4.3753682944706));
#61288=CARTESIAN_POINT('Ctrl Pts',(6.25058379804445,0.104084330837213,4.48453946106473));
#61289=CARTESIAN_POINT('Ctrl Pts',(6.27444171607588,-0.140944443623038,
4.4749681472433));
#61290=CARTESIAN_POINT('Ctrl Pts',(6.29829963410731,-0.351028389709017,
4.349743491311));
#61291=CARTESIAN_POINT('Ctrl Pts',(6.32215755213872,-0.476177279109797,
4.13807688197341));
#61292=CARTESIAN_POINT('Ctrl Pts',(6.34601547017014,-0.483231738207782,
3.89435343878414));
#61293=CARTESIAN_POINT('Ctrl Pts',(6.37782602754537,-0.338784024988664,
3.5998542259592));
#61294=CARTESIAN_POINT('Ctrl Pts',(6.41758922426439,0.0803770223010952,
3.44371490521648));
#61295=CARTESIAN_POINT('Ctrl Pts',(6.46530506032724,0.512014121509362,3.7673575683149));
#61296=CARTESIAN_POINT('Ctrl Pts',(6.51302089639006,0.472271980317209,4.30452828893312));
#61297=CARTESIAN_POINT('Ctrl Pts',(6.56073673245292,-0.000548856210248058,
4.56210751581942));
#61298=CARTESIAN_POINT('Ctrl Pts',(6.60845256851575,-0.473190198344468,
4.30346185287483));
#61299=CARTESIAN_POINT('Ctrl Pts',(6.65616840457859,-0.511122033036262,
3.76615996983968));
#61300=CARTESIAN_POINT('Ctrl Pts',(6.70388424064142,-0.0797735308749388,
3.44358772816382));
#61301=CARTESIAN_POINT('Ctrl Pts',(6.75160007670426,0.424880365184703,3.63198234005898));
#61302=CARTESIAN_POINT('Ctrl Pts',(6.7993159127671,0.539334593204737,4.15833063512042));
#61303=CARTESIAN_POINT('Ctrl Pts',(6.84703174882994,0.158523065679302,4.53928284691909));
#61304=CARTESIAN_POINT('Ctrl Pts',(6.89474758489278,-0.367869781963911,
4.42500259414721));
#61305=CARTESIAN_POINT('Ctrl Pts',(6.94246342095561,-0.556438361909488,
3.92043630538129));
#61306=CARTESIAN_POINT('Ctrl Pts',(6.99017925701846,-0.234023037562683,
3.48893437735136));
#61307=CARTESIAN_POINT('Ctrl Pts',(7.03789509308128,0.303300305128555,3.52675198254107));
#61308=CARTESIAN_POINT('Ctrl Pts',(7.08561092914413,0.562097748282813,3.99916046672433));
#61309=CARTESIAN_POINT('Ctrl Pts',(7.13332676520696,0.304712478085684,4.47233993757656));
#61310=CARTESIAN_POINT('Ctrl Pts',(7.18104260126981,-0.232495107101315,
4.51176235979777));
#61311=CARTESIAN_POINT('Ctrl Pts',(7.22875843733264,-0.556198774489988,
4.08122554105153));
#61312=CARTESIAN_POINT('Ctrl Pts',(7.27647427339549,-0.369136593294786,
3.57609805363465));
#61313=CARTESIAN_POINT('Ctrl Pts',(7.32419010945832,0.156909424853758,3.46024624852207));
#61314=CARTESIAN_POINT('Ctrl Pts',(7.37190594552116,0.538863091386428,3.84005861730642));
#61315=CARTESIAN_POINT('Ctrl Pts',(7.41962178158399,0.425970496197337,4.36674761950234));
#61316=CARTESIAN_POINT('Ctrl Pts',(7.46733761764684,-0.0780973635293338,
4.55664663921719));
#61317=CARTESIAN_POINT('Ctrl Pts',(7.51505345370967,-0.510447210801067,
4.2353684852172));
#61318=CARTESIAN_POINT('Ctrl Pts',(7.56276928977251,-0.474045531130633,
3.69794782953315));
#61319=CARTESIAN_POINT('Ctrl Pts',(7.61048512583535,-0.00232054557778912,
3.43790632971152));
#61320=CARTESIAN_POINT('Ctrl Pts',(7.65820096189818,0.471535432411473,3.69404409621074));
#61321=CARTESIAN_POINT('Ctrl Pts',(7.70591679796103,0.512373167457076,4.23114587691112));
#61322=CARTESIAN_POINT('Ctrl Pts',(7.75363263402387,0.0826907388754792,
4.55598284219971));
#61323=CARTESIAN_POINT('Ctrl Pts',(7.80134847008669,-0.422927867535356,
4.3702522086048));
#61324=CARTESIAN_POINT('Ctrl Pts',(7.84906430614955,-0.540165305628305,
3.84451327478339));
#61325=CARTESIAN_POINT('Ctrl Pts',(7.89678014221237,-0.161360632039799,
3.46156019320034));
#61326=CARTESIAN_POINT('Ctrl Pts',(7.94449597827521,0.365623992797271,3.57306467116217));
#61327=CARTESIAN_POINT('Ctrl Pts',(7.99221181433806,0.556850479203549,4.07663043084052));
#61328=CARTESIAN_POINT('Ctrl Pts',(8.03992765040089,0.236712602309549,4.50982528676712));
#61329=CARTESIAN_POINT('Ctrl Pts',(8.08764348646373,-0.300802099575971,
4.47483973718518));
#61330=CARTESIAN_POINT('Ctrl Pts',(8.13535932252656,-0.562085604986122,
4.00380155059756));
#61331=CARTESIAN_POINT('Ctrl Pts',(8.18307515858941,-0.307197250538534,
3.52927234160183));
#61332=CARTESIAN_POINT('Ctrl Pts',(8.23079099465223,0.229795065915734,3.48701958438918));
#61333=CARTESIAN_POINT('Ctrl Pts',(8.27850683071509,0.555763037488074,3.91584463605021));
#61334=CARTESIAN_POINT('Ctrl Pts',(8.32622266677791,0.371365260221553,4.42195085332305));
#61335=CARTESIAN_POINT('Ctrl Pts',(8.37393850284076,-0.154062949695418,
4.54057310944092));
#61336=CARTESIAN_POINT('Ctrl Pts',(8.4216543389036,-0.538012782343907,4.16277876137275));
#61337=CARTESIAN_POINT('Ctrl Pts',(8.46937017496643,-0.427897198575242,
3.6355021720628));
#61338=CARTESIAN_POINT('Ctrl Pts',(8.51708601102927,0.0751629666897603,
3.44294954666756));
#61339=CARTESIAN_POINT('Ctrl Pts',(8.56480184709211,0.50919982311266,3.76194492389047));
#61340=CARTESIAN_POINT('Ctrl Pts',(8.61251768315494,0.475630646924824,4.29954994045293));
#61341=CARTESIAN_POINT('Ctrl Pts',(8.66023351921779,0.00528252914771292,
4.56207363752918));
#61342=CARTESIAN_POINT('Ctrl Pts',(8.70794935528062,-0.469916616427902,
4.30843646464781));
#61343=CARTESIAN_POINT('Ctrl Pts',(8.75566519134346,-0.513584102541225,
3.7715573403753));
#61344=CARTESIAN_POINT('Ctrl Pts',(8.8033810274063,-0.0856194047837525,
3.44446062547832));
#61345=CARTESIAN_POINT('Ctrl Pts',(8.85109686346913,0.420970909810523,3.6275242662766));
#61346=CARTESIAN_POINT('Ctrl Pts',(8.89881269953199,0.540977160455745,4.15263810462895));
#61347=CARTESIAN_POINT('Ctrl Pts',(8.9465285355948,0.1641957606509,4.5375820228614));
#61348=CARTESIAN_POINT('Ctrl Pts',(8.99424437165766,-0.363369132636193,
4.42885609773758));
#61349=CARTESIAN_POINT('Ctrl Pts',(9.04196020772048,-0.557246560270691,
3.92630501926208));
#61350=CARTESIAN_POINT('Ctrl Pts',(9.08967604378333,-0.239395897268157,
3.49142917554125));
#61351=CARTESIAN_POINT('Ctrl Pts',(9.13739187984617,0.298295701775085,3.52358174528888));
#61352=CARTESIAN_POINT('Ctrl Pts',(9.18510771590899,0.562057768008922,3.99323652897485));
#61353=CARTESIAN_POINT('Ctrl Pts',(9.23282355197185,0.309673537509763,4.46910231217259));
#61354=CARTESIAN_POINT('Ctrl Pts',(9.28053938803466,-0.227088667424462,
4.51418422403538));
#61355=CARTESIAN_POINT('Ctrl Pts',(9.32825522409753,-0.555311854854516,
4.08708285122523));
#61356=CARTESIAN_POINT('Ctrl Pts',(9.37597106016035,-0.373583621400482,
3.58001195619306));
#61357=CARTESIAN_POINT('Ctrl Pts',(9.4236868962232,0.151212199908504,3.45862254413551));
#61358=CARTESIAN_POINT('Ctrl Pts',(9.47140273228603,0.537147531342748,3.83438837996121));
#61359=CARTESIAN_POINT('Ctrl Pts',(9.51911856834887,0.429812019667804,4.36223791473086));
#61360=CARTESIAN_POINT('Ctrl Pts',(9.5668344044117,-0.0722264831760907,
4.5574387986564));
#61361=CARTESIAN_POINT('Ctrl Pts',(9.61455024047456,-0.507938295172089,
4.24073505647735));
#61362=CARTESIAN_POINT('Ctrl Pts',(9.66226607653738,-0.477202555076283,
3.70296060775017));
#61363=CARTESIAN_POINT('Ctrl Pts',(9.70998191260023,-0.00824436594879979,
3.43796200346455));
#61364=CARTESIAN_POINT('Ctrl Pts',(9.75769774866306,0.46828475128534,3.68909153946361));
#61365=CARTESIAN_POINT('Ctrl Pts',(9.80541358472589,0.514780775927077,4.22573309871483));
#61366=CARTESIAN_POINT('Ctrl Pts',(9.85312942078874,0.0885456931146035,
4.55508048006603));
#61367=CARTESIAN_POINT('Ctrl Pts',(9.90084525685159,-0.419002262135622,
4.37468891556157));
#61368=CARTESIAN_POINT('Ctrl Pts',(9.9485610929144,-0.541773992888202,3.8502147545669));
#61369=CARTESIAN_POINT('Ctrl Pts',(9.99627692897727,-0.167026329707142,
3.46329068919569));
#61370=CARTESIAN_POINT('Ctrl Pts',(10.0439927650401,0.361104182074418,3.56923504227033));
#61371=CARTESIAN_POINT('Ctrl Pts',(10.0917086011029,0.557627167155001,4.07075748419897));
#61372=CARTESIAN_POINT('Ctrl Pts',(10.1394244371657,0.242072544440304,4.50730223964386));
#61373=CARTESIAN_POINT('Ctrl Pts',(10.1871402732286,-0.295781020598791,
4.47798354257549));
#61374=CARTESIAN_POINT('Ctrl Pts',(10.2348561092914,-0.56201432324602,4.00972520363789));
#61375=CARTESIAN_POINT('Ctrl Pts',(10.2825719453543,-0.312141225154507,
3.53253606055812));
#61376=CARTESIAN_POINT('Ctrl Pts',(10.3302877814171,0.224375962906492,3.48462624592509));
#61377=CARTESIAN_POINT('Ctrl Pts',(10.37800361748,0.554845251762499,3.90999207970357));
#61378=CARTESIAN_POINT('Ctrl Pts',(10.4257194535428,0.375791608533427,4.41801357164013));
#61379=CARTESIAN_POINT('Ctrl Pts',(10.4734352896056,-0.148357251109035,
4.54216676877402));
#61380=CARTESIAN_POINT('Ctrl Pts',(10.5211511256685,-0.536267364288337,
4.16843987983467));
#61381=CARTESIAN_POINT('Ctrl Pts',(10.5688669617313,-0.431714905307627,
3.64003205746247));
#61382=CARTESIAN_POINT('Ctrl Pts',(10.6165827977942,0.0692879940047382,
3.44218833554121));
#61383=CARTESIAN_POINT('Ctrl Pts',(10.664298633857,0.50666266228973,3.75659164812817));
#61384=CARTESIAN_POINT('Ctrl Pts',(10.7120144699198,0.478761211786921,4.29452059555793));
#61385=CARTESIAN_POINT('Ctrl Pts',(10.7597303059827,0.0112059738120427,
4.56198674830498));
#61386=CARTESIAN_POINT('Ctrl Pts',(10.8074461420455,-0.466639882340508,
4.31337182280594));
#61387=CARTESIAN_POINT('Ctrl Pts',(10.8551619781083,-0.515963154362253,
3.77698273057893));
#61388=CARTESIAN_POINT('Ctrl Pts',(10.9028778141712,-0.0914695226195351,
3.44539382842306));
#61389=CARTESIAN_POINT('Ctrl Pts',(10.950593650234,0.417021979184216,3.62310830733915));
#61390=CARTESIAN_POINT('Ctrl Pts',(10.9983094862969,0.542555780795161,4.14692822684982));
#61391=CARTESIAN_POINT('Ctrl Pts',(11.0460253223597,0.169852260608159,4.53582169486292));
#61392=CARTESIAN_POINT('Ctrl Pts',(11.0937411584225,-0.358829204008283,
4.43266185580689));
#61393=CARTESIAN_POINT('Ctrl Pts',(11.1414569944853,-0.55799228928692,3.93218197720501));
#61394=CARTESIAN_POINT('Ctrl Pts',(11.1891728305482,-0.244742469498405,
3.49398043245019));
#61395=CARTESIAN_POINT('Ctrl Pts',(11.236888666611,0.293258125877444,3.5204644426882));
#61396=CARTESIAN_POINT('Ctrl Pts',(11.2846045026739,0.561955271903759,3.98731333380864));
#61397=CARTESIAN_POINT('Ctrl Pts',(11.3323203387367,0.314600244947554,4.46581258570203));
#61398=CARTESIAN_POINT('Ctrl Pts',(11.3800361747996,-0.221657027690976,
4.51654897269734));
#61399=CARTESIAN_POINT('Ctrl Pts',(11.4277520108624,-0.554363241169119,
4.0929304899371));
#61400=CARTESIAN_POINT('Ctrl Pts',(11.4754678469252,-0.377989160306769,
3.58397250834823));
#61401=CARTESIAN_POINT('Ctrl Pts',(11.5231836829881,0.145498182576105,3.45705897374896));
#61402=CARTESIAN_POINT('Ctrl Pts',(11.5708995190509,0.535372305622036,3.82873653777755));
#61403=CARTESIAN_POINT('Ctrl Pts',(11.6186153551137,0.43360580265347,4.35768797439208));
#61404=CARTESIAN_POINT('Ctrl Pts',(11.6663311911766,-0.0663475807746441,
4.55816904038548));
#61405=CARTESIAN_POINT('Ctrl Pts',(11.7140470272394,-0.505372959888646,
4.24607488805821));
#61406=CARTESIAN_POINT('Ctrl Pts',(11.7617628633023,-0.480306573774387,
3.70800637967828));
#61407=CARTESIAN_POINT('Ctrl Pts',(11.8094786993651,-0.0141672704965164,
3.43808010573911));
#61408=CARTESIAN_POINT('Ctrl Pts',(11.8571945354279,0.464982055269784,3.68417351694868));
#61409=CARTESIAN_POINT('Ctrl Pts',(11.9049103714908,0.517131205013274,4.22029524715934));
#61410=CARTESIAN_POINT('Ctrl Pts',(11.9526262075536,0.0943908121067024,
4.55411646222552));
#61411=CARTESIAN_POINT('Ctrl Pts',(12.0003420436165,-0.415030115946784,
4.37908400385228));
#61412=CARTESIAN_POINT('Ctrl Pts',(12.0480578796793,-0.543322502467158,
3.85593287178435));
#61413=CARTESIAN_POINT('Ctrl Pts',(12.0957737157421,-0.172673474880652,
3.46508080031456));
#61414=CARTESIAN_POINT('Ctrl Pts',(12.143489551805,0.356544261611682,3.56545326070575));
#61415=CARTESIAN_POINT('Ctrl Pts',(12.1912053878678,0.558341916527368,4.06487667815191));
#61416=CARTESIAN_POINT('Ctrl Pts',(12.2389212239306,0.247405598301292,4.50472284379514));
#61417=CARTESIAN_POINT('Ctrl Pts',(12.2866370599935,-0.290727087669313,
4.48107425582212));
#61418=CARTESIAN_POINT('Ctrl Pts',(12.3343528960563,-0.56188061562194,4.01564777644873));
#61419=CARTESIAN_POINT('Ctrl Pts',(12.3820687321191,-0.317050528604376,
3.5358517031905));
#61420=CARTESIAN_POINT('Ctrl Pts',(12.429784568182,0.218931937280033,3.48229015273196));
#61421=CARTESIAN_POINT('Ctrl Pts',(12.4775004042448,0.553865836459325,3.90414952100961));
#61422=CARTESIAN_POINT('Ctrl Pts',(12.5252162403077,0.380176215696692,4.4140298589933));
#61423=CARTESIAN_POINT('Ctrl Pts',(12.5729320763705,-0.142635073703209,
4.54370020679522));
#61424=CARTESIAN_POINT('Ctrl Pts',(12.6206479124333,-0.53446238019874,4.17408228879405));
#61425=CARTESIAN_POINT('Ctrl Pts',(12.6683637484962,-0.435484659196984,
3.644601926393));
#61426=CARTESIAN_POINT('Ctrl Pts',(12.716079584559,0.0634053251381518,3.44148908348752));
#61427=CARTESIAN_POINT('Ctrl Pts',(12.7637954206219,0.504069223782589,3.75126540901054));
#61428=CARTESIAN_POINT('Ctrl Pts',(12.8115112566847,0.481838598125516,4.2894585367128));
#61429=CARTESIAN_POINT('Ctrl Pts',(12.8592270927475,0.0171281737699642,
4.56183743625962));
#61430=CARTESIAN_POINT('Ctrl Pts',(12.9069429288104,-0.463311316109371,
4.31827237310907));
#61431=CARTESIAN_POINT('Ctrl Pts',(12.9546587648732,-0.518284895444539,
3.78243289248252));
#61432=CARTESIAN_POINT('Ctrl Pts',(13.0023746009361,-0.0973094804548018,
3.44638863438952));
#61433=CARTESIAN_POINT('Ctrl Pts',(13.0500904369989,0.413026727735397,3.61873421174243));
#61434=CARTESIAN_POINT('Ctrl Pts',(13.0978062730617,0.544074136613086,4.14120202898048));
#61435=CARTESIAN_POINT('Ctrl Pts',(13.1455221091246,0.17548989418231,4.53400185033327));
#61436=CARTESIAN_POINT('Ctrl Pts',(13.1932379451874,-0.354249418335187,
4.4364195558504));
#61437=CARTESIAN_POINT('Ctrl Pts',(13.2409537812502,-0.558676039167545,
3.93806646805208));
#61438=CARTESIAN_POINT('Ctrl Pts',(13.2886696173131,-0.250061856896528,
3.49658789561142));
#61439=CARTESIAN_POINT('Ctrl Pts',(13.3363854533759,0.288187976258808,3.51740040462167));
#61440=CARTESIAN_POINT('Ctrl Pts',(13.3841012894388,0.56179035647369,3.9813915478171));
#61441=CARTESIAN_POINT('Ctrl Pts',(13.4318171255016,0.319492008083037,4.46247111897993));
#61442=CARTESIAN_POINT('Ctrl Pts',(13.4795329615644,-0.21620076734671,4.51885634555065));
#61443=CARTESIAN_POINT('Ctrl Pts',(13.5272487976273,-0.553353051445561,
4.09876780637113));
#61444=CARTESIAN_POINT('Ctrl Pts',(13.5749646336901,-0.382352713970831,
3.58797927086295));
#61445=CARTESIAN_POINT('Ctrl Pts',(13.6226804697529,0.139768003996038,3.45555571067516));
#61446=CARTESIAN_POINT('Ctrl Pts',(13.6703963058158,0.53353761328617,3.82310371872654));
#61447=CARTESIAN_POINT('Ctrl Pts',(13.7181121418786,0.437351422764197,4.35309830377052));
#61448=CARTESIAN_POINT('Ctrl Pts',(13.7658279779415,-0.0604613087987784,
4.55883728334624));
#61449=CARTESIAN_POINT('Ctrl Pts',(13.8135438140043,-0.502751490175015,
4.25138738680826));
#61450=CARTESIAN_POINT('Ctrl Pts',(13.8612596500671,-0.483357242297515,
3.71308458487209));
#61451=CARTESIAN_POINT('Ctrl Pts',(13.90897548613,-0.0200886014110514,3.43826062340902));
#61452=CARTESIAN_POINT('Ctrl Pts',(13.9566913221928,0.461627711254046,3.67929057494076));
#61453=CARTESIAN_POINT('Ctrl Pts',(14.0044071582557,0.519424193619207,4.21483292625321));
#61454=CARTESIAN_POINT('Ctrl Pts',(14.0521229943185,0.100225446615308,4.55309089575788));
#61455=CARTESIAN_POINT('Ctrl Pts',(14.0998388303813,-0.411011870182152,
4.38343698529073));
#61456=CARTESIAN_POINT('Ctrl Pts',(14.1475546664441,-0.544810662360815,
3.86166699129474));
#61457=CARTESIAN_POINT('Ctrl Pts',(14.195270502507,-0.178301440303968,3.46693032771971));
#61458=CARTESIAN_POINT('Ctrl Pts',(14.2429863385698,0.351944737904315,3.5617197465309));
#61459=CARTESIAN_POINT('Ctrl Pts',(14.2907021746327,0.558994647929194,4.05898866591129));
#61460=CARTESIAN_POINT('Ctrl Pts',(14.3384180106955,0.252711171522458,4.50208738572805));
#61461=CARTESIAN_POINT('Ctrl Pts',(14.3861338467583,-0.28564086215454,4.48411153362329));
#61462=CARTESIAN_POINT('Ctrl Pts',(14.4338496828212,-0.561684496965419,
4.02156861117883));
#61463=CARTESIAN_POINT('Ctrl Pts',(14.481565518884,-0.321924615586062,3.53921890121312));
#61464=CARTESIAN_POINT('Ctrl Pts',(14.5292813549469,0.213463593732893,3.48001156429194));
#61465=CARTESIAN_POINT('Ctrl Pts',(14.5769971910097,0.552824900367352,3.89831760893199));
#61466=CARTESIAN_POINT('Ctrl Pts',(14.6247130270725,0.384518594689996,4.4100001578745));
#61467=CARTESIAN_POINT('Ctrl Pts',(14.6724288631354,-0.136897053070264,
4.54517325317752));
#61468=CARTESIAN_POINT('Ctrl Pts',(14.7201446991982,-0.532598030564186,
4.17970536151887));
#61469=CARTESIAN_POINT('Ctrl Pts',(14.7678605352611,-0.439206041516937,
3.64921127125505));
#61470=CARTESIAN_POINT('Ctrl Pts',(14.8155763713239,0.0575156135089261,
3.44085186817608));
#61471=CARTESIAN_POINT('Ctrl Pts',(14.8632922073868,0.501419795658073,3.74596679815093));
#61472=CARTESIAN_POINT('Ctrl Pts',(14.9110080434496,0.484862464119148,4.284364326187));
#61473=CARTESIAN_POINT('Ctrl Pts',(14.9587238795124,0.0230484712116303,
4.56162571797798));
#61474=CARTESIAN_POINT('Ctrl Pts',(15.0064397155752,-0.459931287455839,
4.32313757122732));
#61475=CARTESIAN_POINT('Ctrl Pts',(15.0541555516381,-0.5205490679001,3.78790722070797));
#61476=CARTESIAN_POINT('Ctrl Pts',(15.1018713877009,-0.103138629614742,
3.44744493287938));
#61477=CARTESIAN_POINT('Ctrl Pts',(15.1495872237638,0.40898559923764,3.61440246534021));
#61478=CARTESIAN_POINT('Ctrl Pts',(15.1973030598266,0.545532059257757,4.13546014705983));
#61479=CARTESIAN_POINT('Ctrl Pts',(15.2450188958894,0.181108035171788,4.53212269141213));
#61480=CARTESIAN_POINT('Ctrl Pts',(15.2927347319523,-0.349630284317748,
4.44012878048063));
#61481=CARTESIAN_POINT('Ctrl Pts',(15.3404505680151,-0.559297733964875,
3.94395783818199));
#61482=CARTESIAN_POINT('Ctrl Pts',(15.3881664040779,-0.255353468610234,
3.49925127540033));
#61483=CARTESIAN_POINT('Ctrl Pts',(15.4358822401408,0.283085816087337,3.51438997142805));
#61484=CARTESIAN_POINT('Ctrl Pts',(15.4835980762036,0.561563040036739,3.97547182876414));
#61485=CARTESIAN_POINT('Ctrl Pts',(15.5313139122665,0.324348283562367,4.45907828316053));
#61486=CARTESIAN_POINT('Ctrl Pts',(15.5790297483293,-0.210720492447169,
4.52110608630326));
#61487=CARTESIAN_POINT('Ctrl Pts',(15.6267455843921,-0.552281397890927,
4.10459415214592));
#61488=CARTESIAN_POINT('Ctrl Pts',(15.674461420455,-0.386673797709831,3.59203179868507));
#61489=CARTESIAN_POINT('Ctrl Pts',(15.7221772565178,0.134022300649356,3.45411292188939));
#61490=CARTESIAN_POINT('Ctrl Pts',(15.7698930925807,0.531643658124066,3.81749054847505));
#61491=CARTESIAN_POINT('Ctrl Pts',(15.8176089286435,0.441048463954279,4.34846941266494));
#61492=CARTESIAN_POINT('Ctrl Pts',(15.8653247647064,-0.054568321067637,
4.5594434533135));
#61493=CARTESIAN_POINT('Ctrl Pts',(15.9130406007692,-0.500074177211609,
4.25667196264028));
#61494=CARTESIAN_POINT('Ctrl Pts',(15.960756436832,-0.486354221791887,3.71819465926869));
#61495=CARTESIAN_POINT('Ctrl Pts',(16.0084722728949,-0.0260077009790528,
3.4385035364232));
#61496=CARTESIAN_POINT('Ctrl Pts',(16.0561881089577,0.458222091822753,3.6744432558139));
#61497=CARTESIAN_POINT('Ctrl Pts',(16.1039039450206,0.52165948705058,4.2093467427251));
#61498=CARTESIAN_POINT('Ctrl Pts',(16.1516197810833,0.106048948556897,4.55200389457816));
#61499=CARTESIAN_POINT('Ctrl Pts',(16.1993356171462,-0.406947971169398,
4.38774737636841));
#61500=CARTESIAN_POINT('Ctrl Pts',(16.247051453209,-0.546238307271431,3.86741647617928));
#61501=CARTESIAN_POINT('Ctrl Pts',(16.2947672892719,-0.183909600849411,
3.46883906597446));
#61502=CARTESIAN_POINT('Ctrl Pts',(16.3424831253347,0.347306121845567,3.55803491444678));
#61503=CARTESIAN_POINT('Ctrl Pts',(16.3901989613975,0.559585288858183,4.05309410148958));
#61504=CARTESIAN_POINT('Ctrl Pts',(16.4379147974604,0.257988674785898,4.49939615817675));
#61505=CARTESIAN_POINT('Ctrl Pts',(16.4856306335232,-0.280522909008289,
4.4870950386126));
#61506=CARTESIAN_POINT('Ctrl Pts',(16.5333464695861,-0.561425989060384,
4.02748705016995));
#61507=CARTESIAN_POINT('Ctrl Pts',(16.5810623056489,-0.326762944709103,
3.54263728061361));
#61508=CARTESIAN_POINT('Ctrl Pts',(16.6287781417117,0.207971539662738,3.4777907336998));
#61509=CARTESIAN_POINT('Ctrl Pts',(16.6764939777746,0.551722559108811,3.89249699125187));
#61510=CARTESIAN_POINT('Ctrl Pts',(16.7242098138374,0.388818263182495,4.40592491588375));
#61511=CARTESIAN_POINT('Ctrl Pts',(16.7719256499003,-0.131143826562283,
4.54658574430191));
#61512=CARTESIAN_POINT('Ctrl Pts',(16.8196414859631,-0.53067452246778,4.18530847342493));
#61513=CARTESIAN_POINT('Ctrl Pts',(16.8673573220259,-0.442878638914007,
3.65385958006445));
#61514=CARTESIAN_POINT('Ctrl Pts',(16.9150731580888,0.0516195133182915,
3.44027676038576));
#61515=CARTESIAN_POINT('Ctrl Pts',(16.9627889941516,0.498714672202087,3.74069640409388));
#61516=CARTESIAN_POINT('Ctrl Pts',(17.0105048302145,0.487832473891125,4.27923852982128));
#61517=CARTESIAN_POINT('Ctrl Pts',(17.0582206662773,0.0289662085384809,
4.56135161697672));
#61518=CARTESIAN_POINT('Ctrl Pts',(17.1059365023401,-0.456500171817451,
4.32796687675757));
#61519=CARTESIAN_POINT('Ctrl Pts',(17.1536523384029,-0.522755420235406,
3.79340510719289));
#61520=CARTESIAN_POINT('Ctrl Pts',(17.2013681744658,-0.108956322625149,
3.44856260656401));
#61521=CARTESIAN_POINT('Ctrl Pts',(17.2490840105286,0.404899042560309,3.61011354928233));
#61522=CARTESIAN_POINT('Ctrl Pts',(17.2967998465915,0.54692938679005,4.12970321886885));
#61523=CARTESIAN_POINT('Ctrl Pts',(17.3445156826543,0.186706059540143,4.53018442682757));
#61524=CARTESIAN_POINT('Ctrl Pts',(17.3922315187172,-0.344972315027459,
4.4437891176945));
#61525=CARTESIAN_POINT('Ctrl Pts',(17.43994735478,-0.559857304624004,3.94985543320929));
#61526=CARTESIAN_POINT('Ctrl Pts',(17.4876631908428,-0.260616716872392,
3.5019702759813));
#61527=CARTESIAN_POINT('Ctrl Pts',(17.5353790269057,0.277952212086773,3.51143347749201));
#61528=CARTESIAN_POINT('Ctrl Pts',(17.5830948629685,0.561273347842132,3.96955483418404));
#61529=CARTESIAN_POINT('Ctrl Pts',(17.6308106990313,0.329168531973526,4.45563445510394));
#61530=CARTESIAN_POINT('Ctrl Pts',(17.6785265350942,-0.205216811715269,
4.52329794506467));
#61531=CARTESIAN_POINT('Ctrl Pts',(17.726242371157,-0.551148399539408,4.11040888009862));
#61532=CARTESIAN_POINT('Ctrl Pts',(17.7739582072198,-0.390951931558304,
3.59612964167903));
#61533=CARTESIAN_POINT('Ctrl Pts',(17.8216740432827,0.128261710741471,3.45273076764982));
#61534=CARTESIAN_POINT('Ctrl Pts',(17.8693898793456,0.529690650507269,3.81189765050732));
#61535=CARTESIAN_POINT('Ctrl Pts',(17.9171057154083,0.44469651557395,4.34380181523062));
#61536=CARTESIAN_POINT('Ctrl Pts',(17.9648215514712,-0.0486692721463468,
4.55998748295674));
#61537=CARTESIAN_POINT('Ctrl Pts',(18.012537387534,-0.497341318381634,4.26192802856871));
#61538=CARTESIAN_POINT('Ctrl Pts',(18.0602532235969,-0.489297179367249,
3.72333603526529));
#61539=CARTESIAN_POINT('Ctrl Pts',(18.1079690596597,-0.0319239117350811,
3.43880881780002));
#61540=CARTESIAN_POINT('Ctrl Pts',(18.1556848957225,0.454765575255941,3.66963209798526));
#61541=CARTESIAN_POINT('Ctrl Pts',(18.2034007317854,0.523836837021606,4.20383730595423));
#61542=CARTESIAN_POINT('Ctrl Pts',(18.2511165678483,0.111860671084556,4.5508555794253));
#61543=CARTESIAN_POINT('Ctrl Pts',(18.298832403911,-0.402838870307115,4.39201469830757));
#61544=CARTESIAN_POINT('Ctrl Pts',(18.346548239974,-0.547605278623001,3.87318068781251));
#61545=CARTESIAN_POINT('Ctrl Pts',(18.3942640760367,-0.189497333589109,
3.47080680306518));
#61546=CARTESIAN_POINT('Ctrl Pts',(18.4419799120997,0.342628928670919,3.55439917374707));
#61547=CARTESIAN_POINT('Ctrl Pts',(18.4896957481624,0.560113773708727,4.04719363962704));
#61548=CARTESIAN_POINT('Ctrl Pts',(18.5374115842253,0.263237521891608,4.49664946007004));
#61549=CARTESIAN_POINT('Ctrl Pts',(18.5851274202881,-0.275373796708506,
4.49002443939646));
#61550=CARTESIAN_POINT('Ctrl Pts',(18.632843256351,-0.561105120620647,4.03340243603));
#61551=CARTESIAN_POINT('Ctrl Pts',(18.6805590924138,-0.331564978554912,
3.54610646169455));
#61552=CARTESIAN_POINT('Ctrl Pts',(18.7282749284766,0.202456385100939,3.47562790763498));
#61553=CARTESIAN_POINT('Ctrl Pts',(18.7759907645394,0.550558935126376,3.8866883144956));
#61554=CARTESIAN_POINT('Ctrl Pts',(18.8237066006023,0.393074743587739,4.40180458567998));
#61555=CARTESIAN_POINT('Ctrl Pts',(18.8714224366651,-0.125376033221007,
4.54793752327491));
#61556=CARTESIAN_POINT('Ctrl Pts',(18.919138272728,-0.528692069562509,4.19089100214638));
#61557=CARTESIAN_POINT('Ctrl Pts',(18.9668541087908,-0.4465020434557,3.6585463365067));
#61558=CARTESIAN_POINT('Ctrl Pts',(19.0145699448537,0.0457176794812401,
3.43976382400136));
#61559=CARTESIAN_POINT('Ctrl Pts',(19.0622857809165,0.495954153879041,3.73545481224116));
#61560=CARTESIAN_POINT('Ctrl Pts',(19.1100016169793,0.490748297561716,4.27408171698104));
#61561=CARTESIAN_POINT('Ctrl Pts',(19.1577174530421,0.0348807284082936,
4.5610151636709));
#61562=CARTESIAN_POINT('Ctrl Pts',(19.205433289105,-0.453018350253257,4.33275975334162));
#61563=CARTESIAN_POINT('Ctrl Pts',(19.2531491251678,-0.524903707479367,
3.79892594114836));
#61564=CARTESIAN_POINT('Ctrl Pts',(19.3008649612307,-0.11476191309534,3.44974153150476));
#61565=CARTESIAN_POINT('Ctrl Pts',(19.3485807972935,0.400767511262006,3.60586793956989));
#61566=CARTESIAN_POINT('Ctrl Pts',(19.3962966333564,0.548265964675035,4.12393188459875));
#61567=CARTESIAN_POINT('Ctrl Pts',(19.4440124694192,0.192283344213529,4.52818727047755));
#61568=CARTESIAN_POINT('Ctrl Pts',(19.491728305482,-0.340276025447905,4.44740016355363));
#61569=CARTESIAN_POINT('Ctrl Pts',(19.5394441415448,-0.560354693525076,
3.95575859308266));
#61570=CARTESIAN_POINT('Ctrl Pts',(19.5871599776077,-0.265851008504119,
3.50474460473346));
#61571=CARTESIAN_POINT('Ctrl Pts',(19.6348758136705,0.272787718306182,3.5085312334714));
#61572=CARTESIAN_POINT('Ctrl Pts',(19.6825916497334,0.560921342594646,3.96364125479661));
#61573=CARTESIAN_POINT('Ctrl Pts',(19.7303074857962,0.33395216026474,4.45213995410186));
#61574=CARTESIAN_POINT('Ctrl Pts',(19.7780233218591,-0.199690227635008,
4.52543179776919));
#61575=CARTESIAN_POINT('Ctrl Pts',(19.8257391579219,-0.549954387748789,
4.11621111891367));
#61576=CARTESIAN_POINT('Ctrl Pts',(19.8734549939848,-0.395186252277308,
3.60027277035845));
#61577=CARTESIAN_POINT('Ctrl Pts',(19.9211708300475,0.122486141425193,3.45140859770427));
#61578=CARTESIAN_POINT('Ctrl Pts',(19.9688866661104,0.527680190865048,3.80632716374734));
#61579=CARTESIAN_POINT('Ctrl Pts',(20.0166025021732,0.448292560087992,4.33909316421112));
#61580=CARTESIAN_POINT('Ctrl Pts',(20.0643183382361,-0.0427598846646947,
4.56047472290141));
#61581=CARTESIAN_POINT('Ctrl Pts',(20.1120341742989,-0.49456253103916,4.26714478353561));
#61582=CARTESIAN_POINT('Ctrl Pts',(20.1597500103618,-0.492168201513856,
3.72852743457374));
#61583=CARTESIAN_POINT('Ctrl Pts',(20.2074658464246,-0.0378697858522375,
3.43914000028616));
#61584=CARTESIAN_POINT('Ctrl Pts',(20.2551816824874,0.451321269441671,3.66492646727415));
#61585=CARTESIAN_POINT('Ctrl Pts',(20.3028975185503,0.52583741886325,4.1981749506787));
#61586=CARTESIAN_POINT('Ctrl Pts',(20.3506133546131,0.117885080656874,4.54989459844945));
#61587=CARTESIAN_POINT('Ctrl Pts',(20.398329190676,-0.399119892637424,4.39574851066478));
#61588=CARTESIAN_POINT('Ctrl Pts',(20.438092387395,-0.523197416260526,3.96600412247733));
#61589=CARTESIAN_POINT('Ctrl Pts',(20.4699029447702,-0.3725623900923,3.67462118354637));
#61590=CARTESIAN_POINT('Ctrl Pts',(20.4937608628016,-0.172533290246804,
3.53519650363565));
#61591=CARTESIAN_POINT('Ctrl Pts',(20.5176187808331,0.0720421502968434,
3.50974356844941));
#61592=CARTESIAN_POINT('Ctrl Pts',(20.5414766988645,0.297725647320748,3.60399556061657));
#61593=CARTESIAN_POINT('Ctrl Pts',(20.5653346168959,0.451286063531533,3.79517586539437));
#61594=CARTESIAN_POINT('Ctrl Pts',(20.5891925349273,0.494134760388362,4.03639109206021));
#61595=CARTESIAN_POINT('Ctrl Pts',(20.6130504529587,0.416344747430809,4.26873428690612));
#61596=CARTESIAN_POINT('Ctrl Pts',(20.6369083709901,0.23664610161733,4.43535054865035));
#61597=CARTESIAN_POINT('Ctrl Pts',(20.6607662890216,-0.000865470816140784,
4.49551919950567));
#61598=CARTESIAN_POINT('Ctrl Pts',(20.684624207053,-0.238193741375527,4.43451595913869));
#61599=CARTESIAN_POINT('Ctrl Pts',(20.7084821250844,-0.417262150572256,
4.26726382233879));
#61600=CARTESIAN_POINT('Ctrl Pts',(20.7323400431158,-0.494306543785295,
4.03465729316116));
#61601=CARTESIAN_POINT('Ctrl Pts',(20.7561979611472,-0.45047531426282,3.79357669839993));
#61602=CARTESIAN_POINT('Ctrl Pts',(20.7800558791787,-0.296492828349621,
3.60297191305088));
#61603=CARTESIAN_POINT('Ctrl Pts',(20.80391379721,-0.0700085893017688,3.50945147432983));
#61604=CARTESIAN_POINT('Ctrl Pts',(20.8277717152415,0.173594031734132,3.53588342526713));
#61605=CARTESIAN_POINT('Ctrl Pts',(20.8516296332729,0.374748514455718,3.6758045671588));
#61606=CARTESIAN_POINT('Ctrl Pts',(20.8754875513043,0.484266602122282,3.89500029884494));
#61607=CARTESIAN_POINT('Ctrl Pts',(20.8993454693358,0.475368407265908,4.13987133054223));
#61608=CARTESIAN_POINT('Ctrl Pts',(20.9232033873671,0.350229638882089,4.35054000504804));
#61609=CARTESIAN_POINT('Ctrl Pts',(20.9470613053986,0.139450209771325,4.47549210343221));
#61610=CARTESIAN_POINT('Ctrl Pts',(20.97091922343,-0.105428607968738,4.48417342845956));
#61611=CARTESIAN_POINT('Ctrl Pts',(20.9947771414615,-0.324527251938122,
4.37446116262749));
#61612=CARTESIAN_POINT('Ctrl Pts',(21.0186350594928,-0.464270146732381,
4.17318294187641));
#61613=CARTESIAN_POINT('Ctrl Pts',(21.0424929775243,-0.490486342136868,
3.92955677471355));
#61614=CARTESIAN_POINT('Ctrl Pts',(21.0663508955557,-0.396765267394252,
3.7031558948169));
#61615=CARTESIAN_POINT('Ctrl Pts',(21.0902088135871,-0.206024276530194,
3.54934148458869));
#61616=CARTESIAN_POINT('Ctrl Pts',(21.1140667316185,0.0350952616297792,
3.50572535702762));
#61617=CARTESIAN_POINT('Ctrl Pts',(21.1379246496499,0.267633052506714,3.58297284346672));
#61618=CARTESIAN_POINT('Ctrl Pts',(21.1617825676814,0.434727271782411,3.76219482925797));
#61619=CARTESIAN_POINT('Ctrl Pts',(21.1856404857128,0.495518831419392,3.99956665698474));
#61620=CARTESIAN_POINT('Ctrl Pts',(21.2094984037442,0.43514253908843,4.23704444887943));
#61621=CARTESIAN_POINT('Ctrl Pts',(21.2333563217756,0.268362042918248,4.41655841606373));
#61622=CARTESIAN_POINT('Ctrl Pts',(21.257214239807,0.0359597172125542,4.49421250369607));
#61623=CARTESIAN_POINT('Ctrl Pts',(21.2810721578384,-0.205235738871087,
4.45101817209691));
#61624=CARTESIAN_POINT('Ctrl Pts',(21.3049300758699,-0.396245466293343,
4.29753761193144));
#61625=CARTESIAN_POINT('Ctrl Pts',(21.3287879939013,-0.490362383696085,
4.07130100088706));
#61626=CARTESIAN_POINT('Ctrl Pts',(21.3526459119327,-0.464572341082516,
3.82762935292545));
#61627=CARTESIAN_POINT('Ctrl Pts',(21.3765038299641,-0.325181706377507,
3.62610702345576));
#61628=CARTESIAN_POINT('Ctrl Pts',(21.4003617479955,-0.106275286691508,
3.51601171139131));
#61629=CARTESIAN_POINT('Ctrl Pts',(21.424219666027,0.138618335471326,3.52426471946798));
#61630=CARTESIAN_POINT('Ctrl Pts',(21.4480775840584,0.349615998723735,3.64884796240357));
#61631=CARTESIAN_POINT('Ctrl Pts',(21.4719355020898,0.475123026939619,3.85929744372095));
#61632=CARTESIAN_POINT('Ctrl Pts',(21.4957934201212,0.484449532977353,4.10415253270923));
#61633=CARTESIAN_POINT('Ctrl Pts',(21.5196513381527,0.375314932061802,4.32353949039209));
#61634=CARTESIAN_POINT('Ctrl Pts',(21.543509256184,0.174405606883644,4.4638122296353));
#61635=CARTESIAN_POINT('Ctrl Pts',(21.5673671742155,-0.069150639890911,
4.49067024474121));
#61636=CARTESIAN_POINT('Ctrl Pts',(21.5912250922469,-0.29579767158652,4.39754601941878));
#61637=CARTESIAN_POINT('Ctrl Pts',(21.6150830102783,-0.450114115212426,
4.20721096341231));
#61638=CARTESIAN_POINT('Ctrl Pts',(21.6389409283097,-0.494365396806572,
3.96620718253823));
#61639=CARTESIAN_POINT('Ctrl Pts',(21.6627988463412,-0.417730872638478,
3.73346666603139));
#61640=CARTESIAN_POINT('Ctrl Pts',(21.6866567643726,-0.238949771349764,
3.56590080990214));
#61641=CARTESIAN_POINT('Ctrl Pts',(21.710514682404,-0.00173894210493873,
3.50448403037633));
#61642=CARTESIAN_POINT('Ctrl Pts',(21.7343726004354,0.235897105852373,3.56423440300754));
#61643=CARTESIAN_POINT('Ctrl Pts',(21.7582305184669,0.415849885720624,3.73054133411992));
#61644=CARTESIAN_POINT('Ctrl Pts',(21.7820884364982,0.49411604100673,3.96273824894669));
#61645=CARTESIAN_POINT('Ctrl Pts',(21.8059463545297,0.451557364815975,4.20404667689569));
#61646=CARTESIAN_POINT('Ctrl Pts',(21.8298042725611,0.29858061275206,4.39546013422383));
#61647=CARTESIAN_POINT('Ctrl Pts',(21.8536621905925,0.0725927676976751,
4.49017281661646));
#61648=CARTESIAN_POINT('Ctrl Pts',(21.8775201086239,-0.171145986446082,
4.46502489330693));
#61649=CARTESIAN_POINT('Ctrl Pts',(21.9013780266554,-0.373034884980705,
4.32616571656009));
#61650=CARTESIAN_POINT('Ctrl Pts',(21.9252359446868,-0.483706592871294,
4.10755013753858));
#61651=CARTESIAN_POINT('Ctrl Pts',(21.9490938627182,-0.476098862901817,
3.86263562028194));
#61652=CARTESIAN_POINT('Ctrl Pts',(21.9729517807496,-0.352071992280181,
3.65131043559696));
#61653=CARTESIAN_POINT('Ctrl Pts',(21.996809698781,-0.141953929297546,3.52524934752154));
#61654=CARTESIAN_POINT('Ctrl Pts',(22.0206676168125,0.102875736145779,3.51527772592526));
#61655=CARTESIAN_POINT('Ctrl Pts',(22.0445255348438,0.322549481822576,3.62383390390986));
#61656=CARTESIAN_POINT('Ctrl Pts',(22.0683834528753,0.46335109312246,3.82437293894729));
#61657=CARTESIAN_POINT('Ctrl Pts',(22.0922413709067,0.490850740723195,4.06785757439707));
#61658=CARTESIAN_POINT('Ctrl Pts',(22.1160992889381,0.398324011712033,4.29474918450382));
#61659=CARTESIAN_POINT('Ctrl Pts',(22.1399572069695,0.208396211707814,4.44956659019228));
#61660=CARTESIAN_POINT('Ctrl Pts',(22.163815125001,-0.0324901386554863,
4.49445271863166));
#61661=CARTESIAN_POINT('Ctrl Pts',(22.1876730430324,-0.265431765108271,
4.41843168874211));
#61662=CARTESIAN_POINT('Ctrl Pts',(22.2115309610638,-0.433468094767725,
4.24009271310828));
#61663=CARTESIAN_POINT('Ctrl Pts',(22.2353888790952,-0.495509667838209,
4.00304452911861));
#61664=CARTESIAN_POINT('Ctrl Pts',(22.2592467971266,-0.436385629680506,
3.76525187484075));
#61665=CARTESIAN_POINT('Ctrl Pts',(22.2831047151581,-0.270553418215538,
3.58486153155103));
#61666=CARTESIAN_POINT('Ctrl Pts',(22.3069626331895,-0.0385635261649252,
3.50598385198694));
#61667=CARTESIAN_POINT('Ctrl Pts',(22.3308205512209,0.202856198284482,3.54790657725669));
#61668=CARTESIAN_POINT('Ctrl Pts',(22.3546784692523,0.394672056935096,3.70037845932536));
#61669=CARTESIAN_POINT('Ctrl Pts',(22.3785363872837,0.489979846308564,3.9261159693126));
#61670=CARTESIAN_POINT('Ctrl Pts',(22.4023943053151,0.465474217808745,4.1699201379362));
#61671=CARTESIAN_POINT('Ctrl Pts',(22.4262522233466,0.327147461276091,4.37217420322137));
#61672=CARTESIAN_POINT('Ctrl Pts',(22.450110141378,0.108824243893236,4.4834215400391));
#61673=CARTESIAN_POINT('Ctrl Pts',(22.4739680594094,-0.136109474402841,
4.47645913832327));
#61674=CARTESIAN_POINT('Ctrl Pts',(22.4978259774408,-0.347760701725541,
4.3529895060813));
#61675=CARTESIAN_POINT('Ctrl Pts',(22.5216838954723,-0.474374996640319,
4.1432043106148));
#61676=CARTESIAN_POINT('Ctrl Pts',(22.5455418135036,-0.484991622785221,
3.89840178635216));
#61677=CARTESIAN_POINT('Ctrl Pts',(22.5693997315351,-0.377014700254462,
3.67844274379546));
#61678=CARTESIAN_POINT('Ctrl Pts',(22.5932576495665,-0.176847198578467,
3.53711330196678));
#61679=CARTESIAN_POINT('Ctrl Pts',(22.6171155675979,0.0665638539184235,
3.50897209184919));
#61680=CARTESIAN_POINT('Ctrl Pts',(22.6409734856293,0.293698998435555,3.60090091054846));
#61681=CARTESIAN_POINT('Ctrl Pts',(22.6648314036608,0.449015288492166,3.79041970485759));
#61682=CARTESIAN_POINT('Ctrl Pts',(22.6886893216922,0.494537845944295,4.03118776656693));
#61683=CARTESIAN_POINT('Ctrl Pts',(22.7125472397236,0.419127261608858,4.26432734830583));
#61684=CARTESIAN_POINT('Ctrl Pts',(22.736405157755,0.241238408088568,4.43283588997321));
#61685=CARTESIAN_POINT('Ctrl Pts',(22.7602630757865,0.00434171083240793,
4.49549632518638));
#61686=CARTESIAN_POINT('Ctrl Pts',(22.7841209938178,-0.233581370990537,
4.43700954435219));
#61687=CARTESIAN_POINT('Ctrl Pts',(22.8079789118493,-0.414457183229959,
4.27163232278894));
#61688=CARTESIAN_POINT('Ctrl Pts',(22.8238841905369,-0.46737397936094,4.11714349286348));
#61689=CARTESIAN_POINT('Ctrl Pts',(22.8318368298807,-0.473742730682552,
4.03823705100924));
#61690=CARTESIAN_POINT('Ctrl Pts',(4.,-0.219892372743211,3.64701365460636));
#61691=CARTESIAN_POINT('Ctrl Pts',(4.00795263934381,-0.161099076858729,
3.61038844940468));
#61692=CARTESIAN_POINT('Ctrl Pts',(4.02385791803142,-0.0249198690254346,
3.56711791692558));
#61693=CARTESIAN_POINT('Ctrl Pts',(4.04771583606284,0.185569069288609,3.60813812632505));
#61694=CARTESIAN_POINT('Ctrl Pts',(4.07157375409426,0.350624105231944,3.74494568050885));
#61695=CARTESIAN_POINT('Ctrl Pts',(4.09543167212568,0.429971014252744,3.94413788601839));
#61696=CARTESIAN_POINT('Ctrl Pts',(4.1192895901571,0.40416308778273,4.15698104289539));
#61697=CARTESIAN_POINT('Ctrl Pts',(4.14314750818851,0.279534313346206,4.3314427366163));
#61698=CARTESIAN_POINT('Ctrl Pts',(4.16700542621994,0.0865475313004802,
4.42485517705098));
#61699=CARTESIAN_POINT('Ctrl Pts',(4.19086334425134,-0.127600227202394,
4.41438026490915));
#61700=CARTESIAN_POINT('Ctrl Pts',(4.21472126228278,-0.310547447266788,
4.30257739619942));
#61701=CARTESIAN_POINT('Ctrl Pts',(4.23857918031418,-0.417556725585918,
4.11678647978038));
#61702=CARTESIAN_POINT('Ctrl Pts',(4.26243709834561,-0.422462345057068,
3.90243789311793));
#61703=CARTESIAN_POINT('Ctrl Pts',(4.28629501637703,-0.324064236326554,
3.71194600226016));
#61704=CARTESIAN_POINT('Ctrl Pts',(4.31015293440845,-0.146423688323203,
3.59189110566319));
#61705=CARTESIAN_POINT('Ctrl Pts',(4.33401085243986,0.0670214896752265,
3.5716299793216));
#61706=CARTESIAN_POINT('Ctrl Pts',(4.35786877047129,0.264078061498623,3.65611697628114));
#61707=CARTESIAN_POINT('Ctrl Pts',(4.38172668850271,0.396560367883193,3.82469274783887));
#61708=CARTESIAN_POINT('Ctrl Pts',(4.40558460653412,0.432072854850341,4.03613591352675));
#61709=CARTESIAN_POINT('Ctrl Pts',(4.42944252456555,0.361931763288092,4.23874286631049));
#61710=CARTESIAN_POINT('Ctrl Pts',(4.45330044259696,0.203288494707987,4.382970683851));
#61711=CARTESIAN_POINT('Ctrl Pts',(4.47715836062838,-0.00506434719902249,
4.43355173791626));
#61712=CARTESIAN_POINT('Ctrl Pts',(4.5010162786598,-0.212178818846594,4.37811758201071));
#61713=CARTESIAN_POINT('Ctrl Pts',(4.52487419669122,-0.367409789343613,
4.23022337776645));
#61714=CARTESIAN_POINT('Ctrl Pts',(4.54873211472264,-0.432799058467291,
4.02603328640456));
#61715=CARTESIAN_POINT('Ctrl Pts',(4.57259003275406,-0.392357168499796,
3.8154773474345));
#61716=CARTESIAN_POINT('Ctrl Pts',(4.59644795078547,-0.255973263285106,
3.65004222328625));
#61717=CARTESIAN_POINT('Ctrl Pts',(4.6203058688169,-0.0569969226013119,
3.57018130821703));
#61718=CARTESIAN_POINT('Ctrl Pts',(4.64416378684831,0.155916718210686,3.59542277130738));
#61719=CARTESIAN_POINT('Ctrl Pts',(4.66802170487973,0.330704474340828,3.71959438727947));
#61720=CARTESIAN_POINT('Ctrl Pts',(4.69187962291115,0.424625978282027,3.91233281365517));
#61721=CARTESIAN_POINT('Ctrl Pts',(4.71573754094257,0.41471486395576,4.1265082550995));
#61722=CARTESIAN_POINT('Ctrl Pts',(4.73959545897399,0.303394668785218,4.30974898215573));
#61723=CARTESIAN_POINT('Ctrl Pts',(4.76345337700541,0.117886212792376,4.41724764568232));
#61724=CARTESIAN_POINT('Ctrl Pts',(4.78731129503683,-0.0964486333844469,
4.42271789424177));
#61725=CARTESIAN_POINT('Ctrl Pts',(4.81116921306824,-0.287199161490599,
4.32482210305491));
#61726=CARTESIAN_POINT('Ctrl Pts',(4.83502713109967,-0.407721671464292,
4.14749845969467));
#61727=CARTESIAN_POINT('Ctrl Pts',(4.85888504913109,-0.42854512664958,3.93410742516172));
#61728=CARTESIAN_POINT('Ctrl Pts',(4.8827429671625,-0.344577625034195,3.73682892005441));
#61729=CARTESIAN_POINT('Ctrl Pts',(4.90660088519393,-0.176351507991885,
3.60390291263011));
#61730=CARTESIAN_POINT('Ctrl Pts',(4.93045880322534,0.0349973564730633,
3.56783343253575));
#61731=CARTESIAN_POINT('Ctrl Pts',(4.95431672125677,0.237788413971502,3.63744045016736));
#61732=CARTESIAN_POINT('Ctrl Pts',(4.97817463928818,0.382433727027559,3.79570315365689));
#61733=CARTESIAN_POINT('Ctrl Pts',(5.0020325573196,0.433563576539811,4.00392200101168));
#61734=CARTESIAN_POINT('Ctrl Pts',(5.02589047535102,0.378675321553375,4.21118181228595));
#61735=CARTESIAN_POINT('Ctrl Pts',(5.04974839338244,0.231190635538481,4.36680191797922));
#61736=CARTESIAN_POINT('Ctrl Pts',(5.07360631141386,0.0271735416279573,
4.43272896324296));
#61737=CARTESIAN_POINT('Ctrl Pts',(5.09746422944527,-0.183488223403015,
4.39284198969348));
#61738=CARTESIAN_POINT('Ctrl Pts',(5.1213221474767,-0.349282119693095,4.256894448863));
#61739=CARTESIAN_POINT('Ctrl Pts',(5.1451800655081,-0.4296670234643,4.05812921762123));
#61740=CARTESIAN_POINT('Ctrl Pts',(5.16903798353954,-0.404986636103755,
3.84514980926298));
#61741=CARTESIAN_POINT('Ctrl Pts',(5.19289590157095,-0.281275984601366,
3.67003549057442));
#61742=CARTESIAN_POINT('Ctrl Pts',(5.21675381960238,-0.0887856930599551,
3.5756064824932));
#61743=CARTESIAN_POINT('Ctrl Pts',(5.24061173763379,0.125415118908336,3.58495324968971));
#61744=CARTESIAN_POINT('Ctrl Pts',(5.26446965566521,0.308948518064291,3.69579025298356));
#61745=CARTESIAN_POINT('Ctrl Pts',(5.28832757369662,0.416935588964862,3.88101482593007));
#61746=CARTESIAN_POINT('Ctrl Pts',(5.31218549172805,0.422970551266107,4.09533451502773));
#61747=CARTESIAN_POINT('Ctrl Pts',(5.33604340975946,0.325577692296299,4.28634231834109));
#61748=CARTESIAN_POINT('Ctrl Pts',(5.35990132779089,0.148572219001774,4.40733162501188));
#61749=CARTESIAN_POINT('Ctrl Pts',(5.3837592458223,-0.0647632088646815,
4.42871725387658));
#61750=CARTESIAN_POINT('Ctrl Pts',(5.40761716385372,-0.26226226804932,4.34526983614494));
#61751=CARTESIAN_POINT('Ctrl Pts',(5.43147508188515,-0.395631058815178,
4.17739453851434));
#61752=CARTESIAN_POINT('Ctrl Pts',(5.45533299991656,-0.432257278927009,
3.96614144408682));
#61753=CARTESIAN_POINT('Ctrl Pts',(5.47919091794798,-0.363184819889405,
3.76316768886851));
#61754=CARTESIAN_POINT('Ctrl Pts',(5.5030488359794,-0.205303779432806,3.61810588490468));
#61755=CARTESIAN_POINT('Ctrl Pts',(5.52690675401082,0.00277962745745752,
3.56642759466814));
#61756=CARTESIAN_POINT('Ctrl Pts',(5.55076467204224,0.210183339719457,3.62076956781107));
#61757=CARTESIAN_POINT('Ctrl Pts',(5.57462259007365,0.36619150013966,3.76784371165257));
#61758=CARTESIAN_POINT('Ctrl Pts',(5.59848050810508,0.432655863921731,3.97168639180759));
#61759=CARTESIAN_POINT('Ctrl Pts',(5.62233842613649,0.393324083661671,4.18245252040861));
#61760=CARTESIAN_POINT('Ctrl Pts',(5.64619634416792,0.257813851021257,4.34860403787086));
#61761=CARTESIAN_POINT('Ctrl Pts',(5.67005426219933,0.0592611090830247,
4.42951237227525));
#61762=CARTESIAN_POINT('Ctrl Pts',(5.69391218023075,-0.153782588238227,
4.40539323200473));
#61763=CARTESIAN_POINT('Ctrl Pts',(5.71777009826218,-0.329222253834466,
4.28214440376531));
#61764=CARTESIAN_POINT('Ctrl Pts',(5.74162801629359,-0.424158110434281,
4.08990358344764));
#61765=CARTESIAN_POINT('Ctrl Pts',(5.76548593432501,-0.415375755386326,
3.8756788878607));
#61766=CARTESIAN_POINT('Ctrl Pts',(5.78934385235642,-0.305022713182347,
3.69185409099321));
#61767=CARTESIAN_POINT('Ctrl Pts',(5.81320177038785,-0.120083309624962,
3.58337936191985));
#61768=CARTESIAN_POINT('Ctrl Pts',(5.83705968841926,0.0942197354074567,
3.57677972866706));
#61769=CARTESIAN_POINT('Ctrl Pts',(5.86091760645069,0.285483486244351,3.673668977605));
#61770=CARTESIAN_POINT('Ctrl Pts',(5.8847755244821,0.406938752801468,3.85035505520226));
#61771=CARTESIAN_POINT('Ctrl Pts',(5.90863344251353,0.428886400972996,4.06363338935351));
#61772=CARTESIAN_POINT('Ctrl Pts',(5.93249136054494,0.345959657594393,4.261351642888));
#61773=CARTESIAN_POINT('Ctrl Pts',(5.95634927857636,0.178436323746589,4.39516226965834));
#61774=CARTESIAN_POINT('Ctrl Pts',(5.98020719660778,-0.0327194942966983,
4.4323450160316));
#61775=CARTESIAN_POINT('Ctrl Pts',(6.0040651146392,-0.23587461323539,4.36380751861078));
#61776=CARTESIAN_POINT('Ctrl Pts',(6.02792303267061,-0.381351759249696,
4.20630938167977));
#61777=CARTESIAN_POINT('Ctrl Pts',(6.05178095070204,-0.433578399193506,
3.9983625870902));
#61778=CARTESIAN_POINT('Ctrl Pts',(6.07563886873346,-0.379782579589031,
3.79081692866841));
#61779=CARTESIAN_POINT('Ctrl Pts',(6.09949678676487,-0.233120953551068,
3.63442082419035));
#61780=CARTESIAN_POINT('Ctrl Pts',(6.12335470479629,-0.0294522997972467,
3.5674214393556));
#61781=CARTESIAN_POINT('Ctrl Pts',(6.14721262282771,0.181413325723775,3.60619428643423));
#61782=CARTESIAN_POINT('Ctrl Pts',(6.17107054085913,0.347927737305898,3.74127281623538));
#61783=CARTESIAN_POINT('Ctrl Pts',(6.19492845889055,0.429346806292137,3.93959933010928));
#61784=CARTESIAN_POINT('Ctrl Pts',(6.21878637692197,0.405811992579865,4.15272917617017));
#61785=CARTESIAN_POINT('Ctrl Pts',(6.24264429495339,0.282982581651336,4.32844890303245));
#61786=CARTESIAN_POINT('Ctrl Pts',(6.26650221298481,0.0910742457207041,
4.42397415233781));
#61787=CARTESIAN_POINT('Ctrl Pts',(6.29036013101623,-0.123327005978964,
4.41559921078967));
#61788=CARTESIAN_POINT('Ctrl Pts',(6.31421804904765,-0.307151379675736,
4.3060270879454));
#61789=CARTESIAN_POINT('Ctrl Pts',(6.33807596707907,-0.416657206472865,
4.12081787696614));
#61790=CARTESIAN_POINT('Ctrl Pts',(6.36193388511048,-0.422829889105799,
3.9075587958503));
#61791=CARTESIAN_POINT('Ctrl Pts',(6.39374444248571,-0.296437506874183,
3.64987069373525));
#61792=CARTESIAN_POINT('Ctrl Pts',(6.43350763920474,0.0703302468340302,
3.51324810367198));
#61793=CARTESIAN_POINT('Ctrl Pts',(6.48122347526758,0.448014600657906,3.7964368525222));
#61794=CARTESIAN_POINT('Ctrl Pts',(6.52893931133042,0.413240052911115,4.26646358767058));
#61795=CARTESIAN_POINT('Ctrl Pts',(6.57665514739325,-0.000480251589724132,
4.49184654025612));
#61796=CARTESIAN_POINT('Ctrl Pts',(6.62437098345609,-0.41404349770976,4.26553045144514));
#61797=CARTESIAN_POINT('Ctrl Pts',(6.67208681951894,-0.447234019333667,
3.79538894860702));
#61798=CARTESIAN_POINT('Ctrl Pts',(6.71980265558177,-0.0698021891909718,
3.51313682319347));
#61799=CARTESIAN_POINT('Ctrl Pts',(6.76751849164461,0.371772181936036,3.67798293440124));
#61800=CARTESIAN_POINT('Ctrl Pts',(6.81523432770745,0.471920133146607,4.13853999974893));
#61801=CARTESIAN_POINT('Ctrl Pts',(6.86295016377028,0.138708377331583,4.4718748549198));
#61802=CARTESIAN_POINT('Ctrl Pts',(6.91066599983312,-0.32188767172048,4.37187913281409));
#61803=CARTESIAN_POINT('Ctrl Pts',(6.95838183589596,-0.486886005735063,
3.93038141845316));
#61804=CARTESIAN_POINT('Ctrl Pts',(7.0060976719588,-0.204771183672361,3.55281534000283));
#61805=CARTESIAN_POINT('Ctrl Pts',(7.05381350802163,0.265389096458903,3.58590591031157));
#61806=CARTESIAN_POINT('Ctrl Pts',(7.10152934408448,0.491837993618785,3.99926540470374));
#61807=CARTESIAN_POINT('Ctrl Pts',(7.14924518014731,0.266624753986561,4.41329951581085));
#61808=CARTESIAN_POINT('Ctrl Pts',(7.19696101621015,-0.203434237821079,
4.44779430805676));
#61809=CARTESIAN_POINT('Ctrl Pts',(7.24467685227299,-0.486676365692783,
4.07107270446015));
#61810=CARTESIAN_POINT('Ctrl Pts',(7.29239268833582,-0.322996137187983,
3.62908393881966));
#61811=CARTESIAN_POINT('Ctrl Pts',(7.34010852439867,0.137296434535941,3.52771310152703));
#61812=CARTESIAN_POINT('Ctrl Pts',(7.3878243604615,0.471507566988788,3.86005058906394));
#61813=CARTESIAN_POINT('Ctrl Pts',(7.43554019652434,0.372726051350611,4.32090577464778));
#61814=CARTESIAN_POINT('Ctrl Pts',(7.48325603258718,-0.0683355354161961,
4.48706824929225));
#61815=CARTESIAN_POINT('Ctrl Pts',(7.53097186865002,-0.44664354691983,4.20594845626764));
#61816=CARTESIAN_POINT('Ctrl Pts',(7.57868770471286,-0.414791917646955,
3.73570302684109));
#61817=CARTESIAN_POINT('Ctrl Pts',(7.62640354077569,-0.00203048755240202,
3.50816557464413));
#61818=CARTESIAN_POINT('Ctrl Pts',(7.67411937683853,0.412595570264971,3.73228724307244));
#61819=CARTESIAN_POINT('Ctrl Pts',(7.72183521290137,0.448328767436039,4.20225365549051));
#61820=CARTESIAN_POINT('Ctrl Pts',(7.7695510489642,0.0723547589785895,4.48648742399228));
#61821=CARTESIAN_POINT('Ctrl Pts',(7.81726688502705,-0.370063737934377,
4.32397230547438));
#61822=CARTESIAN_POINT('Ctrl Pts',(7.86498272108989,-0.472647010158531,
3.86394843388276));
#61823=CARTESIAN_POINT('Ctrl Pts',(7.91269855715272,-0.141191260335066,
3.52886280888004));
#61824=CARTESIAN_POINT('Ctrl Pts',(7.96041439321556,0.31992259635559,3.62642971585976));
#61825=CARTESIAN_POINT('Ctrl Pts',(8.0081302292784,0.48724661017382,4.0670519628834));
#61826=CARTESIAN_POINT('Ctrl Pts',(8.05584606534124,0.207124564615173,4.44609936066402));
#61827=CARTESIAN_POINT('Ctrl Pts',(8.10356190140407,-0.263203155649882,
4.41548685142597));
#61828=CARTESIAN_POINT('Ctrl Pts',(8.15127773746691,-0.491827368180951,
4.00332637343646));
#61829=CARTESIAN_POINT('Ctrl Pts',(8.19899357352975,-0.268798940774433,
3.58811123553743));
#61830=CARTESIAN_POINT('Ctrl Pts',(8.24670940959259,0.201071689948468,3.55113988776764));
#61831=CARTESIAN_POINT('Ctrl Pts',(8.29442524565542,0.486295093906121,3.92636368766143));
#61832=CARTESIAN_POINT('Ctrl Pts',(8.34214108171827,0.324946230517931,4.36920884621601));
#61833=CARTESIAN_POINT('Ctrl Pts',(8.3898569177811,-0.134805756295296,4.47300384028212));
#61834=CARTESIAN_POINT('Ctrl Pts',(8.43757275384394,-0.470763542849379,
4.14243212971755));
#61835=CARTESIAN_POINT('Ctrl Pts',(8.48528858990678,-0.37441192437669,3.68106280283335));
#61836=CARTESIAN_POINT('Ctrl Pts',(8.53300442596962,0.0657679253190804,
3.51257841158684));
#61837=CARTESIAN_POINT('Ctrl Pts',(8.58072026203246,0.445552077224736,3.79170076492532));
#61838=CARTESIAN_POINT('Ctrl Pts',(8.62843609809529,0.41617890091499,4.26210751092856));
#61839=CARTESIAN_POINT('Ctrl Pts',(8.67615193415813,0.0046222361594965,
4.49181689660367));
#61840=CARTESIAN_POINT('Ctrl Pts',(8.72386777022097,-0.411179099183508,
4.26988325855195));
#61841=CARTESIAN_POINT('Ctrl Pts',(8.7715836062838,-0.449388340942622,3.80011167148426));
#61842=CARTESIAN_POINT('Ctrl Pts',(8.81929944234665,-0.0749173544856965,
3.51390061216986));
#61843=CARTESIAN_POINT('Ctrl Pts',(8.86701527840948,0.368351391347115,3.67408210030036));
#61844=CARTESIAN_POINT('Ctrl Pts',(8.91473111447233,0.473357386691186,4.13355901061654));
#61845=CARTESIAN_POINT('Ctrl Pts',(8.96244695053515,0.14367201029714,4.47038662641401));
#61846=CARTESIAN_POINT('Ctrl Pts',(9.01016278659801,-0.317949583830803,
4.37525096534692));
#61847=CARTESIAN_POINT('Ctrl Pts',(9.05787862266083,-0.487593182843731,
3.93551656882348));
#61848=CARTESIAN_POINT('Ctrl Pts',(9.10559445872368,-0.209472459465777,
3.55499829935456));
#61849=CARTESIAN_POINT('Ctrl Pts',(9.15331029478651,0.261010046587687,3.58313193881964));
#61850=CARTESIAN_POINT('Ctrl Pts',(9.20102613084934,0.491803010703882,3.99408193320625));
#61851=CARTESIAN_POINT('Ctrl Pts',(9.2487419669122,0.270965702728691,4.41046657939073));
#61852=CARTESIAN_POINT('Ctrl Pts',(9.29645780297501,-0.198703579405513,
4.44991344988054));
#61853=CARTESIAN_POINT('Ctrl Pts',(9.34417363903789,-0.485900307124067,
4.07619787653679));
#61854=CARTESIAN_POINT('Ctrl Pts',(9.39188947510068,-0.326887306273347,
3.63250862071426));
#61855=CARTESIAN_POINT('Ctrl Pts',(9.43960531116356,0.13231133773591,3.52629235307153));
#61856=CARTESIAN_POINT('Ctrl Pts',(9.48732114722637,0.470006444430667,3.85508910653225));
#61857=CARTESIAN_POINT('Ctrl Pts',(9.53503698328922,0.376087401226012,4.31695976320512));
#61858=CARTESIAN_POINT('Ctrl Pts',(9.58275281935206,-0.0631984893729827,
4.48776139227388));
#61859=CARTESIAN_POINT('Ctrl Pts',(9.63046865541489,-0.444448234747017,
4.21064422964382));
#61860=CARTESIAN_POINT('Ctrl Pts',(9.67818449147773,-0.41755432743774,3.74008922975375));
#61861=CARTESIAN_POINT('Ctrl Pts',(9.72590032754057,-0.00721385634321597,
3.50821428942208));
#61862=CARTESIAN_POINT('Ctrl Pts',(9.77361616360341,0.40975121003073,3.72795373420991));
#61863=CARTESIAN_POINT('Ctrl Pts',(9.82133199966624,0.450435435400681,4.19751745084266));
#61864=CARTESIAN_POINT('Ctrl Pts',(9.86904783572909,0.077477869602138,4.48569785316993));
#61865=CARTESIAN_POINT('Ctrl Pts',(9.91676367179192,-0.366628816002305,
4.3278544435092));
#61866=CARTESIAN_POINT('Ctrl Pts',(9.96447950785476,-0.474054618562381,
3.8689372536849));
#61867=CARTESIAN_POINT('Ctrl Pts',(10.0121953439176,-0.146148770628728,
3.53037700046135));
#61868=CARTESIAN_POINT('Ctrl Pts',(10.0599111799804,0.315967742161179,3.62307877379278));
#61869=CARTESIAN_POINT('Ctrl Pts',(10.1076270160433,0.487926215535836,4.06191310882887));
#61870=CARTESIAN_POINT('Ctrl Pts',(10.1553428521061,0.211814537474087,4.44389168337175));
#61871=CARTESIAN_POINT('Ctrl Pts',(10.203058688169,-0.258809689535701,4.4182376949229));
#61872=CARTESIAN_POINT('Ctrl Pts',(10.2507745242318,-0.491764996345908,
4.00850959581219));
#61873=CARTESIAN_POINT('Ctrl Pts',(10.2984903602946,-0.273124940234581,
3.59096700393021));
#61874=CARTESIAN_POINT('Ctrl Pts',(10.3462061963575,0.196329951061554,3.54904570612073));
#61875=CARTESIAN_POINT('Ctrl Pts',(10.3939220324203,0.485492027373267,3.92124267520431));
#61876=CARTESIAN_POINT('Ctrl Pts',(10.4416378684831,0.328819304693055,4.36576370748498));
#61877=CARTESIAN_POINT('Ctrl Pts',(10.489353704546,-0.129813245022134,4.47439829918413));
#61878=CARTESIAN_POINT('Ctrl Pts',(10.5370695406088,-0.469236294399976,
4.14738563318641));
#61879=CARTESIAN_POINT('Ctrl Pts',(10.5847853766716,-0.377752434501872,
3.68502647241413));
#61880=CARTESIAN_POINT('Ctrl Pts',(10.6325012127345,0.0606272984676223,
3.51191234851464));
#61881=CARTESIAN_POINT('Ctrl Pts',(10.6802170487973,0.443332050383407,3.78701662516801));
#61882=CARTESIAN_POINT('Ctrl Pts',(10.7279328848602,0.418918158891686,4.25770681210006));
#61883=CARTESIAN_POINT('Ctrl Pts',(10.775648720923,0.00980527620531799,
4.49174086815163));
#61884=CARTESIAN_POINT('Ctrl Pts',(10.8233645569858,-0.408311942493964,
4.27420171857372));
#61885=CARTESIAN_POINT('Ctrl Pts',(10.8710803930487,-0.451470021714238,
3.80485891169382));
#61886=CARTESIAN_POINT('Ctrl Pts',(10.9187962291115,-0.080036233235122,
3.51471716883706));
#61887=CARTESIAN_POINT('Ctrl Pts',(10.9665120651743,0.364896059739551,3.6702181168734));
#61888=CARTESIAN_POINT('Ctrl Pts',(11.0142279012372,0.47473868640782,4.1285628425314));
#61889=CARTESIAN_POINT('Ctrl Pts',(11.0619437373,0.148621472554162,4.46884633169921));
#61890=CARTESIAN_POINT('Ctrl Pts',(11.1096595733629,-0.313977126381285,
4.37858102033954));
#61891=CARTESIAN_POINT('Ctrl Pts',(11.1573754094257,-0.488245699001722,
3.94065893278431));
#61892=CARTESIAN_POINT('Ctrl Pts',(11.2050912454886,-0.214150733603143,
3.55723066033293));
#61893=CARTESIAN_POINT('Ctrl Pts',(11.2528070815514,0.256602145595791,3.58040428537983));
#61894=CARTESIAN_POINT('Ctrl Pts',(11.3005229176142,0.491713326162588,3.98889911147238));
#61895=CARTESIAN_POINT('Ctrl Pts',(11.3482387536771,0.275276593332242,4.40758805430897));
#61896=CARTESIAN_POINT('Ctrl Pts',(11.3959545897399,-0.193950870829933,
4.45198261532529));
#61897=CARTESIAN_POINT('Ctrl Pts',(11.4436704258028,-0.485070265991237,
4.08131458604192));
#61898=CARTESIAN_POINT('Ctrl Pts',(11.4913862618656,-0.330742172127369,
3.63597412121053));
#61899=CARTESIAN_POINT('Ctrl Pts',(11.5391020979284,0.127311547523522,3.52492422212962));
#61900=CARTESIAN_POINT('Ctrl Pts',(11.5868179339912,0.468453114143607,3.85014371984754));
#61901=CARTESIAN_POINT('Ctrl Pts',(11.6345337700541,0.379406977967949,4.31297854546471));
#61902=CARTESIAN_POINT('Ctrl Pts',(11.6822496061169,-0.0580544240024287,
4.48840035698771));
#61903=CARTESIAN_POINT('Ctrl Pts',(11.7299654421798,-0.44220355512924,4.21531660568344));
#61904=CARTESIAN_POINT('Ctrl Pts',(11.7776812782426,-0.420270357404582,
3.74450430230823));
#61905=CARTESIAN_POINT('Ctrl Pts',(11.8253971143054,-0.0123964237846327,
3.50831762943));
#61906=CARTESIAN_POINT('Ctrl Pts',(11.8731129503683,0.406861336540243,3.72365044295193));
#61907=CARTESIAN_POINT('Ctrl Pts',(11.9208287864311,0.452492071153857,4.1927593068956));
#61908=CARTESIAN_POINT('Ctrl Pts',(11.968544622494,0.0825923743414284,4.48485433333386));
#61909=CARTESIAN_POINT('Ctrl Pts',(12.0162604585568,-0.363153170675764,
4.33170016502878));
#61910=CARTESIAN_POINT('Ctrl Pts',(12.0639762946196,-0.475409571231627,
3.87394063131468));
#61911=CARTESIAN_POINT('Ctrl Pts',(12.1116921306825,-0.151090047408964,
3.53194335553704));
#61912=CARTESIAN_POINT('Ctrl Pts',(12.1594079667453,0.311977791768556,3.61976969834691));
#61913=CARTESIAN_POINT('Ctrl Pts',(12.2071238028081,0.488551624369653,4.05676737776005));
#61914=CARTESIAN_POINT('Ctrl Pts',(12.254839638871,0.216480982979095,4.44163470069774));
#61915=CARTESIAN_POINT('Ctrl Pts',(12.3025554749338,-0.254387476069249,
4.42094208256136));
#61916=CARTESIAN_POINT('Ctrl Pts',(12.3502713109967,-0.49164800158875,4.0136918729824));
#61917=CARTESIAN_POINT('Ctrl Pts',(12.3979871470595,-0.277420602272412,
3.59386820576715));
#61918=CARTESIAN_POINT('Ctrl Pts',(12.4457029831224,0.191566404775332,3.54700161433684));
#61919=CARTESIAN_POINT('Ctrl Pts',(12.4934188191852,0.484635034689867,3.91613041073711));
#61920=CARTESIAN_POINT('Ctrl Pts',(12.541134655248,0.332655855180181,4.362277941457));
#61921=CARTESIAN_POINT('Ctrl Pts',(12.5888504913109,-0.124806314709729,
4.47574006417428));
#61922=CARTESIAN_POINT('Ctrl Pts',(12.6365663273737,-0.4676569254097,4.15232276575852));
#61923=CARTESIAN_POINT('Ctrl Pts',(12.6842821634365,-0.381050985679211,
3.68902512775968));
#61924=CARTESIAN_POINT('Ctrl Pts',(12.7319979994994,0.0554799374235607,
3.5113004999026));
#61925=CARTESIAN_POINT('Ctrl Pts',(12.7797138355622,0.441062780321708,3.78235614259331));
#61926=CARTESIAN_POINT('Ctrl Pts',(12.8274296716251,0.421610885427219,4.2532774884218));
#61927=CARTESIAN_POINT('Ctrl Pts',(12.8751455076879,0.0149872271275763,
4.49161021945745));
#61928=CARTESIAN_POINT('Ctrl Pts',(12.9228613437507,-0.405399432451448,
4.27848972156979));
#61929=CARTESIAN_POINT('Ctrl Pts',(12.9705771798136,-0.453501555338242,
3.80962782724943));
#61930=CARTESIAN_POINT('Ctrl Pts',(13.0182930158764,-0.0851462219395619,
3.51558762841831));
#61931=CARTESIAN_POINT('Ctrl Pts',(13.0660088519392,0.361400197209248,3.66639076405307));
#61932=CARTESIAN_POINT('Ctrl Pts',(13.1137246880021,0.476067254403989,4.1235523942958));
#61933=CARTESIAN_POINT('Ctrl Pts',(13.1614405240649,0.153554426643267,4.46725395975876));
#61934=CARTESIAN_POINT('Ctrl Pts',(13.2091563601278,-0.30996979384252,4.38186902434892));
#61935=CARTESIAN_POINT('Ctrl Pts',(13.2568721961906,-0.488843983144383,
3.94580788806928));
#61936=CARTESIAN_POINT('Ctrl Pts',(13.3045880322534,-0.218805220893238,
3.55951220202843));
#61937=CARTESIAN_POINT('Ctrl Pts',(13.3523038683163,0.252165742455243,3.57772323864086));
#61938=CARTESIAN_POINT('Ctrl Pts',(13.4000197043791,0.491569024438394,3.98371752277252));
#61939=CARTESIAN_POINT('Ctrl Pts',(13.447735540442,0.279556907518101,4.40466425628032));
#61940=CARTESIAN_POINT('Ctrl Pts',(13.4954513765048,-0.189176619112,4.45400157668594));
#61941=CARTESIAN_POINT('Ctrl Pts',(13.5431672125676,-0.484186345555107,
4.08642226350871));
#61942=CARTESIAN_POINT('Ctrl Pts',(13.5908830486304,-0.334560300710407,
3.63948005597396));
#61943=CARTESIAN_POINT('Ctrl Pts',(13.6385988846933,0.122297616148583,3.52360886035071));
#61944=CARTESIAN_POINT('Ctrl Pts',(13.6863147207561,0.466847750307624,3.8452149784873));
#61945=CARTESIAN_POINT('Ctrl Pts',(13.734030556819,0.3826844119832,4.30896256355269));
#61946=CARTESIAN_POINT('Ctrl Pts',(13.7817463928818,-0.0529039102219543,
4.48898507250754));
#61947=CARTESIAN_POINT('Ctrl Pts',(13.8294622289446,-0.439909757638992,
4.21996506537626));
#61948=CARTESIAN_POINT('Ctrl Pts',(13.8771780650075,-0.422939705734467,
3.74894775411238));
#61949=CARTESIAN_POINT('Ctrl Pts',(13.9248939010703,-0.0175776142901187,
3.50847558318244));
#61950=CARTESIAN_POINT('Ctrl Pts',(13.9726097371332,0.403926270823208,3.71937784729135));
#61951=CARTESIAN_POINT('Ctrl Pts',(14.020325573196,0.454498446235019,4.18797975215946));
#61952=CARTESIAN_POINT('Ctrl Pts',(14.0680414092588,0.0876977051117048,
4.48395695817926));
#61953=CARTESIAN_POINT('Ctrl Pts',(14.1157572453217,-0.359637188018331,
4.33550904286807));
#61954=CARTESIAN_POINT('Ctrl Pts',(14.1634730813845,-0.476711717661702,
3.87895801102093));
#61955=CARTESIAN_POINT('Ctrl Pts',(14.2111889174473,-0.156014541823709,
3.53356170012368));
#61956=CARTESIAN_POINT('Ctrl Pts',(14.2589047535102,0.307953188363286,3.61650285707861));
#61957=CARTESIAN_POINT('Ctrl Pts',(14.306620589573,0.4891227672074,4.05161534124029));
#61958=CARTESIAN_POINT('Ctrl Pts',(14.3543364256359,0.2211233828038,4.4393286633369));
#61959=CARTESIAN_POINT('Ctrl Pts',(14.4020522616987,-0.249937006449114,
4.42359971395084));
#61960=CARTESIAN_POINT('Ctrl Pts',(14.4497680977616,-0.491476396904638,
4.01887262932433));
#61961=CARTESIAN_POINT('Ctrl Pts',(14.4974839338244,-0.281685449746218,
3.59681451879656));
#61962=CARTESIAN_POINT('Ctrl Pts',(14.5451997698872,0.186781580201919,3.54500783946397));
#61963=CARTESIAN_POINT('Ctrl Pts',(14.59291560595,0.483724211046603,3.91102746210588));
#61964=CARTESIAN_POINT('Ctrl Pts',(14.6406314420129,0.33645545583349,4.35875193531444));
#61965=CARTESIAN_POINT('Ctrl Pts',(14.6883472780757,-0.119785521504147,
4.47702898621568));
#61966=CARTESIAN_POINT('Ctrl Pts',(14.7360631141386,-0.466025611307368,
4.15724297904063));
#61967=CARTESIAN_POINT('Ctrl Pts',(14.7837789502014,-0.38430721152129,3.69305832471834));
#61968=CARTESIAN_POINT('Ctrl Pts',(14.8314947862642,0.0503264139313189,
3.51074293371195));
#61969=CARTESIAN_POINT('Ctrl Pts',(14.8792106223271,0.438744519099385,3.77771983486548));
#61970=CARTESIAN_POINT('Ctrl Pts',(14.9269264583899,0.42425678142631,4.24882003188202));
#61971=CARTESIAN_POINT('Ctrl Pts',(14.9746422944528,0.0201675133397715,
4.49142496503298));
#61972=CARTESIAN_POINT('Ctrl Pts',(15.0223581305156,-0.402441892563756,
4.28274679124913));
#61973=CARTESIAN_POINT('Ctrl Pts',(15.0700739665785,-0.455482716161518,
3.8144178884426));
#61974=CARTESIAN_POINT('Ctrl Pts',(15.1177898026413,-0.0902467530057116,
3.51651189422706));
#61975=CARTESIAN_POINT('Ctrl Pts',(15.1655056387041,0.357864192060027,3.66260046696357));
#61976=CARTESIAN_POINT('Ctrl Pts',(15.2132214747669,0.47734294310866,4.11852822244656));
#61977=CARTESIAN_POINT('Ctrl Pts',(15.2609373108298,0.15847032463534,4.46560968746574));
#61978=CARTESIAN_POINT('Ctrl Pts',(15.3086531468926,-0.305928031329979,
4.38511461215921));
#61979=CARTESIAN_POINT('Ctrl Pts',(15.3563689829555,-0.489387968817152,
3.95096286275689));
#61980=CARTESIAN_POINT('Ctrl Pts',(15.4040848190183,-0.223435404337718,
3.56184267101825));
#61981=CARTESIAN_POINT('Ctrl Pts',(15.4518006550811,0.24770132994065,3.57508909640066));
#61982=CARTESIAN_POINT('Ctrl Pts',(15.499516491144,0.491370121559653,3.97853774265298));
#61983=CARTESIAN_POINT('Ctrl Pts',(15.5472323272068,0.283806169849271,4.40169551006635));
#61984=CARTESIAN_POINT('Ctrl Pts',(15.5949481632697,-0.184381354552937,
4.4559701097059));
#61985=CARTESIAN_POINT('Ctrl Pts',(15.6426639993325,-0.483248643997369,
4.09152034160055));
#61986=CARTESIAN_POINT('Ctrl Pts',(15.6903798353953,-0.338341267922855,
3.64302603558196));
#61987=CARTESIAN_POINT('Ctrl Pts',(15.7380956714582,0.117270100534806,3.52234641383892));
#61988=CARTESIAN_POINT('Ctrl Pts',(15.785811507521,0.465190531238913,3.84030342991275));
#61989=CARTESIAN_POINT('Ctrl Pts',(15.8335273435838,0.385919339229949,4.30491226354526));
#61990=CARTESIAN_POINT('Ctrl Pts',(15.8812431796467,-0.0477475201261761,
4.48951547388594));
#61991=CARTESIAN_POINT('Ctrl Pts',(15.9289590157095,-0.437567097060412,
4.22458909239344));
#61992=CARTESIAN_POINT('Ctrl Pts',(15.9766748517724,-0.425562075928853,
3.75341909160864));
#61993=CARTESIAN_POINT('Ctrl Pts',(16.0243906878352,-0.0227568523576073,
3.50868813313462));
#61994=CARTESIAN_POINT('Ctrl Pts',(16.072106523898,0.400946338892803,3.71513642180785));
#61995=CARTESIAN_POINT('Ctrl Pts',(16.1198223599609,0.456454337785543,4.1831793175245));
#61996=CARTESIAN_POINT('Ctrl Pts',(16.1675381960237,0.0927932948370443,
4.4830058273823));
#61997=CARTESIAN_POINT('Ctrl Pts',(16.2152540320865,-0.356081258568678,
4.33928065395499));
#61998=CARTESIAN_POINT('Ctrl Pts',(16.2629698681494,-0.477960913216358,
3.88398883549692));
#61999=CARTESIAN_POINT('Ctrl Pts',(16.3106857042122,-0.160921706883503,
3.53523185446324));
#62000=CARTESIAN_POINT('Ctrl Pts',(16.358401540275,0.303894378979202,3.6132786128531));
#62001=CARTESIAN_POINT('Ctrl Pts',(16.4061173763379,0.489639580609251,4.04645757153336));
#62002=CARTESIAN_POINT('Ctrl Pts',(16.4538332124007,0.225741221292456,4.43697382743292));
#62003=CARTESIAN_POINT('Ctrl Pts',(16.5015490484636,-0.245458775012363,
4.42621029389423));
#62004=CARTESIAN_POINT('Ctrl Pts',(16.5492648845264,-0.4912502013546,4.02405128938415));
#62005=CARTESIAN_POINT('Ctrl Pts',(16.5969807205893,-0.285919008936969,
3.59980561575594));
#62006=CARTESIAN_POINT('Ctrl Pts',(16.6446965566521,0.181976008816936,3.54306460296116));
#62007=CARTESIAN_POINT('Ctrl Pts',(16.6924123927149,0.482759657613431,3.90593439612197));
#62008=CARTESIAN_POINT('Ctrl Pts',(16.7401282287778,0.340217684611379,4.35518608070932));
#62009=CARTESIAN_POINT('Ctrl Pts',(16.7878440648406,-0.114751423091257,
4.47826492214097));
#62010=CARTESIAN_POINT('Ctrl Pts',(16.8355599009034,-0.464342533291602,
4.16214572651883));
#62011=CARTESIAN_POINT('Ctrl Pts',(16.8832757369663,-0.387520750342007,
3.69712561530174));
#62012=CARTESIAN_POINT('Ctrl Pts',(16.9309915730291,0.0451673004198413,
3.51023971187451));
#62013=CARTESIAN_POINT('Ctrl Pts',(16.978707409092,0.436377524217892,3.7731082169636));
#62014=CARTESIAN_POINT('Ctrl Pts',(17.0264232451548,0.426855552995382,4.24433493759383));
#62015=CARTESIAN_POINT('Ctrl Pts',(17.0741390812176,0.0253455594402812,
4.49118512545541));
#62016=CARTESIAN_POINT('Ctrl Pts',(17.1218549172805,-0.399439651340385,
4.28697245475663));
#62017=CARTESIAN_POINT('Ctrl Pts',(17.1695707533433,-0.457413284126125,
3.81922856321607));
#62018=CARTESIAN_POINT('Ctrl Pts',(17.2172865894061,-0.0953372598908034,
3.51748986360026));
#62019=CARTESIAN_POINT('Ctrl Pts',(17.265002425469,0.354288437054553,3.6588476466131));
#62020=CARTESIAN_POINT('Ctrl Pts',(17.3127182615318,0.478565610824392,4.11349088504481));
#62021=CARTESIAN_POINT('Ctrl Pts',(17.3604340975947,0.163368620495752,4.46391369745815));
#62022=CARTESIAN_POINT('Ctrl Pts',(17.4081499336575,-0.301852287783465,
4.38831742326589));
#62023=CARTESIAN_POINT('Ctrl Pts',(17.4558657697204,-0.489877595596684,
3.956123284257));
#62024=CARTESIAN_POINT('Ctrl Pts',(17.5035816057832,-0.228040769637767,
3.56422180844494));
#62025=CARTESIAN_POINT('Ctrl Pts',(17.551297441846,0.243209403937772,3.57250215124727));
#62026=CARTESIAN_POINT('Ctrl Pts',(17.5990132779089,0.491116639619549,3.97336034645914));
#62027=CARTESIAN_POINT('Ctrl Pts',(17.6467291139717,0.288023908337871,4.39868214542132));
#62028=CARTESIAN_POINT('Ctrl Pts',(17.6944449500345,-0.179565609787963,
4.45788799572981));
#62029=CARTESIAN_POINT('Ctrl Pts',(17.7421607860973,-0.48225726547346,4.09660825404716));
#62030=CARTESIAN_POINT('Ctrl Pts',(17.7898766221602,-0.342084653792828,
3.64661166616396));
#62031=CARTESIAN_POINT('Ctrl Pts',(17.837592458223,0.112229559114723,3.52113702282083));
#62032=CARTESIAN_POINT('Ctrl Pts',(17.8853082942859,0.463481641013499,3.83540961967535));
#62033=CARTESIAN_POINT('Ctrl Pts',(17.9330241303487,0.389111400387848,4.30082809533052));
#62034=CARTESIAN_POINT('Ctrl Pts',(17.9807399664116,-0.0425858264624495,
4.48999150220845));
#62035=CARTESIAN_POINT('Ctrl Pts',(18.0284558024744,-0.435175833605105,
4.22918817311999));
#62036=CARTESIAN_POINT('Ctrl Pts',(18.0761716385373,-0.428137176707308,
3.75791781814212));
#62037=CARTESIAN_POINT('Ctrl Pts',(18.1238874746,-0.0279335627019553,3.5089552556775));
#62038=CARTESIAN_POINT('Ctrl Pts',(18.1716033106629,0.397921871745719,3.71092663761881));
#62039=CARTESIAN_POINT('Ctrl Pts',(18.2193191467257,0.458359528554279,4.17835853620019));
#62040=CARTESIAN_POINT('Ctrl Pts',(18.2670349827886,0.097878577523561,4.48200104659009));
#62041=CARTESIAN_POINT('Ctrl Pts',(18.3147508188514,-0.352485777302551,
4.34301457935691));
#62042=CARTESIAN_POINT('Ctrl Pts',(18.3624666549143,-0.479157019140895,
3.88903254594255));
#62043=CARTESIAN_POINT('Ctrl Pts',(18.4101824909771,-0.165810997523729,
3.5369536330429));
#62044=CARTESIAN_POINT('Ctrl Pts',(18.4578983270399,0.299801814449608,3.61009732380414));
#62045=CARTESIAN_POINT('Ctrl Pts',(18.5056141631028,0.49010200717001,4.04129464153984));
#62046=CARTESIAN_POINT('Ctrl Pts',(18.5533299991656,0.230333985517487,4.43457045454981));
#62047=CARTESIAN_POINT('Ctrl Pts',(18.6010458352284,-0.24095327917969,4.42877353242069));
#62048=CARTESIAN_POINT('Ctrl Pts',(18.6487616712913,-0.49096944006335,4.0292272779409));
#62049=CARTESIAN_POINT('Ctrl Pts',(18.6964775073541,-0.290120809601049,
3.60284116440841));
#62050=CARTESIAN_POINT('Ctrl Pts',(18.744193343417,0.177150224400508,3.54117212067402));
#62051=CARTESIAN_POINT('Ctrl Pts',(18.7919091794797,0.481741481528227,3.90085177849878));
#62052=CARTESIAN_POINT('Ctrl Pts',(18.8396250155427,0.343942123623612,4.35158077372017));
#62053=CARTESIAN_POINT('Ctrl Pts',(18.8873408516054,-0.109704578635382,
4.47944773466767));
#62054=CARTESIAN_POINT('Ctrl Pts',(18.9350566876684,-0.462607878309702,
4.16703046362027));
#62055=CARTESIAN_POINT('Ctrl Pts',(18.9827725237311,-0.39069124519864,3.70122654773242));
#62056=CARTESIAN_POINT('Ctrl Pts',(19.030488359794,0.0400031699426168,3.50979089028978));
#62057=CARTESIAN_POINT('Ctrl Pts',(19.0782041958568,0.433962058584907,3.76852180111673));
#62058=CARTESIAN_POINT('Ctrl Pts',(19.1259200319197,0.429406911488226,4.23982270375453));
#62059=CARTESIAN_POINT('Ctrl Pts',(19.1736358679825,0.0305207902517796,
4.49089072733801));
#62060=CARTESIAN_POINT('Ctrl Pts',(19.2213517040454,-0.396393042209671,
4.29116624277653));
#62061=CARTESIAN_POINT('Ctrl Pts',(19.2690675401082,-0.459293044881286,
3.82405931712685));
#62062=CARTESIAN_POINT('Ctrl Pts',(19.316783376171,-0.100417177000157,3.51852142809106));
#62063=CARTESIAN_POINT('Ctrl Pts',(19.3644992122339,0.350673329058588,3.65513271950473));
#62064=CARTESIAN_POINT('Ctrl Pts',(19.4122150482967,0.479735122332443,4.10844094226069));
#62065=CARTESIAN_POINT('Ctrl Pts',(19.4599308843596,0.168248769032157,4.46216617689766));
#62066=CARTESIAN_POINT('Ctrl Pts',(19.5076467204224,-0.297743013815871,
4.39147710422109));
#62067=CARTESIAN_POINT('Ctrl Pts',(19.5553625564852,-0.490312813065352,
3.96128857502183));
#62068=CARTESIAN_POINT('Ctrl Pts',(19.603078392548,-0.232620797759261,3.56664935826393));
#62069=CARTESIAN_POINT('Ctrl Pts',(19.6507942286109,0.238690449241969,3.56996267500769));
#62070=CARTESIAN_POINT('Ctrl Pts',(19.6985100646737,0.490808633485035,3.96818593857384));
#62071=CARTESIAN_POINT('Ctrl Pts',(19.7462259007366,0.292209604061002,4.39562444172689));
#62072=CARTESIAN_POINT('Ctrl Pts',(19.7939417367994,-0.174729824492781,
4.45975512619968));
#62073=CARTESIAN_POINT('Ctrl Pts',(19.8416575728622,-0.481212499922896,
4.10168523844358));
#62074=CARTESIAN_POINT('Ctrl Pts',(19.8893734089251,-0.345789702982467,
3.65023692191923));
#62075=CARTESIAN_POINT('Ctrl Pts',(19.9370892449879,0.107175910646637,3.51998011832295));
#62076=CARTESIAN_POINT('Ctrl Pts',(19.9848050810508,0.461722480014006,3.83053541934297));
#62077=CARTESIAN_POINT('Ctrl Pts',(20.0325209171136,0.392257955100357,4.29670800504879));
#62078=CARTESIAN_POINT('Ctrl Pts',(20.0802367531764,-0.0374150865130887,
4.49041783929577));
#62079=CARTESIAN_POINT('Ctrl Pts',(20.1279525892393,-0.432744382500041,
4.23375285658289));
#62080=CARTESIAN_POINT('Ctrl Pts',(20.1756684253021,-0.430649333670284,
3.76246031529274));
#62081=CARTESIAN_POINT('Ctrl Pts',(20.223384261365,-0.033136228617316,3.50924504180455));
#62082=CARTESIAN_POINT('Ctrl Pts',(20.2711000974278,0.394908089060633,3.70680919012016));
#62083=CARTESIAN_POINT('Ctrl Pts',(20.3188159334906,0.460110046434968,4.17340395051402));
#62084=CARTESIAN_POINT('Ctrl Pts',(20.3665317695535,0.103149962306437,4.48116018402389));
#62085=CARTESIAN_POINT('Ctrl Pts',(20.4142476056163,-0.34923165553999,4.34628168153608));
#62086=CARTESIAN_POINT('Ctrl Pts',(20.4540108023354,-0.457800032585507,
3.97025345815189));
#62087=CARTESIAN_POINT('Ctrl Pts',(20.4858213597105,-0.325993724402262,
3.71529210935379));
#62088=CARTESIAN_POINT('Ctrl Pts',(20.509679277742,-0.15096738523986,3.59329490328468));
#62089=CARTESIAN_POINT('Ctrl Pts',(20.5335371957734,0.0630371972956549,
3.57102347342756));
#62090=CARTESIAN_POINT('Ctrl Pts',(20.5573951138048,0.260511246441404,3.65349437971329));
#62091=CARTESIAN_POINT('Ctrl Pts',(20.5812530318362,0.394877283734959,3.82077798440408));
#62092=CARTESIAN_POINT('Ctrl Pts',(20.6051109498677,0.432370081305563,4.03184236506754));
#62093=CARTESIAN_POINT('Ctrl Pts',(20.6289688678991,0.364303478986858,4.23514367899931));
#62094=CARTESIAN_POINT('Ctrl Pts',(20.6528267859305,0.207066376217976,4.38093363836299));
#62095=CARTESIAN_POINT('Ctrl Pts',(20.6766847039619,-0.000757290757721993,
4.43358147160167));
#62096=CARTESIAN_POINT('Ctrl Pts',(20.7005426219933,-0.208420567790133,
4.38020336888205));
#62097=CARTESIAN_POINT('Ctrl Pts',(20.7244005400248,-0.365106210756856,
4.23385701605743));
#62098=CARTESIAN_POINT('Ctrl Pts',(20.7482584580562,-0.432520392530856,
4.03032528343114));
#62099=CARTESIAN_POINT('Ctrl Pts',(20.7721163760876,-0.394167874571092,
3.81937870627435));
#62100=CARTESIAN_POINT('Ctrl Pts',(20.795974294119,-0.259432524437891,3.65259868360638));
#62101=CARTESIAN_POINT('Ctrl Pts',(20.8198322121504,-0.0612578225112809,
3.57076788979259));
#62102=CARTESIAN_POINT('Ctrl Pts',(20.8436901301819,0.151895538690754,3.5938959627232));
#62103=CARTESIAN_POINT('Ctrl Pts',(20.8675480482132,0.327906592802717,3.71632757520176));
#62104=CARTESIAN_POINT('Ctrl Pts',(20.8914059662447,0.423735399567132,3.90812480123879));
#62105=CARTESIAN_POINT('Ctrl Pts',(20.9152638842761,0.415949440063929,4.12238802732943));
#62106=CARTESIAN_POINT('Ctrl Pts',(20.9391218023075,0.30645246920106,4.30672404095661));
#62107=CARTESIAN_POINT('Ctrl Pts',(20.962979720339,0.122019544809087,4.41605767475162));
#62108=CARTESIAN_POINT('Ctrl Pts',(20.9868376383703,-0.0922504941031022,
4.42365387220386));
#62109=CARTESIAN_POINT('Ctrl Pts',(21.0106955564018,-0.28396276796243,4.32765515869354));
#62110=CARTESIAN_POINT('Ctrl Pts',(21.0345534744332,-0.40623841344949,4.15153583326342));
#62111=CARTESIAN_POINT('Ctrl Pts',(21.0584113924646,-0.429177699343215,
3.93836186909709));
#62112=CARTESIAN_POINT('Ctrl Pts',(21.082269310496,-0.347171348131155,3.74026010679315));
#62113=CARTESIAN_POINT('Ctrl Pts',(21.1061272285274,-0.180272145040548,
3.605671823621));
#62114=CARTESIAN_POINT('Ctrl Pts',(21.1299851465589,0.0307085077608185,
3.56750752082027));
#62115=CARTESIAN_POINT('Ctrl Pts',(21.1538430645903,0.234180094072738,3.63509941005724));
#62116=CARTESIAN_POINT('Ctrl Pts',(21.1777009826217,0.380388268371489,3.79191943321731));
#62117=CARTESIAN_POINT('Ctrl Pts',(21.2015589006531,0.433581149524578,3.99962082296209));
#62118=CARTESIAN_POINT('Ctrl Pts',(21.2254168186846,0.380751629084578,4.2074149318183));
#62119=CARTESIAN_POINT('Ctrl Pts',(21.2492747367159,0.234817963878357,4.36449043997717));
#62120=CARTESIAN_POINT('Ctrl Pts',(21.2731326547474,0.0314649101850846,
4.43243810704058));
#62121=CARTESIAN_POINT('Ctrl Pts',(21.2969905727788,-0.179582171132277,
4.39464287755545));
#62122=CARTESIAN_POINT('Ctrl Pts',(21.3208484908102,-0.346716519889314,
4.26034671465164));
#62123=CARTESIAN_POINT('Ctrl Pts',(21.3447064088417,-0.429069235164158,
4.0623886883135));
#62124=CARTESIAN_POINT('Ctrl Pts',(21.368564326873,-0.406502834830527,3.8491749282489));
#62125=CARTESIAN_POINT('Ctrl Pts',(21.3924222449045,-0.284535418465691,
3.67284200661995));
#62126=CARTESIAN_POINT('Ctrl Pts',(21.4162801629359,-0.0929913416969399,
3.5765081259772));
#62127=CARTESIAN_POINT('Ctrl Pts',(21.4401380809674,0.121291651150069,3.58372954422009));
#62128=CARTESIAN_POINT('Ctrl Pts',(21.4639959989987,0.305915531372611,3.69274042788069));
#62129=CARTESIAN_POINT('Ctrl Pts',(21.4878539170302,0.415734731202803,3.87688464650718));
#62130=CARTESIAN_POINT('Ctrl Pts',(21.5117118350615,0.423895464867194,4.09113392265755));
#62131=CARTESIAN_POINT('Ctrl Pts',(21.535569753093,0.328402210690932,4.28309847227994));
#62132=CARTESIAN_POINT('Ctrl Pts',(21.5594276711244,0.152605670504114,4.40583773398234));
#62133=CARTESIAN_POINT('Ctrl Pts',(21.5832855891559,-0.0605071130159612,
4.42933861492812));
#62134=CARTESIAN_POINT('Ctrl Pts',(21.6071435071872,-0.258824259222961,
4.34785450957493));
#62135=CARTESIAN_POINT('Ctrl Pts',(21.6310014252187,-0.39385182381868,4.18131050126406));
#62136=CARTESIAN_POINT('Ctrl Pts',(21.6548593432501,-0.432571889182456,
3.97043113659525));
#62137=CARTESIAN_POINT('Ctrl Pts',(21.6787172612815,-0.365516344619441,
3.76678216446856));
#62138=CARTESIAN_POINT('Ctrl Pts',(21.702575179313,-0.209082097331647,3.62016130585559));
#62139=CARTESIAN_POINT('Ctrl Pts',(21.7264330973443,-0.00152158196427748,
3.56642135455923));
#62140=CARTESIAN_POINT('Ctrl Pts',(21.7502910153758,0.206411001640417,3.61870319251831));
#62141=CARTESIAN_POINT('Ctrl Pts',(21.7741489334072,0.363870472821225,3.76422248622317));
#62142=CARTESIAN_POINT('Ctrl Pts',(21.7980068514386,0.432353701764573,3.96739580449697));
#62143=CARTESIAN_POINT('Ctrl Pts',(21.82186476947,0.395114673548107,4.17854173669174));
#62144=CARTESIAN_POINT('Ctrl Pts',(21.8457226875014,0.261259344941517,4.3460293508861));
#62145=CARTESIAN_POINT('Ctrl Pts',(21.8695806055329,0.0635189899350569,
4.42890336313855));
#62146=CARTESIAN_POINT('Ctrl Pts',(21.8934385235643,-0.14975348833307,4.40689882001058));
#62147=CARTESIAN_POINT('Ctrl Pts',(21.9172964415957,-0.326407159500644,
4.28539643168872));
#62148=CARTESIAN_POINT('Ctrl Pts',(21.9411543596271,-0.423245389017799,
4.09410684177624));
#62149=CARTESIAN_POINT('Ctrl Pts',(21.9650122776585,-0.416588591947193,
3.87980556563057));
#62150=CARTESIAN_POINT('Ctrl Pts',(21.98887019569,-0.30806453650007,3.69489510271888));
#62151=CARTESIAN_POINT('Ctrl Pts',(22.0127281137213,-0.12421031036921,3.58459109808296));
#62152=CARTESIAN_POINT('Ctrl Pts',(22.0365860317528,0.0900167200678817,
3.57586588547707));
#62153=CARTESIAN_POINT('Ctrl Pts',(22.0604439497842,0.282232210442068,3.67085301705332));
#62154=CARTESIAN_POINT('Ctrl Pts',(22.0843018678157,0.405434237512275,3.8463255517439));
#62155=CARTESIAN_POINT('Ctrl Pts',(22.108159785847,0.429496549703537,4.05937567504088));
#62156=CARTESIAN_POINT('Ctrl Pts',(22.1320177038785,0.348535256241736,4.25790682842971));
#62157=CARTESIAN_POINT('Ctrl Pts',(22.1558756219099,0.182347598717988,4.39337273702606));
#62158=CARTESIAN_POINT('Ctrl Pts',(22.1797335399413,-0.0284290137391457,
4.43264829616218));
#62159=CARTESIAN_POINT('Ctrl Pts',(22.2035914579727,-0.232253957950086,
4.36612956178204));
#62160=CARTESIAN_POINT('Ctrl Pts',(22.2274493760041,-0.379286482964224,
4.21008217638027));
#62161=CARTESIAN_POINT('Ctrl Pts',(22.2513072940356,-0.433573131350875,
4.00266397632408));
#62162=CARTESIAN_POINT('Ctrl Pts',(22.275165212067,-0.381839338801546,3.79459436150246));
#62163=CARTESIAN_POINT('Ctrl Pts',(22.2990231300984,-0.236735426869051,
3.63675202040985));
#62164=CARTESIAN_POINT('Ctrl Pts',(22.3228810481298,-0.0337432544318164,
3.56773370504276));
#62165=CARTESIAN_POINT('Ctrl Pts',(22.3467389661613,0.177500062688638,3.60441627341574));
#62166=CARTESIAN_POINT('Ctrl Pts',(22.3705968841926,0.345339779804043,3.73782983856348));
#62167=CARTESIAN_POINT('Ctrl Pts',(22.3944548022241,0.428734513273282,3.93535114928888));
#62168=CARTESIAN_POINT('Ctrl Pts',(22.4183127202555,0.407291980919218,4.1486808655136));
#62169=CARTESIAN_POINT('Ctrl Pts',(22.4421706382869,0.286255462618544,4.32565405918856));
#62170=CARTESIAN_POINT('Ctrl Pts',(22.4660285563183,0.0952216904214238,
4.42299596654013));
#62171=CARTESIAN_POINT('Ctrl Pts',(22.4898864743497,-0.119096386717928,
4.41690383452019));
#62172=CARTESIAN_POINT('Ctrl Pts',(22.5137443923812,-0.304292138366774,
4.30886736509782));
#62173=CARTESIAN_POINT('Ctrl Pts',(22.5376023104126,-0.415080201412036,
4.12530439950267));
#62174=CARTESIAN_POINT('Ctrl Pts',(22.561460228444,-0.424369795825249,3.91110111771763));
#62175=CARTESIAN_POINT('Ctrl Pts',(22.5853181464754,-0.329889515310188,
3.71863599132299));
#62176=CARTESIAN_POINT('Ctrl Pts',(22.6091760645068,-0.154742073939436,
3.59497211022641));
#62177=CARTESIAN_POINT('Ctrl Pts',(22.6330339825383,0.0582436639512456,
3.57034842802071));
#62178=CARTESIAN_POINT('Ctrl Pts',(22.6568919005697,0.256987911016647,3.65078654733876));
#62179=CARTESIAN_POINT('Ctrl Pts',(22.6807498186011,0.39289034562191,3.81661632308649));
#62180=CARTESIAN_POINT('Ctrl Pts',(22.7046077366325,0.432722782933869,4.02728943245291));
#62181=CARTESIAN_POINT('Ctrl Pts',(22.7284656546639,0.366738191089385,4.2312875884069));
#62182=CARTESIAN_POINT('Ctrl Pts',(22.7523235726953,0.211084664509997,4.37873330099785));
#62183=CARTESIAN_POINT('Ctrl Pts',(22.7761814907268,0.00379901600965994,
4.43356145647204));
#62184=CARTESIAN_POINT('Ctrl Pts',(22.8000394087582,-0.204384723485633,
4.3823852668741));
#62185=CARTESIAN_POINT('Ctrl Pts',(22.8238973267896,-0.36265185203719,4.2376794731));
#62186=CARTESIAN_POINT('Ctrl Pts',(22.8398026054772,-0.408954280604672,
4.10250106973657));
#62187=CARTESIAN_POINT('Ctrl Pts',(22.847755244821,-0.414526965927561,4.03345758723954));
#62188=CARTESIAN_POINT('',(22.8,-0.592174260192535,4.04779597854866));
#62189=CARTESIAN_POINT('Ctrl Pts',(22.8,-0.19576256658266,4.36695865185836));
#62190=CARTESIAN_POINT('Ctrl Pts',(22.8,-0.195886593570853,4.36694806728808));
#62191=CARTESIAN_POINT('Ctrl Pts',(22.8,-0.196010613870461,4.36693742279878));
#62192=CARTESIAN_POINT('Ctrl Pts',(22.8,-0.196134627427637,4.36692671841166));
#62193=CARTESIAN_POINT('Ctrl Pts',(22.8,-0.216622178843513,4.36515830948628));
#62194=CARTESIAN_POINT('Ctrl Pts',(22.8,-0.236921239981942,4.36175743074964));
#62195=CARTESIAN_POINT('Ctrl Pts',(22.8,-0.256857422940798,4.35688458679081));
#62196=CARTESIAN_POINT('Ctrl Pts',(22.8,-0.271809560159941,4.35322995382169));
#62197=CARTESIAN_POINT('Ctrl Pts',(22.8,-0.286558947067823,4.34874691155445));
#62198=CARTESIAN_POINT('Ctrl Pts',(22.8,-0.301048271828705,4.34349077646485));
#62199=CARTESIAN_POINT('Ctrl Pts',(22.8,-0.310003423377303,4.3402422133286));
#62200=CARTESIAN_POINT('Ctrl Pts',(22.8,-0.318859482942331,4.33669811041118));
#62201=CARTESIAN_POINT('Ctrl Pts',(22.8,-0.327604744452034,4.33286912874946));
#62202=CARTESIAN_POINT('Ctrl Pts',(22.8,-0.333457186121174,4.33030672489195));
#62203=CARTESIAN_POINT('Ctrl Pts',(22.8,-0.33926207870774,4.32761569029118));
#62204=CARTESIAN_POINT('Ctrl Pts',(22.8,-0.345009487597299,4.32480202294401));
#62205=CARTESIAN_POINT('Ctrl Pts',(22.8,-0.365309066997251,4.31486428146495));
#62206=CARTESIAN_POINT('Ctrl Pts',(22.8,-0.384828901796994,4.30343044333042));
#62207=CARTESIAN_POINT('Ctrl Pts',(22.8,-0.403416958856431,4.29067119823496));
#62208=CARTESIAN_POINT('Ctrl Pts',(22.8,-0.409874425773003,4.28623865303559));
#62209=CARTESIAN_POINT('Ctrl Pts',(22.8,-0.416219739836017,4.28164578247975));
#62210=CARTESIAN_POINT('Ctrl Pts',(22.8,-0.422447327171508,4.27689854297234));
#62211=CARTESIAN_POINT('Ctrl Pts',(22.8,-0.43500295340691,4.2673274905416));
#62212=CARTESIAN_POINT('Ctrl Pts',(22.8,-0.447079966647781,4.25712966465555));
#62213=CARTESIAN_POINT('Ctrl Pts',(22.8,-0.458660056443695,4.24636133358853));
#62214=CARTESIAN_POINT('Ctrl Pts',(22.8,-0.465333929961841,4.24015529539631));
#62215=CARTESIAN_POINT('Ctrl Pts',(22.8,-0.471842796551704,4.23375955955572));
#62216=CARTESIAN_POINT('Ctrl Pts',(22.8,-0.478183280583292,4.22718326898633));
#62217=CARTESIAN_POINT('Ctrl Pts',(22.8,-0.48330469601013,4.22187138494));
#62218=CARTESIAN_POINT('Ctrl Pts',(22.8,-0.488310096860405,4.21644792156372));
#62219=CARTESIAN_POINT('Ctrl Pts',(22.8,-0.49319389770791,4.21092357737429));
#62220=CARTESIAN_POINT('Ctrl Pts',(22.8,-0.509882204568999,4.19204648678071));
#62221=CARTESIAN_POINT('Ctrl Pts',(22.8,-0.525164669297395,4.17198027236651));
#62222=CARTESIAN_POINT('Ctrl Pts',(22.8,-0.538985569877159,4.15095378743758));
#62223=CARTESIAN_POINT('Ctrl Pts',(22.8,-0.553292287721507,4.12918820238033));
#62224=CARTESIAN_POINT('Ctrl Pts',(22.8,-0.566034197593199,4.10639346234103));
#62225=CARTESIAN_POINT('Ctrl Pts',(22.8,-0.577149101532509,4.08276767497818));
#62226=CARTESIAN_POINT('Ctrl Pts',(22.8,-0.582543745751794,4.07130084468266));
#62227=CARTESIAN_POINT('Ctrl Pts',(22.8,-0.587554988912119,4.05963744408228));
#62228=CARTESIAN_POINT('Ctrl Pts',(22.8,-0.592174260192535,4.04779597854866));
#62229=CARTESIAN_POINT('Ctrl Pts',(22.8,-0.592174260192532,4.04779597854869));
#62230=CARTESIAN_POINT('Ctrl Pts',(22.7920473606562,-0.584213376873468,
4.14642833911734));
#62231=CARTESIAN_POINT('Ctrl Pts',(22.7840947213124,-0.551140611244481,
4.24298318064208));
#62232=CARTESIAN_POINT('Ctrl Pts',(22.7761420819686,-0.496922031827459,
4.32571394759471));
#62233=CARTESIAN_POINT('Ctrl Pts',(22.7681894426248,-0.442703452410443,
4.40844471454734));
#62234=CARTESIAN_POINT('Ctrl Pts',(22.760236803281,-0.367339059205388,4.47735140692785));
#62235=CARTESIAN_POINT('Ctrl Pts',(22.7522841639372,-0.280089901523161,
4.52398941366922));
#62236=CARTESIAN_POINT('Ctrl Pts',(22.7444712463773,-0.194373644734646,
4.56980802634291));
#62237=CARTESIAN_POINT('Ctrl Pts',(22.7366583288174,-0.0971865673270821,
4.59413356703531));
#62238=CARTESIAN_POINT('Ctrl Pts',(22.7288454112575,-7.11440487624268E-7,
4.59414971000239));
#62239=CARTESIAN_POINT('Origin',(27.2,0.3,2.9));
#62240=CARTESIAN_POINT('',(29.2,0.3,3.04606079858305));
#62241=CARTESIAN_POINT('',(27.2,0.3,3.04606079858305));
#62242=CARTESIAN_POINT('',(23.3,0.3,3.04606079858305));
#62243=CARTESIAN_POINT('',(29.2,0.3,3.35));
#62244=CARTESIAN_POINT('',(29.2,0.3,2.9));
#62245=CARTESIAN_POINT('',(27.2,0.3,3.35));
#62246=CARTESIAN_POINT('',(27.2,0.3,3.35));
#62247=CARTESIAN_POINT('',(27.2,0.3,2.9));
#62248=CARTESIAN_POINT('Origin',(27.2,0.,3.125));
#62249=CARTESIAN_POINT('',(27.2,-0.3,3.04606079858305));
#62250=CARTESIAN_POINT('Origin',(27.2,0.,4.));
#62251=CARTESIAN_POINT('',(27.2,-0.3,3.35));
#62252=CARTESIAN_POINT('',(27.2,0.3,3.35));
#62253=CARTESIAN_POINT('',(27.2,-0.3,3.35));
#62254=CARTESIAN_POINT('Origin',(27.2,0.3,3.35));
#62255=CARTESIAN_POINT('',(29.2,-0.3,3.35));
#62256=CARTESIAN_POINT('',(29.2,0.3,3.35));
#62257=CARTESIAN_POINT('',(27.2,-0.3,3.35));
#62258=CARTESIAN_POINT('Origin',(27.2,-0.3,3.35));
#62259=CARTESIAN_POINT('',(29.2,-0.3,3.04606079858305));
#62260=CARTESIAN_POINT('',(23.3,-0.3,3.04606079858305));
#62261=CARTESIAN_POINT('',(29.2,-0.3,3.35));
#62262=CARTESIAN_POINT('Origin',(29.2,0.,3.125));
#62263=CARTESIAN_POINT('Origin',(29.2,0.,4.));
#62264=CARTESIAN_POINT('Origin',(23.3,0.,4.));
#62265=CARTESIAN_POINT('',(29.4,-1.22464679914735E-16,5.));
#62266=CARTESIAN_POINT('Origin',(29.4,0.,4.));
#62267=CARTESIAN_POINT('',(23.3,-1.22464679914735E-16,5.));
#62268=CARTESIAN_POINT('',(23.3,-1.22464679914735E-16,5.));
#62269=CARTESIAN_POINT('Origin',(23.3,0.,4.));
#62270=CARTESIAN_POINT('Origin',(29.4,0.,4.));
#62271=CARTESIAN_POINT('Origin',(22.8,0.,4.));
#62272=CARTESIAN_POINT('',(22.8,-1.65327317884893E-16,5.35));
#62273=CARTESIAN_POINT('Origin',(22.8,0.,4.));
#62274=CARTESIAN_POINT('Origin',(22.8,0.,4.));
#62275=CARTESIAN_POINT('Origin',(22.8,0.,4.));
#62276=CARTESIAN_POINT('',(23.3,-1.65327317884893E-16,5.35));
#62277=CARTESIAN_POINT('Origin',(23.3,0.,4.));
#62278=CARTESIAN_POINT('',(22.8,-1.65327317884893E-16,5.35));
#62279=CARTESIAN_POINT('Origin',(23.3,0.,4.));
#62280=CARTESIAN_POINT('Origin',(4.,0.,4.));
#62281=CARTESIAN_POINT('',(0.,0.,0.));
#62282=CARTESIAN_POINT('Origin',(24.7,0.,4.));
#62283=CARTESIAN_POINT('',(25.4,-1.23689326713883E-16,5.01));
#62284=CARTESIAN_POINT('Origin',(25.4,0.,4.));
#62285=CARTESIAN_POINT('',(24.7,-1.23689326713883E-16,5.01));
#62286=CARTESIAN_POINT('',(24.7,-1.23689326713883E-16,5.01));
#62287=CARTESIAN_POINT('Origin',(24.7,0.,4.));
#62288=CARTESIAN_POINT('Origin',(24.7,0.,4.));
#62289=CARTESIAN_POINT('',(25.4,-1.65327317884893E-16,5.35));
#62290=CARTESIAN_POINT('Origin',(25.4,0.,4.));
#62291=CARTESIAN_POINT('',(24.7,-1.65327317884893E-16,5.35));
#62292=CARTESIAN_POINT('',(24.7,-1.65327317884893E-16,5.35));
#62293=CARTESIAN_POINT('Origin',(24.7,0.,4.));
#62294=CARTESIAN_POINT('Origin',(25.4,0.,4.));
#62295=CARTESIAN_POINT('Origin',(24.7,0.,4.));
#62296=CARTESIAN_POINT('',(0.,0.,0.));
#62297=CARTESIAN_POINT('Origin',(25.8,0.99,4.));
#62298=CARTESIAN_POINT('',(25.6809411910021,0.99,4.17298843892006));
#62299=CARTESIAN_POINT('',(25.9190588089979,0.99,4.17298843892006));
#62300=CARTESIAN_POINT('',(25.4,0.99,4.17298843892006));
#62301=CARTESIAN_POINT('Origin',(25.8,0.99,4.));
#62302=CARTESIAN_POINT('Origin',(25.8,0.99,4.));
#62303=CARTESIAN_POINT('',(25.6809411910021,0.99,3.82701156107994));
#62304=CARTESIAN_POINT('',(25.59,1.005,4.));
#62305=CARTESIAN_POINT('Ctrl Pts',(25.6809411910021,0.989999999999999,3.82701156107994));
#62306=CARTESIAN_POINT('Ctrl Pts',(25.6701985776047,0.99129192197638,3.83440513468868));
#62307=CARTESIAN_POINT('Ctrl Pts',(25.6603122906273,0.992653949439047,3.84270286127439));
#62308=CARTESIAN_POINT('Ctrl Pts',(25.6329072257467,0.996748084390898,3.87010792615492));
#62309=CARTESIAN_POINT('Ctrl Pts',(25.6167579436671,0.999695893276376,3.89366983224072));
#62310=CARTESIAN_POINT('Ctrl Pts',(25.5953022060351,1.00385029472357,3.94538709536759));
#62311=CARTESIAN_POINT('Ctrl Pts',(25.59,1.005,3.97354876917015));
#62312=CARTESIAN_POINT('Ctrl Pts',(25.59,1.005,4.));
#62313=CARTESIAN_POINT('',(25.9190588089979,0.99,3.82701156107994));
#62314=CARTESIAN_POINT('Origin',(25.8,0.99,4.));
#62315=CARTESIAN_POINT('Ctrl Pts',(25.9190588089979,0.99,4.17298843892006));
#62316=CARTESIAN_POINT('Ctrl Pts',(25.9298014223953,0.991291921976381,4.16559486531132));
#62317=CARTESIAN_POINT('Ctrl Pts',(25.9396877093727,0.992653949439047,4.15729713872561));
#62318=CARTESIAN_POINT('Ctrl Pts',(25.9670927742533,0.996748084390898,4.12989207384508));
#62319=CARTESIAN_POINT('Ctrl Pts',(25.9832420563329,0.999695893276376,4.10633016775929));
#62320=CARTESIAN_POINT('Ctrl Pts',(26.0046977939649,1.00385029472357,4.05461290463241));
#62321=CARTESIAN_POINT('Ctrl Pts',(26.01,1.005,4.02645123082985));
#62322=CARTESIAN_POINT('Ctrl Pts',(26.01,1.005,3.97354876917015));
#62323=CARTESIAN_POINT('Ctrl Pts',(26.0046977939649,1.00385029472357,3.94538709536759));
#62324=CARTESIAN_POINT('Ctrl Pts',(25.9832420563329,0.999695893276376,3.89366983224072));
#62325=CARTESIAN_POINT('Ctrl Pts',(25.9670927742533,0.996748084390898,3.87010792615492));
#62326=CARTESIAN_POINT('Ctrl Pts',(25.9396877093727,0.992653949439047,3.84270286127439));
#62327=CARTESIAN_POINT('Ctrl Pts',(25.9298014223953,0.991291921976381,3.83440513468868));
#62328=CARTESIAN_POINT('Ctrl Pts',(25.9190588089979,0.99,3.82701156107994));
#62329=CARTESIAN_POINT('Ctrl Pts',(25.59,1.005,4.));
#62330=CARTESIAN_POINT('Ctrl Pts',(25.59,1.005,4.02645123082985));
#62331=CARTESIAN_POINT('Ctrl Pts',(25.5953022060351,1.00385029472357,4.05461290463241));
#62332=CARTESIAN_POINT('Ctrl Pts',(25.6167579436671,0.999695893276376,4.10633016775929));
#62333=CARTESIAN_POINT('Ctrl Pts',(25.6329072257467,0.996748084390898,4.12989207384508));
#62334=CARTESIAN_POINT('Ctrl Pts',(25.6603122906273,0.992653949439047,4.15729713872561));
#62335=CARTESIAN_POINT('Ctrl Pts',(25.6701985776047,0.991291921976381,4.16559486531132));
#62336=CARTESIAN_POINT('Ctrl Pts',(25.6809411910021,0.99,4.17298843892006));
#62337=CARTESIAN_POINT('',(25.59,1.5,4.));
#62338=CARTESIAN_POINT('',(25.59,0.99,4.));
#62339=CARTESIAN_POINT('',(25.8,1.48522725533839,4.21));
#62340=CARTESIAN_POINT('Ctrl Pts',(25.8,1.48522725533839,4.21));
#62341=CARTESIAN_POINT('Ctrl Pts',(25.7735944730755,1.48522725533839,4.21));
#62342=CARTESIAN_POINT('Ctrl Pts',(25.7454529259093,1.48600415954412,4.2047157372696));
#62343=CARTESIAN_POINT('Ctrl Pts',(25.6937237310949,1.48880073282317,4.18327376303633));
#62344=CARTESIAN_POINT('Ctrl Pts',(25.670133075872,1.49077897157582,4.16711792397039));
#62345=CARTESIAN_POINT('Ctrl Pts',(25.632882321789,1.49448481141327,4.12986716988737));
#62346=CARTESIAN_POINT('Ctrl Pts',(25.6167262899986,1.49645455657129,4.10627640830577));
#62347=CARTESIAN_POINT('Ctrl Pts',(25.5952841751738,1.49923165515646,4.0545468514059));
#62348=CARTESIAN_POINT('Ctrl Pts',(25.59,1.5,4.02640517850928));
#62349=CARTESIAN_POINT('Ctrl Pts',(25.59,1.5,4.));
#62350=CARTESIAN_POINT('Ctrl Pts',(25.59,1.5,4.));
#62351=CARTESIAN_POINT('Ctrl Pts',(25.59,1.5,3.97359482149072));
#62352=CARTESIAN_POINT('Ctrl Pts',(25.5952841751738,1.49923165515646,3.9454531485941));
#62353=CARTESIAN_POINT('Ctrl Pts',(25.6167262899986,1.49645455657129,3.89372359169423));
#62354=CARTESIAN_POINT('Ctrl Pts',(25.632882321789,1.49448481141327,3.87013283011263));
#62355=CARTESIAN_POINT('Ctrl Pts',(25.670133075872,1.49077897157582,3.83288207602961));
#62356=CARTESIAN_POINT('Ctrl Pts',(25.6937237310949,1.48880073282317,3.81672623696366));
#62357=CARTESIAN_POINT('Ctrl Pts',(25.7454529259093,1.48600415954412,3.7952842627304));
#62358=CARTESIAN_POINT('Ctrl Pts',(25.7735944730755,1.48522725533839,3.79));
#62359=CARTESIAN_POINT('Ctrl Pts',(25.8264055269245,1.48522725533839,3.79));
#62360=CARTESIAN_POINT('Ctrl Pts',(25.8545470740907,1.48600415954412,3.7952842627304));
#62361=CARTESIAN_POINT('Ctrl Pts',(25.9062762689051,1.48880073282317,3.81672623696367));
#62362=CARTESIAN_POINT('Ctrl Pts',(25.929866924128,1.49077897157582,3.83288207602961));
#62363=CARTESIAN_POINT('Ctrl Pts',(25.967117678211,1.49448481141327,3.87013283011263));
#62364=CARTESIAN_POINT('Ctrl Pts',(25.9832737100014,1.49645455657129,3.89372359169423));
#62365=CARTESIAN_POINT('Ctrl Pts',(26.0047158248262,1.49923165515646,3.9454531485941));
#62366=CARTESIAN_POINT('Ctrl Pts',(26.01,1.5,3.97359482149072));
#62367=CARTESIAN_POINT('Ctrl Pts',(26.01,1.5,4.02640517850928));
#62368=CARTESIAN_POINT('Ctrl Pts',(26.0047158248262,1.49923165515646,4.0545468514059));
#62369=CARTESIAN_POINT('Ctrl Pts',(25.9832737100014,1.49645455657129,4.10627640830577));
#62370=CARTESIAN_POINT('Ctrl Pts',(25.967117678211,1.49448481141327,4.12986716988737));
#62371=CARTESIAN_POINT('Ctrl Pts',(25.929866924128,1.49077897157582,4.16711792397039));
#62372=CARTESIAN_POINT('Ctrl Pts',(25.9062762689051,1.48880073282317,4.18327376303633));
#62373=CARTESIAN_POINT('Ctrl Pts',(25.8545470740907,1.48600415954412,4.20471573726959));
#62374=CARTESIAN_POINT('Ctrl Pts',(25.8264055269245,1.48522725533839,4.21));
#62375=CARTESIAN_POINT('Ctrl Pts',(25.8,1.48522725533839,4.21));
#62376=CARTESIAN_POINT('Origin',(25.8,0.99,4.));
#62377=CARTESIAN_POINT('',(25.4,0.99,3.82701156107994));
#62378=CARTESIAN_POINT('Origin',(25.4,0.,4.));
#62379=CARTESIAN_POINT('',(26.2,-1.23077003314309E-16,5.005));
#62380=CARTESIAN_POINT('Origin',(26.2,0.,4.));
#62381=CARTESIAN_POINT('',(25.4,-1.23077003314309E-16,5.005));
#62382=CARTESIAN_POINT('',(25.4,-1.23077003314309E-16,5.005));
#62383=CARTESIAN_POINT('Origin',(25.4,0.,4.));
#62384=CARTESIAN_POINT('Origin',(25.4,0.,4.));
#62385=CARTESIAN_POINT('',(26.2,-1.83697019872103E-16,5.5));
#62386=CARTESIAN_POINT('Origin',(26.2,0.,4.));
#62387=CARTESIAN_POINT('',(25.4,-1.83697019872103E-16,5.5));
#62388=CARTESIAN_POINT('',(25.4,-1.83697019872103E-16,5.5));
#62389=CARTESIAN_POINT('Origin',(25.4,0.,4.));
#62390=CARTESIAN_POINT('Origin',(26.2,0.,4.));
#62391=CARTESIAN_POINT('Origin',(25.4,0.,4.));
#62392=CARTESIAN_POINT('',(0.,0.,0.));
#62393=CARTESIAN_POINT('Origin',(28.7,0.,6.5));
#62394=CARTESIAN_POINT('',(28.8,-3.06161699786838E-17,6.75));
#62395=CARTESIAN_POINT('Origin',(28.8,0.,6.5));
#62396=CARTESIAN_POINT('',(29.4,3.06161699786838E-17,6.75));
#62397=CARTESIAN_POINT('',(28.7,-3.06161699786838E-17,6.75));
#62398=CARTESIAN_POINT('Origin',(29.4,0.,6.5));
#62399=CARTESIAN_POINT('Origin',(28.,0.99,4.));
#62400=CARTESIAN_POINT('',(27.844436508139,0.99,4.14106735979666));
#62401=CARTESIAN_POINT('',(28.155563491861,0.99,4.14106735979666));
#62402=CARTESIAN_POINT('',(27.,0.99,4.14106735979666));
#62403=CARTESIAN_POINT('Origin',(28.,0.99,4.));
#62404=CARTESIAN_POINT('Origin',(28.,0.99,4.));
#62405=CARTESIAN_POINT('',(27.844436508139,0.99,3.85893264020334));
#62406=CARTESIAN_POINT('',(27.79,1.,4.));
#62407=CARTESIAN_POINT('Ctrl Pts',(27.844436508139,0.99,3.85893264020334));
#62408=CARTESIAN_POINT('Ctrl Pts',(27.8287948476368,0.992457849824465,3.87618164330178));
#62409=CARTESIAN_POINT('Ctrl Pts',(27.815375956669,0.994938193049464,3.8970013568903));
#62410=CARTESIAN_POINT('Ctrl Pts',(27.7953025362756,0.998844492372413,3.94538588560165));
#62411=CARTESIAN_POINT('Ctrl Pts',(27.79,1.,3.97354792631755));
#62412=CARTESIAN_POINT('Ctrl Pts',(27.79,1.,4.));
#62413=CARTESIAN_POINT('',(28.155563491861,0.99,3.85893264020334));
#62414=CARTESIAN_POINT('Origin',(28.,0.99,4.));
#62415=CARTESIAN_POINT('Ctrl Pts',(28.155563491861,0.99,4.14106735979666));
#62416=CARTESIAN_POINT('Ctrl Pts',(28.1712051523632,0.992457849824465,4.12381835669823));
#62417=CARTESIAN_POINT('Ctrl Pts',(28.184624043331,0.994938193049464,4.1029986431097));
#62418=CARTESIAN_POINT('Ctrl Pts',(28.2046974637244,0.998844492372413,4.05461411439835));
#62419=CARTESIAN_POINT('Ctrl Pts',(28.21,1.,4.02645207368245));
#62420=CARTESIAN_POINT('Ctrl Pts',(28.21,1.,3.97354792631755));
#62421=CARTESIAN_POINT('Ctrl Pts',(28.2046974637244,0.998844492372413,3.94538588560165));
#62422=CARTESIAN_POINT('Ctrl Pts',(28.184624043331,0.994938193049464,3.8970013568903));
#62423=CARTESIAN_POINT('Ctrl Pts',(28.1712051523632,0.992457849824465,3.87618164330178));
#62424=CARTESIAN_POINT('Ctrl Pts',(28.155563491861,0.99,3.85893264020334));
#62425=CARTESIAN_POINT('Ctrl Pts',(27.79,1.,4.));
#62426=CARTESIAN_POINT('Ctrl Pts',(27.79,1.,4.02645207368245));
#62427=CARTESIAN_POINT('Ctrl Pts',(27.7953025362756,0.998844492372413,4.05461411439835));
#62428=CARTESIAN_POINT('Ctrl Pts',(27.815375956669,0.994938193049464,4.1029986431097));
#62429=CARTESIAN_POINT('Ctrl Pts',(27.8287948476368,0.992457849824465,4.12381835669823));
#62430=CARTESIAN_POINT('Ctrl Pts',(27.844436508139,0.99,4.14106735979666));
#62431=CARTESIAN_POINT('',(27.79,1.5,4.));
#62432=CARTESIAN_POINT('',(27.79,0.99,4.));
#62433=CARTESIAN_POINT('',(28.,1.48522725533839,4.21));
#62434=CARTESIAN_POINT('Ctrl Pts',(28.,1.48522725533839,4.21));
#62435=CARTESIAN_POINT('Ctrl Pts',(27.9735944730755,1.48522725533839,4.21));
#62436=CARTESIAN_POINT('Ctrl Pts',(27.9454529259093,1.48600415954412,4.20471573726959));
#62437=CARTESIAN_POINT('Ctrl Pts',(27.8937237310949,1.48880073282317,4.18327376303633));
#62438=CARTESIAN_POINT('Ctrl Pts',(27.870133075872,1.49077897157582,4.16711792397039));
#62439=CARTESIAN_POINT('Ctrl Pts',(27.832882321789,1.49448481141327,4.12986716988737));
#62440=CARTESIAN_POINT('Ctrl Pts',(27.8167262899986,1.49645455657129,4.10627640830576));
#62441=CARTESIAN_POINT('Ctrl Pts',(27.7952841751738,1.49923165515646,4.0545468514059));
#62442=CARTESIAN_POINT('Ctrl Pts',(27.79,1.5,4.02640517850928));
#62443=CARTESIAN_POINT('Ctrl Pts',(27.79,1.5,4.));
#62444=CARTESIAN_POINT('Ctrl Pts',(27.79,1.5,4.));
#62445=CARTESIAN_POINT('Ctrl Pts',(27.79,1.5,3.97359482149072));
#62446=CARTESIAN_POINT('Ctrl Pts',(27.7952841751738,1.49923165515646,3.9454531485941));
#62447=CARTESIAN_POINT('Ctrl Pts',(27.8167262899986,1.49645455657129,3.89372359169424));
#62448=CARTESIAN_POINT('Ctrl Pts',(27.832882321789,1.49448481141327,3.87013283011263));
#62449=CARTESIAN_POINT('Ctrl Pts',(27.870133075872,1.49077897157582,3.83288207602961));
#62450=CARTESIAN_POINT('Ctrl Pts',(27.8937237310949,1.48880073282317,3.81672623696367));
#62451=CARTESIAN_POINT('Ctrl Pts',(27.9454529259093,1.48600415954412,3.7952842627304));
#62452=CARTESIAN_POINT('Ctrl Pts',(27.9735944730755,1.48522725533839,3.79));
#62453=CARTESIAN_POINT('Ctrl Pts',(28.0264055269245,1.48522725533839,3.79));
#62454=CARTESIAN_POINT('Ctrl Pts',(28.0545470740907,1.48600415954412,3.7952842627304));
#62455=CARTESIAN_POINT('Ctrl Pts',(28.1062762689051,1.48880073282317,3.81672623696367));
#62456=CARTESIAN_POINT('Ctrl Pts',(28.129866924128,1.49077897157582,3.83288207602961));
#62457=CARTESIAN_POINT('Ctrl Pts',(28.167117678211,1.49448481141327,3.87013283011263));
#62458=CARTESIAN_POINT('Ctrl Pts',(28.1832737100014,1.49645455657129,3.89372359169424));
#62459=CARTESIAN_POINT('Ctrl Pts',(28.2047158248262,1.49923165515646,3.9454531485941));
#62460=CARTESIAN_POINT('Ctrl Pts',(28.21,1.5,3.97359482149072));
#62461=CARTESIAN_POINT('Ctrl Pts',(28.21,1.5,4.02640517850928));
#62462=CARTESIAN_POINT('Ctrl Pts',(28.2047158248262,1.49923165515646,4.0545468514059));
#62463=CARTESIAN_POINT('Ctrl Pts',(28.1832737100014,1.49645455657129,4.10627640830576));
#62464=CARTESIAN_POINT('Ctrl Pts',(28.167117678211,1.49448481141327,4.12986716988737));
#62465=CARTESIAN_POINT('Ctrl Pts',(28.129866924128,1.49077897157582,4.16711792397039));
#62466=CARTESIAN_POINT('Ctrl Pts',(28.1062762689051,1.48880073282317,4.18327376303633));
#62467=CARTESIAN_POINT('Ctrl Pts',(28.0545470740907,1.48600415954412,4.2047157372696));
#62468=CARTESIAN_POINT('Ctrl Pts',(28.0264055269245,1.48522725533839,4.21));
#62469=CARTESIAN_POINT('Ctrl Pts',(28.,1.48522725533839,4.21));
#62470=CARTESIAN_POINT('Origin',(28.,0.99,4.));
#62471=CARTESIAN_POINT('',(27.,0.99,3.85893264020334));
#62472=CARTESIAN_POINT('Origin',(26.9,-0.3,4.));
#62473=CARTESIAN_POINT('',(29.4,-0.3,2.5));
#62474=CARTESIAN_POINT('',(29.4,-0.3,3.04606079858305));
#62475=CARTESIAN_POINT('',(29.4,-0.3,4.));
#62476=CARTESIAN_POINT('',(28.8,-0.3,2.5));
#62477=CARTESIAN_POINT('',(26.9,-0.3,2.5));
#62478=CARTESIAN_POINT('',(28.8,-0.3,2.53030615433009));
#62479=CARTESIAN_POINT('',(28.8,-0.3,4.));
#62480=CARTESIAN_POINT('',(27.,-0.3,2.53030615433009));
#62481=CARTESIAN_POINT('',(27.,-0.3,2.53030615433009));
#62482=CARTESIAN_POINT('',(27.,-0.3,3.04606079858305));
#62483=CARTESIAN_POINT('',(27.,-0.3,4.));
#62484=CARTESIAN_POINT('',(27.,-0.3,3.04606079858305));
#62485=CARTESIAN_POINT('Origin',(26.9,-0.3,2.5));
#62486=CARTESIAN_POINT('',(29.4,0.3,2.5));
#62487=CARTESIAN_POINT('',(29.4,-0.15,2.5));
#62488=CARTESIAN_POINT('',(28.8,0.3,2.5));
#62489=CARTESIAN_POINT('',(26.9,0.3,2.5));
#62490=CARTESIAN_POINT('',(28.8,-0.15,2.5));
#62491=CARTESIAN_POINT('Origin',(26.9,0.3,2.5));
#62492=CARTESIAN_POINT('',(29.4,0.3,3.04606079858305));
#62493=CARTESIAN_POINT('',(29.4,0.3,3.25));
#62494=CARTESIAN_POINT('',(27.,0.3,3.04606079858305));
#62495=CARTESIAN_POINT('',(27.,0.3,3.04606079858305));
#62496=CARTESIAN_POINT('',(27.,0.3,2.53030615433009));
#62497=CARTESIAN_POINT('',(27.,0.3,3.25));
#62498=CARTESIAN_POINT('',(28.8,0.3,2.53030615433009));
#62499=CARTESIAN_POINT('',(27.,0.3,2.53030615433009));
#62500=CARTESIAN_POINT('',(28.8,0.3,3.25));
#62501=CARTESIAN_POINT('Origin',(29.4,0.,4.));
#62502=CARTESIAN_POINT('',(29.4,-4.28626379701574E-16,7.5));
#62503=CARTESIAN_POINT('Origin',(29.4,0.,4.));
#62504=CARTESIAN_POINT('Origin',(29.4,0.,4.));
#62505=CARTESIAN_POINT('Origin',(28.8,0.,4.));
#62506=CARTESIAN_POINT('',(28.8,-4.28626379701574E-16,7.5));
#62507=CARTESIAN_POINT('Origin',(28.8,0.,4.));
#62508=CARTESIAN_POINT('Origin',(28.8,0.,4.));
#62509=CARTESIAN_POINT('Origin',(28.8,0.,4.));
#62510=CARTESIAN_POINT('',(28.8,-4.28626379701574E-16,7.5));
#62511=CARTESIAN_POINT('Origin',(27.,0.,4.));
#62512=CARTESIAN_POINT('Origin',(27.,0.,4.));
#62513=CARTESIAN_POINT('Origin',(27.,0.,4.));
#62514=CARTESIAN_POINT('Origin',(27.,0.,4.));
#62515=CARTESIAN_POINT('Origin',(27.,0.,4.));
#62516=CARTESIAN_POINT('',(0.,0.,0.));
#62517=CARTESIAN_POINT('Origin',(29.4,0.,6.5));
#62518=CARTESIAN_POINT('',(31.03,-4.04133443718627E-17,6.83));
#62519=CARTESIAN_POINT('Origin',(31.03,0.,6.5));
#62520=CARTESIAN_POINT('',(29.4,-4.04133443718627E-17,6.83));
#62521=CARTESIAN_POINT('',(29.4,-4.04133443718627E-17,6.83));
#62522=CARTESIAN_POINT('Origin',(29.4,0.,6.5));
#62523=CARTESIAN_POINT('Origin',(29.4,0.,6.5));
#62524=CARTESIAN_POINT('',(31.03,-4.89858719658942E-17,6.9));
#62525=CARTESIAN_POINT('Origin',(31.03,0.,6.5));
#62526=CARTESIAN_POINT('',(29.4,-4.89858719658942E-17,6.9));
#62527=CARTESIAN_POINT('',(29.4,-4.89858719658942E-17,6.9));
#62528=CARTESIAN_POINT('Origin',(29.4,0.,6.5));
#62529=CARTESIAN_POINT('Origin',(31.03,0.,6.5));
#62530=CARTESIAN_POINT('Origin',(29.4,0.,6.5));
#62531=CARTESIAN_POINT('',(0.,0.,0.));
#62532=CARTESIAN_POINT('Origin',(29.4,0.,6.5));
#62533=CARTESIAN_POINT('',(31.,-4.95981953654678E-17,6.905));
#62534=CARTESIAN_POINT('Origin',(31.,0.,6.5));
#62535=CARTESIAN_POINT('',(29.4,-4.95981953654678E-17,6.905));
#62536=CARTESIAN_POINT('',(29.4,-4.95981953654678E-17,6.905));
#62537=CARTESIAN_POINT('Origin',(29.4,0.,6.5));
#62538=CARTESIAN_POINT('Origin',(29.4,0.,6.5));
#62539=CARTESIAN_POINT('',(31.,-1.10218211923262E-16,7.4));
#62540=CARTESIAN_POINT('Origin',(31.,0.,6.5));
#62541=CARTESIAN_POINT('',(29.4,-1.10218211923262E-16,7.4));
#62542=CARTESIAN_POINT('',(29.4,-1.10218211923262E-16,7.4));
#62543=CARTESIAN_POINT('Origin',(29.4,0.,6.5));
#62544=CARTESIAN_POINT('Origin',(31.,0.,6.5));
#62545=CARTESIAN_POINT('Origin',(29.4,0.,6.5));
#62546=CARTESIAN_POINT('',(0.,0.,0.));
#62547=CARTESIAN_POINT('Origin',(-1.,0.,0.35));
#62548=CARTESIAN_POINT('',(-1.,-0.26,0.6));
#62549=CARTESIAN_POINT('',(-1.,-0.3,0.56));
#62550=CARTESIAN_POINT('',(-1.,-0.2675,0.5925));
#62551=CARTESIAN_POINT('',(-1.,0.26,0.6));
#62552=CARTESIAN_POINT('',(-1.,0.,0.6));
#62553=CARTESIAN_POINT('',(-1.,0.3,0.56));
#62554=CARTESIAN_POINT('',(-1.,0.2675,0.5925));
#62555=CARTESIAN_POINT('',(-1.,0.3,0.04));
#62556=CARTESIAN_POINT('',(-1.,0.3,0.175));
#62557=CARTESIAN_POINT('',(-1.,0.26,0.));
#62558=CARTESIAN_POINT('',(-1.,0.2925,0.0325));
#62559=CARTESIAN_POINT('',(-1.,-0.26,0.));
#62560=CARTESIAN_POINT('',(-1.,0.,0.));
#62561=CARTESIAN_POINT('',(-1.,-0.3,0.04));
#62562=CARTESIAN_POINT('',(-1.,-0.2925,0.0325));
#62563=CARTESIAN_POINT('',(-1.,-0.3,0.175));
#62564=CARTESIAN_POINT('Origin',(0.75,0.28,0.02));
#62565=CARTESIAN_POINT('',(1.,0.3,0.04));
#62566=CARTESIAN_POINT('',(0.75,0.3,0.04));
#62567=CARTESIAN_POINT('',(1.,0.26,0.));
#62568=CARTESIAN_POINT('',(1.,0.2925,0.0325));
#62569=CARTESIAN_POINT('',(0.75,0.26,0.));
#62570=CARTESIAN_POINT('Origin',(1.5,0.3,0.));
#62571=CARTESIAN_POINT('',(1.,0.3,0.56));
#62572=CARTESIAN_POINT('',(0.75,0.3,0.56));
#62573=CARTESIAN_POINT('',(1.,0.3,0.175));
#62574=CARTESIAN_POINT('Origin',(0.75,0.28,0.58));
#62575=CARTESIAN_POINT('',(1.,0.26,0.6));
#62576=CARTESIAN_POINT('',(0.75,0.26,0.6));
#62577=CARTESIAN_POINT('',(1.,0.2675,0.5925));
#62578=CARTESIAN_POINT('Origin',(0.,0.,0.6));
#62579=CARTESIAN_POINT('',(1.,-0.26,0.6));
#62580=CARTESIAN_POINT('',(-0.75,-0.26,0.6));
#62581=CARTESIAN_POINT('',(1.,0.,0.6));
#62582=CARTESIAN_POINT('Origin',(1.,0.,0.35));
#62583=CARTESIAN_POINT('',(1.,-0.26,0.));
#62584=CARTESIAN_POINT('',(1.,-0.3,0.04));
#62585=CARTESIAN_POINT('',(1.,-0.2925,0.0325));
#62586=CARTESIAN_POINT('',(1.,0.,0.));
#62587=CARTESIAN_POINT('',(1.,-0.3,0.56));
#62588=CARTESIAN_POINT('',(1.,-0.2675,0.5925));
#62589=CARTESIAN_POINT('',(1.,-0.3,0.175));
#62590=CARTESIAN_POINT('Origin',(0.,0.,0.));
#62591=CARTESIAN_POINT('',(-0.75,-0.26,0.));
#62592=CARTESIAN_POINT('Origin',(-0.75,-0.28,0.58));
#62593=CARTESIAN_POINT('',(-0.75,-0.3,0.56));
#62594=CARTESIAN_POINT('Origin',(-0.75,-0.28,0.02));
#62595=CARTESIAN_POINT('',(-0.75,-0.3,0.04));
#62596=CARTESIAN_POINT('Origin',(-1.5,-0.3,0.));
#62597=CARTESIAN_POINT('',(0.,0.,0.));
#62598=CARTESIAN_POINT('Origin',(0.0721687836487032,0.,-0.125));
#62599=CARTESIAN_POINT('',(0.0721687836487032,0.,-0.125));
#62600=CARTESIAN_POINT('',(0.144337567297406,0.,0.));
#62601=CARTESIAN_POINT('',(0.117710979560879,0.,-0.0461186027918559));
#62602=CARTESIAN_POINT('',(0.0721687836487032,-0.25,-0.125));
#62603=CARTESIAN_POINT('',(0.0721687836487032,0.,-0.125));
#62604=CARTESIAN_POINT('',(0.144337567297406,-0.25,0.));
#62605=CARTESIAN_POINT('',(0.144337567297406,-0.25,0.));
#62606=CARTESIAN_POINT('',(0.144337567297406,0.,0.));
#62607=CARTESIAN_POINT('Origin',(-0.0721687836487032,0.,-0.125));
#62608=CARTESIAN_POINT('',(-0.0721687836487032,0.,-0.125));
#62609=CARTESIAN_POINT('',(0.0739156081756484,0.,-0.125));
#62610=CARTESIAN_POINT('',(-0.0721687836487032,-0.25,-0.125));
#62611=CARTESIAN_POINT('',(-0.0721687836487032,0.,-0.125));
#62612=CARTESIAN_POINT('',(0.0721687836487032,-0.25,-0.125));
#62613=CARTESIAN_POINT('Origin',(-0.144337567297406,0.,-4.16333634234434E-17));
#62614=CARTESIAN_POINT('',(-0.144337567297406,0.,-1.76762539787485E-17));
#62615=CARTESIAN_POINT('',(-0.0987953713852306,0.,-0.0788813972081442));
#62616=CARTESIAN_POINT('',(-0.144337567297406,-0.25,-2.77555756156289E-17));
#62617=CARTESIAN_POINT('',(-0.144337567297406,0.,-1.76762539787485E-17));
#62618=CARTESIAN_POINT('',(-0.0721687836487032,-0.25,-0.125));
#62619=CARTESIAN_POINT('Origin',(-0.0721687836487033,0.,0.125));
#62620=CARTESIAN_POINT('',(-0.0721687836487033,0.,0.125));
#62621=CARTESIAN_POINT('',(-0.0627109795608791,0.,0.141381397208144));
#62622=CARTESIAN_POINT('',(-0.0721687836487033,-0.25,0.125));
#62623=CARTESIAN_POINT('',(-0.0721687836487033,0.,0.125));
#62624=CARTESIAN_POINT('',(-0.144337567297406,-0.25,-1.76762539787485E-17));
#62625=CARTESIAN_POINT('Origin',(0.0721687836487032,0.,0.125));
#62626=CARTESIAN_POINT('',(0.0721687836487032,0.,0.125));
#62627=CARTESIAN_POINT('',(0.146084391824352,0.,0.125));
#62628=CARTESIAN_POINT('',(0.0721687836487032,-0.25,0.125));
#62629=CARTESIAN_POINT('',(0.0721687836487032,0.,0.125));
#62630=CARTESIAN_POINT('',(-0.0721687836487033,-0.25,0.125));
#62631=CARTESIAN_POINT('Origin',(0.144337567297406,0.,0.));
#62632=CARTESIAN_POINT('',(0.153795371385231,0.,-0.0163813972081441));
#62633=CARTESIAN_POINT('',(0.0721687836487032,-0.25,0.125));
#62634=CARTESIAN_POINT('Origin',(0.,-0.25,0.));
#62635=CARTESIAN_POINT('Origin',(0.22,0.,0.));
#62636=CARTESIAN_POINT('',(-0.22,-8.67361737988404E-18,-2.69422295812418E-17));
#62637=CARTESIAN_POINT('Origin',(0.,0.,0.));
#62638=CARTESIAN_POINT('Origin',(0.,-0.015,0.));
#62639=CARTESIAN_POINT('',(-0.24505,-0.02505,-3.00099698131059E-17));
#62640=CARTESIAN_POINT('Origin',(0.,-0.02505,0.));
#62641=CARTESIAN_POINT('',(-0.235,-0.015,-2.87791997799628E-17));
#62642=CARTESIAN_POINT('Origin',(0.,-0.3775,0.));
#62643=CARTESIAN_POINT('',(-0.24505,-0.72995,3.00099698131059E-17));
#62644=CARTESIAN_POINT('Origin',(0.,-0.72995,0.));
#62645=CARTESIAN_POINT('',(-0.24505,-0.3775,-3.00099698131059E-17));
#62646=CARTESIAN_POINT('Origin',(0.,-0.7625,0.));
#62647=CARTESIAN_POINT('',(-0.175,-0.8,-2.14313189850787E-17));
#62648=CARTESIAN_POINT('Origin',(0.,-0.8,0.));
#62649=CARTESIAN_POINT('',(-0.2125,-0.7625,-2.60237444818813E-17));
#62650=CARTESIAN_POINT('Origin',(0.,-0.8,0.));
#62651=CARTESIAN_POINT('',(0.,0.,0.));
#62652=CARTESIAN_POINT('Origin',(0.,0.,0.));
#62653=CARTESIAN_POINT('',(-0.32,0.16,3.91886975727153E-17));
#62654=CARTESIAN_POINT('Origin',(0.,0.16,0.));
#62655=CARTESIAN_POINT('',(-0.32,0.,3.91886975727153E-17));
#62656=CARTESIAN_POINT('',(-0.32,0.,3.91886975727153E-17));
#62657=CARTESIAN_POINT('Origin',(0.,0.,0.));
#62658=CARTESIAN_POINT('Origin',(0.,0.,0.));
#62659=CARTESIAN_POINT('',(-0.6,0.16,7.34788079488412E-17));
#62660=CARTESIAN_POINT('Origin',(0.,0.16,0.));
#62661=CARTESIAN_POINT('',(-0.6,0.,7.34788079488412E-17));
#62662=CARTESIAN_POINT('',(-0.6,0.,7.34788079488412E-17));
#62663=CARTESIAN_POINT('Origin',(0.,0.,0.));
#62664=CARTESIAN_POINT('Origin',(0.,0.16,0.));
#62665=CARTESIAN_POINT('Origin',(0.,0.,0.));
#62666=CARTESIAN_POINT('',(0.,0.,0.));
#62667=CARTESIAN_POINT('Origin',(0.45,0.6,0.));
#62668=CARTESIAN_POINT('',(-0.45,0.6,-5.51091059616309E-17));
#62669=CARTESIAN_POINT('Origin',(0.,0.6,0.));
#62670=CARTESIAN_POINT('Origin',(0.,0.575,0.));
#62671=CARTESIAN_POINT('',(-0.5,0.55,-6.12323399573677E-17));
#62672=CARTESIAN_POINT('Origin',(0.,0.55,0.));
#62673=CARTESIAN_POINT('',(-0.475,0.575,-5.81707229594993E-17));
#62674=CARTESIAN_POINT('Origin',(0.,0.29,0.));
#62675=CARTESIAN_POINT('',(-0.5,0.0299999999999998,-6.12323399573677E-17));
#62676=CARTESIAN_POINT('Origin',(0.,0.0299999999999998,0.));
#62677=CARTESIAN_POINT('',(-0.5,0.29,-6.12323399573677E-17));
#62678=CARTESIAN_POINT('Origin',(0.,0.0150000000000001,0.));
#62679=CARTESIAN_POINT('',(-0.47,7.11236625150491E-17,-5.75583995599256E-17));
#62680=CARTESIAN_POINT('Origin',(0.,0.,0.));
#62681=CARTESIAN_POINT('',(-0.485,0.0150000000000001,-5.93953697586466E-17));
#62682=CARTESIAN_POINT('Origin',(0.32,0.,0.));
#62683=CARTESIAN_POINT('',(-0.32,-6.93889390390723E-18,-3.91886975727153E-17));
#62684=CARTESIAN_POINT('Origin',(0.,0.,0.));
#62685=CARTESIAN_POINT('Origin',(0.,-0.02,0.));
#62686=CARTESIAN_POINT('',(-0.2942,-0.0515999999999999,3.60291088309151E-17));
#62687=CARTESIAN_POINT('Origin',(0.,-0.0515999999999999,0.));
#62688=CARTESIAN_POINT('',(-0.31,-0.02,-3.7964050773568E-17));
#62689=CARTESIAN_POINT('Origin',(0.,-1.24,0.));
#62690=CARTESIAN_POINT('',(-0.2942,-2.4458,3.60291088309151E-17));
#62691=CARTESIAN_POINT('Origin',(0.,-2.4458,0.));
#62692=CARTESIAN_POINT('',(-0.2942,-1.24,-3.60291088309151E-17));
#62693=CARTESIAN_POINT('Origin',(0.,-2.47,0.));
#62694=CARTESIAN_POINT('',(-0.24,-2.5,-2.93915231795365E-17));
#62695=CARTESIAN_POINT('Origin',(0.,-2.5,0.));
#62696=CARTESIAN_POINT('',(-0.27,-2.47,-3.30654635769785E-17));
#62697=CARTESIAN_POINT('Origin',(0.,-2.5,0.));
#62698=CARTESIAN_POINT('Origin',(0.144337567297406,-0.6,-0.25));
#62699=CARTESIAN_POINT('',(0.288675134594813,-0.6,0.));
#62700=CARTESIAN_POINT('',(0.144337567297406,-0.6,-0.25));
#62701=CARTESIAN_POINT('',(0.288675134594813,-0.6,0.));
#62702=CARTESIAN_POINT('',(0.144337567297406,-0.96,-0.25));
#62703=CARTESIAN_POINT('',(0.144337567297406,-0.6,-0.25));
#62704=CARTESIAN_POINT('',(0.288675134594813,-0.96,0.));
#62705=CARTESIAN_POINT('',(0.288675134594813,-0.96,0.));
#62706=CARTESIAN_POINT('',(0.288675134594813,-0.6,0.));
#62707=CARTESIAN_POINT('Origin',(-0.144337567297406,-0.6,-0.25));
#62708=CARTESIAN_POINT('',(-0.144337567297406,-0.6,-0.25));
#62709=CARTESIAN_POINT('',(0.144337567297406,-0.6,-0.25));
#62710=CARTESIAN_POINT('',(-0.144337567297406,-0.96,-0.25));
#62711=CARTESIAN_POINT('',(-0.144337567297406,-0.6,-0.25));
#62712=CARTESIAN_POINT('',(0.144337567297406,-0.96,-0.25));
#62713=CARTESIAN_POINT('Origin',(-0.288675134594813,-0.6,-8.32667268468867E-17));
#62714=CARTESIAN_POINT('',(-0.288675134594813,-0.6,-3.53525079574969E-17));
#62715=CARTESIAN_POINT('',(-0.144337567297406,-0.6,-0.25));
#62716=CARTESIAN_POINT('',(-0.288675134594813,-0.96,-5.55111512312578E-17));
#62717=CARTESIAN_POINT('',(-0.288675134594813,-0.6,-3.53525079574969E-17));
#62718=CARTESIAN_POINT('',(-0.144337567297406,-0.96,-0.25));
#62719=CARTESIAN_POINT('Origin',(-0.144337567297407,-0.6,0.25));
#62720=CARTESIAN_POINT('',(-0.144337567297407,-0.6,0.25));
#62721=CARTESIAN_POINT('',(-0.288675134594813,-0.6,-3.53525079574969E-17));
#62722=CARTESIAN_POINT('',(-0.144337567297407,-0.96,0.25));
#62723=CARTESIAN_POINT('',(-0.144337567297407,-0.6,0.25));
#62724=CARTESIAN_POINT('',(-0.288675134594813,-0.96,-3.53525079574969E-17));
#62725=CARTESIAN_POINT('Origin',(0.144337567297406,-0.6,0.25));
#62726=CARTESIAN_POINT('',(0.144337567297406,-0.6,0.25));
#62727=CARTESIAN_POINT('',(-0.144337567297407,-0.6,0.25));
#62728=CARTESIAN_POINT('',(0.144337567297406,-0.96,0.25));
#62729=CARTESIAN_POINT('',(0.144337567297406,-0.6,0.25));
#62730=CARTESIAN_POINT('',(-0.144337567297407,-0.96,0.25));
#62731=CARTESIAN_POINT('Origin',(0.288675134594813,-0.6,0.));
#62732=CARTESIAN_POINT('',(0.144337567297406,-0.6,0.25));
#62733=CARTESIAN_POINT('',(0.144337567297406,-0.96,0.25));
#62734=CARTESIAN_POINT('Origin',(0.,-0.6,0.));
#62735=CARTESIAN_POINT('Origin',(0.,-0.96,0.));
#62736=CARTESIAN_POINT('',(0.,0.,0.));
#62737=CARTESIAN_POINT('',(0.,0.,0.));
#62738=CARTESIAN_POINT('',(0.,0.,0.));
#62739=CARTESIAN_POINT('',(0.,0.,0.));
#62740=CARTESIAN_POINT('',(0.,0.,0.));
#62741=CARTESIAN_POINT('',(0.,0.,0.));
#62742=CARTESIAN_POINT('',(0.,0.,0.));
#62743=CARTESIAN_POINT('',(0.,0.,0.));
#62744=CARTESIAN_POINT('',(1.,-7.8,2.2));
#62745=CARTESIAN_POINT('',(1.,-5.5,2.2));
#62746=CARTESIAN_POINT('',(26.,-7.8,2.2));
#62747=CARTESIAN_POINT('',(26.,-5.5,2.2));
#62748=CARTESIAN_POINT('',(2.5,-6.,2.8));
#62749=CARTESIAN_POINT('',(4.5,-6.,3.77));
#62750=CARTESIAN_POINT('',(10.5,-6.,3.77));
#62751=CARTESIAN_POINT('',(16.5,-6.,3.77));
#62752=CARTESIAN_POINT('',(22.5,-6.,3.77));
#62753=CARTESIAN_POINT('',(3.,-2.4,0.));
#62754=CARTESIAN_POINT('',(3.,2.4,0.));
#62755=CARTESIAN_POINT('',(3.,0.,4.));
#62756=CARTESIAN_POINT('',(1.6,-2.1,4.));
#62757=CARTESIAN_POINT('',(1.6,2.1,4.));
#62758=CARTESIAN_POINT('',(1.6,0.,6.1));
#62759=CARTESIAN_POINT('',(24.,-3.5,0.));
#62760=CARTESIAN_POINT('',(24.,3.5,0.));
#62761=CARTESIAN_POINT('',(24.,0.,4.));
#62762=CARTESIAN_POINT('',(25.4,-2.6,4.));
#62763=CARTESIAN_POINT('',(25.4,2.6,4.));
#62764=CARTESIAN_POINT('',(25.4,0.,6.6));
#62765=CARTESIAN_POINT('',(3.5,-9.25,2.4));
#62766=CARTESIAN_POINT('',(23.5,-9.25,2.4));
#62767=CARTESIAN_POINT('',(8.,-1.8,0.6));
#62768=CARTESIAN_POINT('',(18.,-1.8,0.6));
#62769=CARTESIAN_POINT('',(8.,-7.2,0.6));
#62770=CARTESIAN_POINT('',(18.,-7.2,0.6));
#62771=CARTESIAN_POINT('',(0.,0.,0.));
#62772=CARTESIAN_POINT('',(0.,0.,0.));
#62773=CARTESIAN_POINT('',(0.,0.,0.));
#62774=CARTESIAN_POINT('',(0.,0.,0.));
#62775=CARTESIAN_POINT('',(0.,0.,0.));
#62776=CARTESIAN_POINT('',(0.,0.,0.));
#62777=CARTESIAN_POINT('',(28.2,0.,3.35));
#62778=CARTESIAN_POINT('',(25.8,1.8,4.));
#62779=CARTESIAN_POINT('',(28.,1.8,4.));
#62780=CARTESIAN_POINT('',(31.03,0.,6.5));
#62781=CARTESIAN_POINT('',(31.19,0.,6.5));
#62782=CARTESIAN_POINT('',(0.,0.,0.));
#62783=CARTESIAN_POINT('',(0.,0.,0.));
#62784=CARTESIAN_POINT('',(0.,-3.46410161513776,6.));
#62785=CARTESIAN_POINT('',(0.,0.,0.));
#62786=CARTESIAN_POINT('',(9.,-17.,7.2));
#62787=UNCERTAINTY_MEASURE_WITH_UNIT(LENGTH_MEASURE(0.001),#62985,
'DISTANCE_ACCURACY_VALUE',
'Maximum model space distance between geometric entities at asserted c
onnectivities');
#62788=UNCERTAINTY_MEASURE_WITH_UNIT(LENGTH_MEASURE(0.001),#62985,
'DISTANCE_ACCURACY_VALUE',
'Maximum model space distance between geometric entities at asserted c
onnectivities');
#62789=UNCERTAINTY_MEASURE_WITH_UNIT(LENGTH_MEASURE(0.001),#62985,
'DISTANCE_ACCURACY_VALUE',
'Maximum model space distance between geometric entities at asserted c
onnectivities');
#62790=UNCERTAINTY_MEASURE_WITH_UNIT(LENGTH_MEASURE(0.001),#62985,
'DISTANCE_ACCURACY_VALUE',
'Maximum model space distance between geometric entities at asserted c
onnectivities');
#62791=UNCERTAINTY_MEASURE_WITH_UNIT(LENGTH_MEASURE(0.001),#62985,
'DISTANCE_ACCURACY_VALUE',
'Maximum model space distance between geometric entities at asserted c
onnectivities');
#62792=UNCERTAINTY_MEASURE_WITH_UNIT(LENGTH_MEASURE(0.001),#62985,
'DISTANCE_ACCURACY_VALUE',
'Maximum model space distance between geometric entities at asserted c
onnectivities');
#62793=UNCERTAINTY_MEASURE_WITH_UNIT(LENGTH_MEASURE(0.001),#62985,
'DISTANCE_ACCURACY_VALUE',
'Maximum model space distance between geometric entities at asserted c
onnectivities');
#62794=UNCERTAINTY_MEASURE_WITH_UNIT(LENGTH_MEASURE(0.001),#62985,
'DISTANCE_ACCURACY_VALUE',
'Maximum model space distance between geometric entities at asserted c
onnectivities');
#62795=UNCERTAINTY_MEASURE_WITH_UNIT(LENGTH_MEASURE(0.001),#62985,
'DISTANCE_ACCURACY_VALUE',
'Maximum model space distance between geometric entities at asserted c
onnectivities');
#62796=UNCERTAINTY_MEASURE_WITH_UNIT(LENGTH_MEASURE(0.001),#62985,
'DISTANCE_ACCURACY_VALUE',
'Maximum model space distance between geometric entities at asserted c
onnectivities');
#62797=UNCERTAINTY_MEASURE_WITH_UNIT(LENGTH_MEASURE(0.001),#62985,
'DISTANCE_ACCURACY_VALUE',
'Maximum model space distance between geometric entities at asserted c
onnectivities');
#62798=UNCERTAINTY_MEASURE_WITH_UNIT(LENGTH_MEASURE(0.001),#62985,
'DISTANCE_ACCURACY_VALUE',
'Maximum model space distance between geometric entities at asserted c
onnectivities');
#62799=UNCERTAINTY_MEASURE_WITH_UNIT(LENGTH_MEASURE(0.001),#62985,
'DISTANCE_ACCURACY_VALUE',
'Maximum model space distance between geometric entities at asserted c
onnectivities');
#62800=UNCERTAINTY_MEASURE_WITH_UNIT(LENGTH_MEASURE(0.001),#62985,
'DISTANCE_ACCURACY_VALUE',
'Maximum model space distance between geometric entities at asserted c
onnectivities');
#62801=UNCERTAINTY_MEASURE_WITH_UNIT(LENGTH_MEASURE(0.001),#62985,
'DISTANCE_ACCURACY_VALUE',
'Maximum model space distance between geometric entities at asserted c
onnectivities');
#62802=UNCERTAINTY_MEASURE_WITH_UNIT(LENGTH_MEASURE(0.001),#62985,
'DISTANCE_ACCURACY_VALUE',
'Maximum model space distance between geometric entities at asserted c
onnectivities');
#62803=UNCERTAINTY_MEASURE_WITH_UNIT(LENGTH_MEASURE(0.001),#62985,
'DISTANCE_ACCURACY_VALUE',
'Maximum model space distance between geometric entities at asserted c
onnectivities');
#62804=UNCERTAINTY_MEASURE_WITH_UNIT(LENGTH_MEASURE(0.001),#62985,
'DISTANCE_ACCURACY_VALUE',
'Maximum model space distance between geometric entities at asserted c
onnectivities');
#62805=UNCERTAINTY_MEASURE_WITH_UNIT(LENGTH_MEASURE(0.001),#62985,
'DISTANCE_ACCURACY_VALUE',
'Maximum model space distance between geometric entities at asserted c
onnectivities');
#62806=UNCERTAINTY_MEASURE_WITH_UNIT(LENGTH_MEASURE(0.001),#62985,
'DISTANCE_ACCURACY_VALUE',
'Maximum model space distance between geometric entities at asserted c
onnectivities');
#62807=UNCERTAINTY_MEASURE_WITH_UNIT(LENGTH_MEASURE(0.001),#62985,
'DISTANCE_ACCURACY_VALUE',
'Maximum model space distance between geometric entities at asserted c
onnectivities');
#62808=UNCERTAINTY_MEASURE_WITH_UNIT(LENGTH_MEASURE(0.001),#62985,
'DISTANCE_ACCURACY_VALUE',
'Maximum model space distance between geometric entities at asserted c
onnectivities');
#62809=UNCERTAINTY_MEASURE_WITH_UNIT(LENGTH_MEASURE(0.001),#62985,
'DISTANCE_ACCURACY_VALUE',
'Maximum model space distance between geometric entities at asserted c
onnectivities');
#62810=UNCERTAINTY_MEASURE_WITH_UNIT(LENGTH_MEASURE(0.001),#62985,
'DISTANCE_ACCURACY_VALUE',
'Maximum model space distance between geometric entities at asserted c
onnectivities');
#62811=UNCERTAINTY_MEASURE_WITH_UNIT(LENGTH_MEASURE(0.001),#62985,
'DISTANCE_ACCURACY_VALUE',
'Maximum model space distance between geometric entities at asserted c
onnectivities');
#62812=UNCERTAINTY_MEASURE_WITH_UNIT(LENGTH_MEASURE(0.001),#62985,
'DISTANCE_ACCURACY_VALUE',
'Maximum model space distance between geometric entities at asserted c
onnectivities');
#62813=UNCERTAINTY_MEASURE_WITH_UNIT(LENGTH_MEASURE(0.001),#62985,
'DISTANCE_ACCURACY_VALUE',
'Maximum model space distance between geometric entities at asserted c
onnectivities');
#62814=UNCERTAINTY_MEASURE_WITH_UNIT(LENGTH_MEASURE(0.001),#62985,
'DISTANCE_ACCURACY_VALUE',
'Maximum model space distance between geometric entities at asserted c
onnectivities');
#62815=UNCERTAINTY_MEASURE_WITH_UNIT(LENGTH_MEASURE(0.001),#62985,
'DISTANCE_ACCURACY_VALUE',
'Maximum model space distance between geometric entities at asserted c
onnectivities');
#62816=UNCERTAINTY_MEASURE_WITH_UNIT(LENGTH_MEASURE(0.001),#62985,
'DISTANCE_ACCURACY_VALUE',
'Maximum model space distance between geometric entities at asserted c
onnectivities');
#62817=UNCERTAINTY_MEASURE_WITH_UNIT(LENGTH_MEASURE(0.001),#62985,
'DISTANCE_ACCURACY_VALUE',
'Maximum model space distance between geometric entities at asserted c
onnectivities');
#62818=UNCERTAINTY_MEASURE_WITH_UNIT(LENGTH_MEASURE(0.001),#62985,
'DISTANCE_ACCURACY_VALUE',
'Maximum model space distance between geometric entities at asserted c
onnectivities');
#62819=UNCERTAINTY_MEASURE_WITH_UNIT(LENGTH_MEASURE(0.001),#62985,
'DISTANCE_ACCURACY_VALUE',
'Maximum model space distance between geometric entities at asserted c
onnectivities');
#62820=UNCERTAINTY_MEASURE_WITH_UNIT(LENGTH_MEASURE(0.001),#62985,
'DISTANCE_ACCURACY_VALUE',
'Maximum model space distance between geometric entities at asserted c
onnectivities');
#62821=UNCERTAINTY_MEASURE_WITH_UNIT(LENGTH_MEASURE(0.001),#62985,
'DISTANCE_ACCURACY_VALUE',
'Maximum model space distance between geometric entities at asserted c
onnectivities');
#62822=UNCERTAINTY_MEASURE_WITH_UNIT(LENGTH_MEASURE(0.001),#62985,
'DISTANCE_ACCURACY_VALUE',
'Maximum model space distance between geometric entities at asserted c
onnectivities');
#62823=UNCERTAINTY_MEASURE_WITH_UNIT(LENGTH_MEASURE(0.001),#62985,
'DISTANCE_ACCURACY_VALUE',
'Maximum model space distance between geometric entities at asserted c
onnectivities');
#62824=UNCERTAINTY_MEASURE_WITH_UNIT(LENGTH_MEASURE(0.001),#62985,
'DISTANCE_ACCURACY_VALUE',
'Maximum model space distance between geometric entities at asserted c
onnectivities');
#62825=UNCERTAINTY_MEASURE_WITH_UNIT(LENGTH_MEASURE(0.001),#62985,
'DISTANCE_ACCURACY_VALUE',
'Maximum model space distance between geometric entities at asserted c
onnectivities');
#62826=UNCERTAINTY_MEASURE_WITH_UNIT(LENGTH_MEASURE(0.001),#62985,
'DISTANCE_ACCURACY_VALUE',
'Maximum model space distance between geometric entities at asserted c
onnectivities');
#62827=UNCERTAINTY_MEASURE_WITH_UNIT(LENGTH_MEASURE(0.001),#62985,
'DISTANCE_ACCURACY_VALUE',
'Maximum model space distance between geometric entities at asserted c
onnectivities');
#62828=UNCERTAINTY_MEASURE_WITH_UNIT(LENGTH_MEASURE(0.001),#62985,
'DISTANCE_ACCURACY_VALUE',
'Maximum model space distance between geometric entities at asserted c
onnectivities');
#62829=UNCERTAINTY_MEASURE_WITH_UNIT(LENGTH_MEASURE(0.001),#62985,
'DISTANCE_ACCURACY_VALUE',
'Maximum model space distance between geometric entities at asserted c
onnectivities');
#62830=UNCERTAINTY_MEASURE_WITH_UNIT(LENGTH_MEASURE(0.001),#62985,
'DISTANCE_ACCURACY_VALUE',
'Maximum model space distance between geometric entities at asserted c
onnectivities');
#62831=UNCERTAINTY_MEASURE_WITH_UNIT(LENGTH_MEASURE(0.001),#62985,
'DISTANCE_ACCURACY_VALUE',
'Maximum model space distance between geometric entities at asserted c
onnectivities');
#62832=UNCERTAINTY_MEASURE_WITH_UNIT(LENGTH_MEASURE(0.001),#62985,
'DISTANCE_ACCURACY_VALUE',
'Maximum model space distance between geometric entities at asserted c
onnectivities');
#62833=UNCERTAINTY_MEASURE_WITH_UNIT(LENGTH_MEASURE(0.001),#62985,
'DISTANCE_ACCURACY_VALUE',
'Maximum model space distance between geometric entities at asserted c
onnectivities');
#62834=UNCERTAINTY_MEASURE_WITH_UNIT(LENGTH_MEASURE(0.001),#62985,
'DISTANCE_ACCURACY_VALUE',
'Maximum model space distance between geometric entities at asserted c
onnectivities');
#62835=UNCERTAINTY_MEASURE_WITH_UNIT(LENGTH_MEASURE(0.001),#62985,
'DISTANCE_ACCURACY_VALUE',
'Maximum model space distance between geometric entities at asserted c
onnectivities');
#62836=UNCERTAINTY_MEASURE_WITH_UNIT(LENGTH_MEASURE(0.001),#62985,
'DISTANCE_ACCURACY_VALUE',
'Maximum model space distance between geometric entities at asserted c
onnectivities');
#62837=UNCERTAINTY_MEASURE_WITH_UNIT(LENGTH_MEASURE(0.001),#62985,
'DISTANCE_ACCURACY_VALUE',
'Maximum model space distance between geometric entities at asserted c
onnectivities');
#62838=UNCERTAINTY_MEASURE_WITH_UNIT(LENGTH_MEASURE(0.001),#62985,
'DISTANCE_ACCURACY_VALUE',
'Maximum model space distance between geometric entities at asserted c
onnectivities');
#62839=UNCERTAINTY_MEASURE_WITH_UNIT(LENGTH_MEASURE(0.001),#62985,
'DISTANCE_ACCURACY_VALUE',
'Maximum model space distance between geometric entities at asserted c
onnectivities');
#62840=UNCERTAINTY_MEASURE_WITH_UNIT(LENGTH_MEASURE(0.001),#62985,
'DISTANCE_ACCURACY_VALUE',
'Maximum model space distance between geometric entities at asserted c
onnectivities');
#62841=UNCERTAINTY_MEASURE_WITH_UNIT(LENGTH_MEASURE(0.001),#62985,
'DISTANCE_ACCURACY_VALUE',
'Maximum model space distance between geometric entities at asserted c
onnectivities');
#62842=UNCERTAINTY_MEASURE_WITH_UNIT(LENGTH_MEASURE(0.001),#62985,
'DISTANCE_ACCURACY_VALUE',
'Maximum model space distance between geometric entities at asserted c
onnectivities');
#62843=UNCERTAINTY_MEASURE_WITH_UNIT(LENGTH_MEASURE(0.001),#62985,
'DISTANCE_ACCURACY_VALUE',
'Maximum model space distance between geometric entities at asserted c
onnectivities');
#62844=UNCERTAINTY_MEASURE_WITH_UNIT(LENGTH_MEASURE(0.001),#62985,
'DISTANCE_ACCURACY_VALUE',
'Maximum model space distance between geometric entities at asserted c
onnectivities');
#62845=UNCERTAINTY_MEASURE_WITH_UNIT(LENGTH_MEASURE(0.001),#62985,
'DISTANCE_ACCURACY_VALUE',
'Maximum model space distance between geometric entities at asserted c
onnectivities');
#62846=UNCERTAINTY_MEASURE_WITH_UNIT(LENGTH_MEASURE(0.001),#62985,
'DISTANCE_ACCURACY_VALUE',
'Maximum model space distance between geometric entities at asserted c
onnectivities');
#62847=UNCERTAINTY_MEASURE_WITH_UNIT(LENGTH_MEASURE(0.001),#62985,
'DISTANCE_ACCURACY_VALUE',
'Maximum model space distance between geometric entities at asserted c
onnectivities');
#62848=UNCERTAINTY_MEASURE_WITH_UNIT(LENGTH_MEASURE(0.001),#62985,
'DISTANCE_ACCURACY_VALUE',
'Maximum model space distance between geometric entities at asserted c
onnectivities');
#62849=UNCERTAINTY_MEASURE_WITH_UNIT(LENGTH_MEASURE(0.001),#62985,
'DISTANCE_ACCURACY_VALUE',
'Maximum model space distance between geometric entities at asserted c
onnectivities');
#62850=UNCERTAINTY_MEASURE_WITH_UNIT(LENGTH_MEASURE(0.001),#62985,
'DISTANCE_ACCURACY_VALUE',
'Maximum model space distance between geometric entities at asserted c
onnectivities');
#62851=UNCERTAINTY_MEASURE_WITH_UNIT(LENGTH_MEASURE(0.001),#62985,
'DISTANCE_ACCURACY_VALUE',
'Maximum model space distance between geometric entities at asserted c
onnectivities');
#62852=UNCERTAINTY_MEASURE_WITH_UNIT(LENGTH_MEASURE(0.001),#62985,
'DISTANCE_ACCURACY_VALUE',
'Maximum model space distance between geometric entities at asserted c
onnectivities');
#62853=UNCERTAINTY_MEASURE_WITH_UNIT(LENGTH_MEASURE(0.001),#62985,
'DISTANCE_ACCURACY_VALUE',
'Maximum model space distance between geometric entities at asserted c
onnectivities');
#62854=UNCERTAINTY_MEASURE_WITH_UNIT(LENGTH_MEASURE(0.001),#62985,
'DISTANCE_ACCURACY_VALUE',
'Maximum model space distance between geometric entities at asserted c
onnectivities');
#62855=UNCERTAINTY_MEASURE_WITH_UNIT(LENGTH_MEASURE(0.001),#62985,
'DISTANCE_ACCURACY_VALUE',
'Maximum model space distance between geometric entities at asserted c
onnectivities');
#62856=UNCERTAINTY_MEASURE_WITH_UNIT(LENGTH_MEASURE(0.001),#62985,
'DISTANCE_ACCURACY_VALUE',
'Maximum model space distance between geometric entities at asserted c
onnectivities');
#62857=UNCERTAINTY_MEASURE_WITH_UNIT(LENGTH_MEASURE(0.001),#62985,
'DISTANCE_ACCURACY_VALUE',
'Maximum model space distance between geometric entities at asserted c
onnectivities');
#62858=UNCERTAINTY_MEASURE_WITH_UNIT(LENGTH_MEASURE(0.001),#62985,
'DISTANCE_ACCURACY_VALUE',
'Maximum model space distance between geometric entities at asserted c
onnectivities');
#62859=UNCERTAINTY_MEASURE_WITH_UNIT(LENGTH_MEASURE(0.001),#62985,
'DISTANCE_ACCURACY_VALUE',
'Maximum model space distance between geometric entities at asserted c
onnectivities');
#62860=UNCERTAINTY_MEASURE_WITH_UNIT(LENGTH_MEASURE(0.001),#62985,
'DISTANCE_ACCURACY_VALUE',
'Maximum model space distance between geometric entities at asserted c
onnectivities');
#62861=UNCERTAINTY_MEASURE_WITH_UNIT(LENGTH_MEASURE(0.001),#62985,
'DISTANCE_ACCURACY_VALUE',
'Maximum model space distance between geometric entities at asserted c
onnectivities');
#62862=UNCERTAINTY_MEASURE_WITH_UNIT(LENGTH_MEASURE(0.001),#62985,
'DISTANCE_ACCURACY_VALUE',
'Maximum model space distance between geometric entities at asserted c
onnectivities');
#62863=UNCERTAINTY_MEASURE_WITH_UNIT(LENGTH_MEASURE(0.001),#62985,
'DISTANCE_ACCURACY_VALUE',
'Maximum model space distance between geometric entities at asserted c
onnectivities');
#62864=UNCERTAINTY_MEASURE_WITH_UNIT(LENGTH_MEASURE(0.001),#62985,
'DISTANCE_ACCURACY_VALUE',
'Maximum model space distance between geometric entities at asserted c
onnectivities');
#62865=UNCERTAINTY_MEASURE_WITH_UNIT(LENGTH_MEASURE(0.001),#62985,
'DISTANCE_ACCURACY_VALUE',
'Maximum model space distance between geometric entities at asserted c
onnectivities');
#62866=UNCERTAINTY_MEASURE_WITH_UNIT(LENGTH_MEASURE(0.001),#62985,
'DISTANCE_ACCURACY_VALUE',
'Maximum model space distance between geometric entities at asserted c
onnectivities');
#62867=UNCERTAINTY_MEASURE_WITH_UNIT(LENGTH_MEASURE(0.001),#62985,
'DISTANCE_ACCURACY_VALUE',
'Maximum model space distance between geometric entities at asserted c
onnectivities');
#62868=UNCERTAINTY_MEASURE_WITH_UNIT(LENGTH_MEASURE(0.001),#62985,
'DISTANCE_ACCURACY_VALUE',
'Maximum model space distance between geometric entities at asserted c
onnectivities');
#62869=UNCERTAINTY_MEASURE_WITH_UNIT(LENGTH_MEASURE(0.001),#62985,
'DISTANCE_ACCURACY_VALUE',
'Maximum model space distance between geometric entities at asserted c
onnectivities');
#62870=UNCERTAINTY_MEASURE_WITH_UNIT(LENGTH_MEASURE(0.001),#62985,
'DISTANCE_ACCURACY_VALUE',
'Maximum model space distance between geometric entities at asserted c
onnectivities');
#62871=UNCERTAINTY_MEASURE_WITH_UNIT(LENGTH_MEASURE(0.001),#62985,
'DISTANCE_ACCURACY_VALUE',
'Maximum model space distance between geometric entities at asserted c
onnectivities');
#62872=UNCERTAINTY_MEASURE_WITH_UNIT(LENGTH_MEASURE(0.001),#62985,
'DISTANCE_ACCURACY_VALUE',
'Maximum model space distance between geometric entities at asserted c
onnectivities');
#62873=UNCERTAINTY_MEASURE_WITH_UNIT(LENGTH_MEASURE(0.001),#62985,
'DISTANCE_ACCURACY_VALUE',
'Maximum model space distance between geometric entities at asserted c
onnectivities');
#62874=UNCERTAINTY_MEASURE_WITH_UNIT(LENGTH_MEASURE(0.001),#62985,
'DISTANCE_ACCURACY_VALUE',
'Maximum model space distance between geometric entities at asserted c
onnectivities');
#62875=UNCERTAINTY_MEASURE_WITH_UNIT(LENGTH_MEASURE(0.001),#62985,
'DISTANCE_ACCURACY_VALUE',
'Maximum model space distance between geometric entities at asserted c
onnectivities');
#62876=UNCERTAINTY_MEASURE_WITH_UNIT(LENGTH_MEASURE(0.001),#62985,
'DISTANCE_ACCURACY_VALUE',
'Maximum model space distance between geometric entities at asserted c
onnectivities');
#62877=UNCERTAINTY_MEASURE_WITH_UNIT(LENGTH_MEASURE(0.001),#62985,
'DISTANCE_ACCURACY_VALUE',
'Maximum model space distance between geometric entities at asserted c
onnectivities');
#62878=UNCERTAINTY_MEASURE_WITH_UNIT(LENGTH_MEASURE(0.001),#62985,
'DISTANCE_ACCURACY_VALUE',
'Maximum model space distance between geometric entities at asserted c
onnectivities');
#62879=UNCERTAINTY_MEASURE_WITH_UNIT(LENGTH_MEASURE(0.001),#62985,
'DISTANCE_ACCURACY_VALUE',
'Maximum model space distance between geometric entities at asserted c
onnectivities');
#62880=UNCERTAINTY_MEASURE_WITH_UNIT(LENGTH_MEASURE(0.001),#62985,
'DISTANCE_ACCURACY_VALUE',
'Maximum model space distance between geometric entities at asserted c
onnectivities');
#62881=UNCERTAINTY_MEASURE_WITH_UNIT(LENGTH_MEASURE(0.001),#62985,
'DISTANCE_ACCURACY_VALUE',
'Maximum model space distance between geometric entities at asserted c
onnectivities');
#62882=UNCERTAINTY_MEASURE_WITH_UNIT(LENGTH_MEASURE(0.001),#62985,
'DISTANCE_ACCURACY_VALUE',
'Maximum model space distance between geometric entities at asserted c
onnectivities');
#62883=UNCERTAINTY_MEASURE_WITH_UNIT(LENGTH_MEASURE(0.001),#62985,
'DISTANCE_ACCURACY_VALUE',
'Maximum model space distance between geometric entities at asserted c
onnectivities');
#62884=UNCERTAINTY_MEASURE_WITH_UNIT(LENGTH_MEASURE(0.001),#62985,
'DISTANCE_ACCURACY_VALUE',
'Maximum model space distance between geometric entities at asserted c
onnectivities');
#62885=UNCERTAINTY_MEASURE_WITH_UNIT(LENGTH_MEASURE(0.001),#62985,
'DISTANCE_ACCURACY_VALUE',
'Maximum model space distance between geometric entities at asserted c
onnectivities');
#62886=(
GEOMETRIC_REPRESENTATION_CONTEXT(3)
GLOBAL_UNCERTAINTY_ASSIGNED_CONTEXT((#62787))
GLOBAL_UNIT_ASSIGNED_CONTEXT((#62985,#62987,#62988))
REPRESENTATION_CONTEXT('','3D')
);
#62887=(
GEOMETRIC_REPRESENTATION_CONTEXT(3)
GLOBAL_UNCERTAINTY_ASSIGNED_CONTEXT((#62788))
GLOBAL_UNIT_ASSIGNED_CONTEXT((#62985,#62987,#62988))
REPRESENTATION_CONTEXT('','3D')
);
#62888=(
GEOMETRIC_REPRESENTATION_CONTEXT(3)
GLOBAL_UNCERTAINTY_ASSIGNED_CONTEXT((#62789))
GLOBAL_UNIT_ASSIGNED_CONTEXT((#62985,#62987,#62988))
REPRESENTATION_CONTEXT('','3D')
);
#62889=(
GEOMETRIC_REPRESENTATION_CONTEXT(3)
GLOBAL_UNCERTAINTY_ASSIGNED_CONTEXT((#62790))
GLOBAL_UNIT_ASSIGNED_CONTEXT((#62985,#62987,#62988))
REPRESENTATION_CONTEXT('','3D')
);
#62890=(
GEOMETRIC_REPRESENTATION_CONTEXT(3)
GLOBAL_UNCERTAINTY_ASSIGNED_CONTEXT((#62791))
GLOBAL_UNIT_ASSIGNED_CONTEXT((#62985,#62987,#62988))
REPRESENTATION_CONTEXT('','3D')
);
#62891=(
GEOMETRIC_REPRESENTATION_CONTEXT(3)
GLOBAL_UNCERTAINTY_ASSIGNED_CONTEXT((#62792))
GLOBAL_UNIT_ASSIGNED_CONTEXT((#62985,#62987,#62988))
REPRESENTATION_CONTEXT('','3D')
);
#62892=(
GEOMETRIC_REPRESENTATION_CONTEXT(3)
GLOBAL_UNCERTAINTY_ASSIGNED_CONTEXT((#62793))
GLOBAL_UNIT_ASSIGNED_CONTEXT((#62985,#62987,#62988))
REPRESENTATION_CONTEXT('','3D')
);
#62893=(
GEOMETRIC_REPRESENTATION_CONTEXT(3)
GLOBAL_UNCERTAINTY_ASSIGNED_CONTEXT((#62794))
GLOBAL_UNIT_ASSIGNED_CONTEXT((#62985,#62987,#62988))
REPRESENTATION_CONTEXT('','3D')
);
#62894=(
GEOMETRIC_REPRESENTATION_CONTEXT(3)
GLOBAL_UNCERTAINTY_ASSIGNED_CONTEXT((#62795))
GLOBAL_UNIT_ASSIGNED_CONTEXT((#62985,#62987,#62988))
REPRESENTATION_CONTEXT('','3D')
);
#62895=(
GEOMETRIC_REPRESENTATION_CONTEXT(3)
GLOBAL_UNCERTAINTY_ASSIGNED_CONTEXT((#62796))
GLOBAL_UNIT_ASSIGNED_CONTEXT((#62985,#62987,#62988))
REPRESENTATION_CONTEXT('','3D')
);
#62896=(
GEOMETRIC_REPRESENTATION_CONTEXT(3)
GLOBAL_UNCERTAINTY_ASSIGNED_CONTEXT((#62797))
GLOBAL_UNIT_ASSIGNED_CONTEXT((#62985,#62987,#62988))
REPRESENTATION_CONTEXT('','3D')
);
#62897=(
GEOMETRIC_REPRESENTATION_CONTEXT(3)
GLOBAL_UNCERTAINTY_ASSIGNED_CONTEXT((#62798))
GLOBAL_UNIT_ASSIGNED_CONTEXT((#62985,#62987,#62988))
REPRESENTATION_CONTEXT('','3D')
);
#62898=(
GEOMETRIC_REPRESENTATION_CONTEXT(3)
GLOBAL_UNCERTAINTY_ASSIGNED_CONTEXT((#62799))
GLOBAL_UNIT_ASSIGNED_CONTEXT((#62985,#62987,#62988))
REPRESENTATION_CONTEXT('','3D')
);
#62899=(
GEOMETRIC_REPRESENTATION_CONTEXT(3)
GLOBAL_UNCERTAINTY_ASSIGNED_CONTEXT((#62800))
GLOBAL_UNIT_ASSIGNED_CONTEXT((#62985,#62987,#62988))
REPRESENTATION_CONTEXT('','3D')
);
#62900=(
GEOMETRIC_REPRESENTATION_CONTEXT(3)
GLOBAL_UNCERTAINTY_ASSIGNED_CONTEXT((#62801))
GLOBAL_UNIT_ASSIGNED_CONTEXT((#62985,#62987,#62988))
REPRESENTATION_CONTEXT('','3D')
);
#62901=(
GEOMETRIC_REPRESENTATION_CONTEXT(3)
GLOBAL_UNCERTAINTY_ASSIGNED_CONTEXT((#62802))
GLOBAL_UNIT_ASSIGNED_CONTEXT((#62985,#62987,#62988))
REPRESENTATION_CONTEXT('','3D')
);
#62902=(
GEOMETRIC_REPRESENTATION_CONTEXT(3)
GLOBAL_UNCERTAINTY_ASSIGNED_CONTEXT((#62803))
GLOBAL_UNIT_ASSIGNED_CONTEXT((#62985,#62987,#62988))
REPRESENTATION_CONTEXT('','3D')
);
#62903=(
GEOMETRIC_REPRESENTATION_CONTEXT(3)
GLOBAL_UNCERTAINTY_ASSIGNED_CONTEXT((#62804))
GLOBAL_UNIT_ASSIGNED_CONTEXT((#62985,#62987,#62988))
REPRESENTATION_CONTEXT('','3D')
);
#62904=(
GEOMETRIC_REPRESENTATION_CONTEXT(3)
GLOBAL_UNCERTAINTY_ASSIGNED_CONTEXT((#62805))
GLOBAL_UNIT_ASSIGNED_CONTEXT((#62985,#62987,#62988))
REPRESENTATION_CONTEXT('','3D')
);
#62905=(
GEOMETRIC_REPRESENTATION_CONTEXT(3)
GLOBAL_UNCERTAINTY_ASSIGNED_CONTEXT((#62806))
GLOBAL_UNIT_ASSIGNED_CONTEXT((#62985,#62987,#62988))
REPRESENTATION_CONTEXT('','3D')
);
#62906=(
GEOMETRIC_REPRESENTATION_CONTEXT(3)
GLOBAL_UNCERTAINTY_ASSIGNED_CONTEXT((#62807))
GLOBAL_UNIT_ASSIGNED_CONTEXT((#62985,#62987,#62988))
REPRESENTATION_CONTEXT('','3D')
);
#62907=(
GEOMETRIC_REPRESENTATION_CONTEXT(3)
GLOBAL_UNCERTAINTY_ASSIGNED_CONTEXT((#62808))
GLOBAL_UNIT_ASSIGNED_CONTEXT((#62985,#62987,#62988))
REPRESENTATION_CONTEXT('','3D')
);
#62908=(
GEOMETRIC_REPRESENTATION_CONTEXT(3)
GLOBAL_UNCERTAINTY_ASSIGNED_CONTEXT((#62809))
GLOBAL_UNIT_ASSIGNED_CONTEXT((#62985,#62987,#62988))
REPRESENTATION_CONTEXT('','3D')
);
#62909=(
GEOMETRIC_REPRESENTATION_CONTEXT(3)
GLOBAL_UNCERTAINTY_ASSIGNED_CONTEXT((#62810))
GLOBAL_UNIT_ASSIGNED_CONTEXT((#62985,#62987,#62988))
REPRESENTATION_CONTEXT('','3D')
);
#62910=(
GEOMETRIC_REPRESENTATION_CONTEXT(3)
GLOBAL_UNCERTAINTY_ASSIGNED_CONTEXT((#62811))
GLOBAL_UNIT_ASSIGNED_CONTEXT((#62985,#62987,#62988))
REPRESENTATION_CONTEXT('','3D')
);
#62911=(
GEOMETRIC_REPRESENTATION_CONTEXT(3)
GLOBAL_UNCERTAINTY_ASSIGNED_CONTEXT((#62812))
GLOBAL_UNIT_ASSIGNED_CONTEXT((#62985,#62987,#62988))
REPRESENTATION_CONTEXT('','3D')
);
#62912=(
GEOMETRIC_REPRESENTATION_CONTEXT(3)
GLOBAL_UNCERTAINTY_ASSIGNED_CONTEXT((#62813))
GLOBAL_UNIT_ASSIGNED_CONTEXT((#62985,#62987,#62988))
REPRESENTATION_CONTEXT('','3D')
);
#62913=(
GEOMETRIC_REPRESENTATION_CONTEXT(3)
GLOBAL_UNCERTAINTY_ASSIGNED_CONTEXT((#62814))
GLOBAL_UNIT_ASSIGNED_CONTEXT((#62985,#62987,#62988))
REPRESENTATION_CONTEXT('','3D')
);
#62914=(
GEOMETRIC_REPRESENTATION_CONTEXT(3)
GLOBAL_UNCERTAINTY_ASSIGNED_CONTEXT((#62815))
GLOBAL_UNIT_ASSIGNED_CONTEXT((#62985,#62987,#62988))
REPRESENTATION_CONTEXT('','3D')
);
#62915=(
GEOMETRIC_REPRESENTATION_CONTEXT(3)
GLOBAL_UNCERTAINTY_ASSIGNED_CONTEXT((#62816))
GLOBAL_UNIT_ASSIGNED_CONTEXT((#62985,#62987,#62988))
REPRESENTATION_CONTEXT('','3D')
);
#62916=(
GEOMETRIC_REPRESENTATION_CONTEXT(3)
GLOBAL_UNCERTAINTY_ASSIGNED_CONTEXT((#62817))
GLOBAL_UNIT_ASSIGNED_CONTEXT((#62985,#62987,#62988))
REPRESENTATION_CONTEXT('','3D')
);
#62917=(
GEOMETRIC_REPRESENTATION_CONTEXT(3)
GLOBAL_UNCERTAINTY_ASSIGNED_CONTEXT((#62818))
GLOBAL_UNIT_ASSIGNED_CONTEXT((#62985,#62987,#62988))
REPRESENTATION_CONTEXT('','3D')
);
#62918=(
GEOMETRIC_REPRESENTATION_CONTEXT(3)
GLOBAL_UNCERTAINTY_ASSIGNED_CONTEXT((#62819))
GLOBAL_UNIT_ASSIGNED_CONTEXT((#62985,#62987,#62988))
REPRESENTATION_CONTEXT('','3D')
);
#62919=(
GEOMETRIC_REPRESENTATION_CONTEXT(3)
GLOBAL_UNCERTAINTY_ASSIGNED_CONTEXT((#62820))
GLOBAL_UNIT_ASSIGNED_CONTEXT((#62985,#62987,#62988))
REPRESENTATION_CONTEXT('','3D')
);
#62920=(
GEOMETRIC_REPRESENTATION_CONTEXT(3)
GLOBAL_UNCERTAINTY_ASSIGNED_CONTEXT((#62821))
GLOBAL_UNIT_ASSIGNED_CONTEXT((#62985,#62987,#62988))
REPRESENTATION_CONTEXT('','3D')
);
#62921=(
GEOMETRIC_REPRESENTATION_CONTEXT(3)
GLOBAL_UNCERTAINTY_ASSIGNED_CONTEXT((#62822))
GLOBAL_UNIT_ASSIGNED_CONTEXT((#62985,#62987,#62988))
REPRESENTATION_CONTEXT('','3D')
);
#62922=(
GEOMETRIC_REPRESENTATION_CONTEXT(3)
GLOBAL_UNCERTAINTY_ASSIGNED_CONTEXT((#62823))
GLOBAL_UNIT_ASSIGNED_CONTEXT((#62985,#62987,#62988))
REPRESENTATION_CONTEXT('','3D')
);
#62923=(
GEOMETRIC_REPRESENTATION_CONTEXT(3)
GLOBAL_UNCERTAINTY_ASSIGNED_CONTEXT((#62824))
GLOBAL_UNIT_ASSIGNED_CONTEXT((#62985,#62987,#62988))
REPRESENTATION_CONTEXT('','3D')
);
#62924=(
GEOMETRIC_REPRESENTATION_CONTEXT(3)
GLOBAL_UNCERTAINTY_ASSIGNED_CONTEXT((#62825))
GLOBAL_UNIT_ASSIGNED_CONTEXT((#62985,#62987,#62988))
REPRESENTATION_CONTEXT('','3D')
);
#62925=(
GEOMETRIC_REPRESENTATION_CONTEXT(3)
GLOBAL_UNCERTAINTY_ASSIGNED_CONTEXT((#62826))
GLOBAL_UNIT_ASSIGNED_CONTEXT((#62985,#62987,#62988))
REPRESENTATION_CONTEXT('','3D')
);
#62926=(
GEOMETRIC_REPRESENTATION_CONTEXT(3)
GLOBAL_UNCERTAINTY_ASSIGNED_CONTEXT((#62827))
GLOBAL_UNIT_ASSIGNED_CONTEXT((#62985,#62987,#62988))
REPRESENTATION_CONTEXT('','3D')
);
#62927=(
GEOMETRIC_REPRESENTATION_CONTEXT(3)
GLOBAL_UNCERTAINTY_ASSIGNED_CONTEXT((#62828))
GLOBAL_UNIT_ASSIGNED_CONTEXT((#62985,#62987,#62988))
REPRESENTATION_CONTEXT('','3D')
);
#62928=(
GEOMETRIC_REPRESENTATION_CONTEXT(3)
GLOBAL_UNCERTAINTY_ASSIGNED_CONTEXT((#62829))
GLOBAL_UNIT_ASSIGNED_CONTEXT((#62985,#62987,#62988))
REPRESENTATION_CONTEXT('','3D')
);
#62929=(
GEOMETRIC_REPRESENTATION_CONTEXT(3)
GLOBAL_UNCERTAINTY_ASSIGNED_CONTEXT((#62830))
GLOBAL_UNIT_ASSIGNED_CONTEXT((#62985,#62987,#62988))
REPRESENTATION_CONTEXT('','3D')
);
#62930=(
GEOMETRIC_REPRESENTATION_CONTEXT(3)
GLOBAL_UNCERTAINTY_ASSIGNED_CONTEXT((#62831))
GLOBAL_UNIT_ASSIGNED_CONTEXT((#62985,#62987,#62988))
REPRESENTATION_CONTEXT('','3D')
);
#62931=(
GEOMETRIC_REPRESENTATION_CONTEXT(3)
GLOBAL_UNCERTAINTY_ASSIGNED_CONTEXT((#62832))
GLOBAL_UNIT_ASSIGNED_CONTEXT((#62985,#62987,#62988))
REPRESENTATION_CONTEXT('','3D')
);
#62932=(
GEOMETRIC_REPRESENTATION_CONTEXT(3)
GLOBAL_UNCERTAINTY_ASSIGNED_CONTEXT((#62833))
GLOBAL_UNIT_ASSIGNED_CONTEXT((#62985,#62987,#62988))
REPRESENTATION_CONTEXT('','3D')
);
#62933=(
GEOMETRIC_REPRESENTATION_CONTEXT(3)
GLOBAL_UNCERTAINTY_ASSIGNED_CONTEXT((#62834))
GLOBAL_UNIT_ASSIGNED_CONTEXT((#62985,#62987,#62988))
REPRESENTATION_CONTEXT('','3D')
);
#62934=(
GEOMETRIC_REPRESENTATION_CONTEXT(3)
GLOBAL_UNCERTAINTY_ASSIGNED_CONTEXT((#62835))
GLOBAL_UNIT_ASSIGNED_CONTEXT((#62985,#62987,#62988))
REPRESENTATION_CONTEXT('','3D')
);
#62935=(
GEOMETRIC_REPRESENTATION_CONTEXT(3)
GLOBAL_UNCERTAINTY_ASSIGNED_CONTEXT((#62836))
GLOBAL_UNIT_ASSIGNED_CONTEXT((#62985,#62987,#62988))
REPRESENTATION_CONTEXT('','3D')
);
#62936=(
GEOMETRIC_REPRESENTATION_CONTEXT(3)
GLOBAL_UNCERTAINTY_ASSIGNED_CONTEXT((#62837))
GLOBAL_UNIT_ASSIGNED_CONTEXT((#62985,#62987,#62988))
REPRESENTATION_CONTEXT('','3D')
);
#62937=(
GEOMETRIC_REPRESENTATION_CONTEXT(3)
GLOBAL_UNCERTAINTY_ASSIGNED_CONTEXT((#62838))
GLOBAL_UNIT_ASSIGNED_CONTEXT((#62985,#62987,#62988))
REPRESENTATION_CONTEXT('','3D')
);
#62938=(
GEOMETRIC_REPRESENTATION_CONTEXT(3)
GLOBAL_UNCERTAINTY_ASSIGNED_CONTEXT((#62839))
GLOBAL_UNIT_ASSIGNED_CONTEXT((#62985,#62987,#62988))
REPRESENTATION_CONTEXT('','3D')
);
#62939=(
GEOMETRIC_REPRESENTATION_CONTEXT(3)
GLOBAL_UNCERTAINTY_ASSIGNED_CONTEXT((#62840))
GLOBAL_UNIT_ASSIGNED_CONTEXT((#62985,#62987,#62988))
REPRESENTATION_CONTEXT('','3D')
);
#62940=(
GEOMETRIC_REPRESENTATION_CONTEXT(3)
GLOBAL_UNCERTAINTY_ASSIGNED_CONTEXT((#62841))
GLOBAL_UNIT_ASSIGNED_CONTEXT((#62985,#62987,#62988))
REPRESENTATION_CONTEXT('','3D')
);
#62941=(
GEOMETRIC_REPRESENTATION_CONTEXT(3)
GLOBAL_UNCERTAINTY_ASSIGNED_CONTEXT((#62842))
GLOBAL_UNIT_ASSIGNED_CONTEXT((#62985,#62987,#62988))
REPRESENTATION_CONTEXT('','3D')
);
#62942=(
GEOMETRIC_REPRESENTATION_CONTEXT(3)
GLOBAL_UNCERTAINTY_ASSIGNED_CONTEXT((#62843))
GLOBAL_UNIT_ASSIGNED_CONTEXT((#62985,#62987,#62988))
REPRESENTATION_CONTEXT('','3D')
);
#62943=(
GEOMETRIC_REPRESENTATION_CONTEXT(3)
GLOBAL_UNCERTAINTY_ASSIGNED_CONTEXT((#62844))
GLOBAL_UNIT_ASSIGNED_CONTEXT((#62985,#62987,#62988))
REPRESENTATION_CONTEXT('','3D')
);
#62944=(
GEOMETRIC_REPRESENTATION_CONTEXT(3)
GLOBAL_UNCERTAINTY_ASSIGNED_CONTEXT((#62845))
GLOBAL_UNIT_ASSIGNED_CONTEXT((#62985,#62987,#62988))
REPRESENTATION_CONTEXT('','3D')
);
#62945=(
GEOMETRIC_REPRESENTATION_CONTEXT(3)
GLOBAL_UNCERTAINTY_ASSIGNED_CONTEXT((#62846))
GLOBAL_UNIT_ASSIGNED_CONTEXT((#62985,#62987,#62988))
REPRESENTATION_CONTEXT('','3D')
);
#62946=(
GEOMETRIC_REPRESENTATION_CONTEXT(3)
GLOBAL_UNCERTAINTY_ASSIGNED_CONTEXT((#62847))
GLOBAL_UNIT_ASSIGNED_CONTEXT((#62985,#62987,#62988))
REPRESENTATION_CONTEXT('','3D')
);
#62947=(
GEOMETRIC_REPRESENTATION_CONTEXT(3)
GLOBAL_UNCERTAINTY_ASSIGNED_CONTEXT((#62848))
GLOBAL_UNIT_ASSIGNED_CONTEXT((#62985,#62987,#62988))
REPRESENTATION_CONTEXT('','3D')
);
#62948=(
GEOMETRIC_REPRESENTATION_CONTEXT(3)
GLOBAL_UNCERTAINTY_ASSIGNED_CONTEXT((#62849))
GLOBAL_UNIT_ASSIGNED_CONTEXT((#62985,#62987,#62988))
REPRESENTATION_CONTEXT('','3D')
);
#62949=(
GEOMETRIC_REPRESENTATION_CONTEXT(3)
GLOBAL_UNCERTAINTY_ASSIGNED_CONTEXT((#62850))
GLOBAL_UNIT_ASSIGNED_CONTEXT((#62985,#62987,#62988))
REPRESENTATION_CONTEXT('','3D')
);
#62950=(
GEOMETRIC_REPRESENTATION_CONTEXT(3)
GLOBAL_UNCERTAINTY_ASSIGNED_CONTEXT((#62851))
GLOBAL_UNIT_ASSIGNED_CONTEXT((#62985,#62987,#62988))
REPRESENTATION_CONTEXT('','3D')
);
#62951=(
GEOMETRIC_REPRESENTATION_CONTEXT(3)
GLOBAL_UNCERTAINTY_ASSIGNED_CONTEXT((#62852))
GLOBAL_UNIT_ASSIGNED_CONTEXT((#62985,#62987,#62988))
REPRESENTATION_CONTEXT('','3D')
);
#62952=(
GEOMETRIC_REPRESENTATION_CONTEXT(3)
GLOBAL_UNCERTAINTY_ASSIGNED_CONTEXT((#62853))
GLOBAL_UNIT_ASSIGNED_CONTEXT((#62985,#62987,#62988))
REPRESENTATION_CONTEXT('','3D')
);
#62953=(
GEOMETRIC_REPRESENTATION_CONTEXT(3)
GLOBAL_UNCERTAINTY_ASSIGNED_CONTEXT((#62854))
GLOBAL_UNIT_ASSIGNED_CONTEXT((#62985,#62987,#62988))
REPRESENTATION_CONTEXT('','3D')
);
#62954=(
GEOMETRIC_REPRESENTATION_CONTEXT(3)
GLOBAL_UNCERTAINTY_ASSIGNED_CONTEXT((#62855))
GLOBAL_UNIT_ASSIGNED_CONTEXT((#62985,#62987,#62988))
REPRESENTATION_CONTEXT('','3D')
);
#62955=(
GEOMETRIC_REPRESENTATION_CONTEXT(3)
GLOBAL_UNCERTAINTY_ASSIGNED_CONTEXT((#62856))
GLOBAL_UNIT_ASSIGNED_CONTEXT((#62985,#62987,#62988))
REPRESENTATION_CONTEXT('','3D')
);
#62956=(
GEOMETRIC_REPRESENTATION_CONTEXT(3)
GLOBAL_UNCERTAINTY_ASSIGNED_CONTEXT((#62857))
GLOBAL_UNIT_ASSIGNED_CONTEXT((#62985,#62987,#62988))
REPRESENTATION_CONTEXT('','3D')
);
#62957=(
GEOMETRIC_REPRESENTATION_CONTEXT(3)
GLOBAL_UNCERTAINTY_ASSIGNED_CONTEXT((#62858))
GLOBAL_UNIT_ASSIGNED_CONTEXT((#62985,#62987,#62988))
REPRESENTATION_CONTEXT('','3D')
);
#62958=(
GEOMETRIC_REPRESENTATION_CONTEXT(3)
GLOBAL_UNCERTAINTY_ASSIGNED_CONTEXT((#62859))
GLOBAL_UNIT_ASSIGNED_CONTEXT((#62985,#62987,#62988))
REPRESENTATION_CONTEXT('','3D')
);
#62959=(
GEOMETRIC_REPRESENTATION_CONTEXT(3)
GLOBAL_UNCERTAINTY_ASSIGNED_CONTEXT((#62860))
GLOBAL_UNIT_ASSIGNED_CONTEXT((#62985,#62987,#62988))
REPRESENTATION_CONTEXT('','3D')
);
#62960=(
GEOMETRIC_REPRESENTATION_CONTEXT(3)
GLOBAL_UNCERTAINTY_ASSIGNED_CONTEXT((#62861))
GLOBAL_UNIT_ASSIGNED_CONTEXT((#62985,#62987,#62988))
REPRESENTATION_CONTEXT('','3D')
);
#62961=(
GEOMETRIC_REPRESENTATION_CONTEXT(3)
GLOBAL_UNCERTAINTY_ASSIGNED_CONTEXT((#62862))
GLOBAL_UNIT_ASSIGNED_CONTEXT((#62985,#62987,#62988))
REPRESENTATION_CONTEXT('','3D')
);
#62962=(
GEOMETRIC_REPRESENTATION_CONTEXT(3)
GLOBAL_UNCERTAINTY_ASSIGNED_CONTEXT((#62863))
GLOBAL_UNIT_ASSIGNED_CONTEXT((#62985,#62987,#62988))
REPRESENTATION_CONTEXT('','3D')
);
#62963=(
GEOMETRIC_REPRESENTATION_CONTEXT(3)
GLOBAL_UNCERTAINTY_ASSIGNED_CONTEXT((#62864))
GLOBAL_UNIT_ASSIGNED_CONTEXT((#62985,#62987,#62988))
REPRESENTATION_CONTEXT('','3D')
);
#62964=(
GEOMETRIC_REPRESENTATION_CONTEXT(3)
GLOBAL_UNCERTAINTY_ASSIGNED_CONTEXT((#62865))
GLOBAL_UNIT_ASSIGNED_CONTEXT((#62985,#62987,#62988))
REPRESENTATION_CONTEXT('','3D')
);
#62965=(
GEOMETRIC_REPRESENTATION_CONTEXT(3)
GLOBAL_UNCERTAINTY_ASSIGNED_CONTEXT((#62866))
GLOBAL_UNIT_ASSIGNED_CONTEXT((#62985,#62987,#62988))
REPRESENTATION_CONTEXT('','3D')
);
#62966=(
GEOMETRIC_REPRESENTATION_CONTEXT(3)
GLOBAL_UNCERTAINTY_ASSIGNED_CONTEXT((#62867))
GLOBAL_UNIT_ASSIGNED_CONTEXT((#62985,#62987,#62988))
REPRESENTATION_CONTEXT('','3D')
);
#62967=(
GEOMETRIC_REPRESENTATION_CONTEXT(3)
GLOBAL_UNCERTAINTY_ASSIGNED_CONTEXT((#62868))
GLOBAL_UNIT_ASSIGNED_CONTEXT((#62985,#62987,#62988))
REPRESENTATION_CONTEXT('','3D')
);
#62968=(
GEOMETRIC_REPRESENTATION_CONTEXT(3)
GLOBAL_UNCERTAINTY_ASSIGNED_CONTEXT((#62869))
GLOBAL_UNIT_ASSIGNED_CONTEXT((#62985,#62987,#62988))
REPRESENTATION_CONTEXT('','3D')
);
#62969=(
GEOMETRIC_REPRESENTATION_CONTEXT(3)
GLOBAL_UNCERTAINTY_ASSIGNED_CONTEXT((#62870))
GLOBAL_UNIT_ASSIGNED_CONTEXT((#62985,#62987,#62988))
REPRESENTATION_CONTEXT('','3D')
);
#62970=(
GEOMETRIC_REPRESENTATION_CONTEXT(3)
GLOBAL_UNCERTAINTY_ASSIGNED_CONTEXT((#62871))
GLOBAL_UNIT_ASSIGNED_CONTEXT((#62985,#62987,#62988))
REPRESENTATION_CONTEXT('','3D')
);
#62971=(
GEOMETRIC_REPRESENTATION_CONTEXT(3)
GLOBAL_UNCERTAINTY_ASSIGNED_CONTEXT((#62872))
GLOBAL_UNIT_ASSIGNED_CONTEXT((#62985,#62987,#62988))
REPRESENTATION_CONTEXT('','3D')
);
#62972=(
GEOMETRIC_REPRESENTATION_CONTEXT(3)
GLOBAL_UNCERTAINTY_ASSIGNED_CONTEXT((#62873))
GLOBAL_UNIT_ASSIGNED_CONTEXT((#62985,#62987,#62988))
REPRESENTATION_CONTEXT('','3D')
);
#62973=(
GEOMETRIC_REPRESENTATION_CONTEXT(3)
GLOBAL_UNCERTAINTY_ASSIGNED_CONTEXT((#62874))
GLOBAL_UNIT_ASSIGNED_CONTEXT((#62985,#62987,#62988))
REPRESENTATION_CONTEXT('','3D')
);
#62974=(
GEOMETRIC_REPRESENTATION_CONTEXT(3)
GLOBAL_UNCERTAINTY_ASSIGNED_CONTEXT((#62875))
GLOBAL_UNIT_ASSIGNED_CONTEXT((#62985,#62987,#62988))
REPRESENTATION_CONTEXT('','3D')
);
#62975=(
GEOMETRIC_REPRESENTATION_CONTEXT(3)
GLOBAL_UNCERTAINTY_ASSIGNED_CONTEXT((#62876))
GLOBAL_UNIT_ASSIGNED_CONTEXT((#62985,#62987,#62988))
REPRESENTATION_CONTEXT('','3D')
);
#62976=(
GEOMETRIC_REPRESENTATION_CONTEXT(3)
GLOBAL_UNCERTAINTY_ASSIGNED_CONTEXT((#62877))
GLOBAL_UNIT_ASSIGNED_CONTEXT((#62985,#62987,#62988))
REPRESENTATION_CONTEXT('','3D')
);
#62977=(
GEOMETRIC_REPRESENTATION_CONTEXT(3)
GLOBAL_UNCERTAINTY_ASSIGNED_CONTEXT((#62878))
GLOBAL_UNIT_ASSIGNED_CONTEXT((#62985,#62987,#62988))
REPRESENTATION_CONTEXT('','3D')
);
#62978=(
GEOMETRIC_REPRESENTATION_CONTEXT(3)
GLOBAL_UNCERTAINTY_ASSIGNED_CONTEXT((#62879))
GLOBAL_UNIT_ASSIGNED_CONTEXT((#62985,#62987,#62988))
REPRESENTATION_CONTEXT('','3D')
);
#62979=(
GEOMETRIC_REPRESENTATION_CONTEXT(3)
GLOBAL_UNCERTAINTY_ASSIGNED_CONTEXT((#62880))
GLOBAL_UNIT_ASSIGNED_CONTEXT((#62985,#62987,#62988))
REPRESENTATION_CONTEXT('','3D')
);
#62980=(
GEOMETRIC_REPRESENTATION_CONTEXT(3)
GLOBAL_UNCERTAINTY_ASSIGNED_CONTEXT((#62881))
GLOBAL_UNIT_ASSIGNED_CONTEXT((#62985,#62987,#62988))
REPRESENTATION_CONTEXT('','3D')
);
#62981=(
GEOMETRIC_REPRESENTATION_CONTEXT(3)
GLOBAL_UNCERTAINTY_ASSIGNED_CONTEXT((#62882))
GLOBAL_UNIT_ASSIGNED_CONTEXT((#62985,#62987,#62988))
REPRESENTATION_CONTEXT('','3D')
);
#62982=(
GEOMETRIC_REPRESENTATION_CONTEXT(3)
GLOBAL_UNCERTAINTY_ASSIGNED_CONTEXT((#62883))
GLOBAL_UNIT_ASSIGNED_CONTEXT((#62985,#62987,#62988))
REPRESENTATION_CONTEXT('','3D')
);
#62983=(
GEOMETRIC_REPRESENTATION_CONTEXT(3)
GLOBAL_UNCERTAINTY_ASSIGNED_CONTEXT((#62884))
GLOBAL_UNIT_ASSIGNED_CONTEXT((#62985,#62987,#62988))
REPRESENTATION_CONTEXT('','3D')
);
#62984=(
GEOMETRIC_REPRESENTATION_CONTEXT(3)
GLOBAL_UNCERTAINTY_ASSIGNED_CONTEXT((#62885))
GLOBAL_UNIT_ASSIGNED_CONTEXT((#62985,#62987,#62988))
REPRESENTATION_CONTEXT('','3D')
);
#62985=(
LENGTH_UNIT()
NAMED_UNIT(*)
SI_UNIT(.CENTI.,.METRE.)
);
#62986=(
LENGTH_UNIT()
NAMED_UNIT(*)
SI_UNIT($,.METRE.)
);
#62987=(
NAMED_UNIT(*)
PLANE_ANGLE_UNIT()
SI_UNIT($,.RADIAN.)
);
#62988=(
NAMED_UNIT(*)
SI_UNIT($,.STERADIAN.)
SOLID_ANGLE_UNIT()
);
#62989=SHAPE_DEFINITION_REPRESENTATION(#63087,#63349);
#62990=SHAPE_DEFINITION_REPRESENTATION(#63088,#63350);
#62991=SHAPE_DEFINITION_REPRESENTATION(#63089,#63351);
#62992=SHAPE_DEFINITION_REPRESENTATION(#63090,#63352);
#62993=SHAPE_DEFINITION_REPRESENTATION(#63091,#63353);
#62994=SHAPE_DEFINITION_REPRESENTATION(#63092,#63354);
#62995=SHAPE_DEFINITION_REPRESENTATION(#63093,#63355);
#62996=SHAPE_DEFINITION_REPRESENTATION(#63094,#63356);
#62997=SHAPE_DEFINITION_REPRESENTATION(#63095,#63357);
#62998=SHAPE_DEFINITION_REPRESENTATION(#63096,#63358);
#62999=SHAPE_DEFINITION_REPRESENTATION(#63097,#63359);
#63000=SHAPE_DEFINITION_REPRESENTATION(#63098,#63360);
#63001=SHAPE_DEFINITION_REPRESENTATION(#63099,#63361);
#63002=SHAPE_DEFINITION_REPRESENTATION(#63100,#63362);
#63003=SHAPE_DEFINITION_REPRESENTATION(#63101,#63363);
#63004=SHAPE_DEFINITION_REPRESENTATION(#63102,#63364);
#63005=SHAPE_DEFINITION_REPRESENTATION(#63103,#63365);
#63006=SHAPE_DEFINITION_REPRESENTATION(#63104,#63366);
#63007=SHAPE_DEFINITION_REPRESENTATION(#63105,#63367);
#63008=SHAPE_DEFINITION_REPRESENTATION(#63106,#63368);
#63009=SHAPE_DEFINITION_REPRESENTATION(#63112,#63369);
#63010=SHAPE_DEFINITION_REPRESENTATION(#63113,#63370);
#63011=SHAPE_DEFINITION_REPRESENTATION(#63114,#63371);
#63012=SHAPE_DEFINITION_REPRESENTATION(#63115,#63372);
#63013=SHAPE_DEFINITION_REPRESENTATION(#63116,#63373);
#63014=SHAPE_DEFINITION_REPRESENTATION(#63117,#63374);
#63015=SHAPE_DEFINITION_REPRESENTATION(#63123,#63375);
#63016=SHAPE_DEFINITION_REPRESENTATION(#63124,#63376);
#63017=SHAPE_DEFINITION_REPRESENTATION(#63125,#63377);
#63018=SHAPE_DEFINITION_REPRESENTATION(#63126,#63378);
#63019=SHAPE_DEFINITION_REPRESENTATION(#63127,#63379);
#63020=SHAPE_DEFINITION_REPRESENTATION(#63128,#63380);
#63021=SHAPE_DEFINITION_REPRESENTATION(#63129,#63381);
#63022=SHAPE_DEFINITION_REPRESENTATION(#63130,#63382);
#63023=SHAPE_DEFINITION_REPRESENTATION(#63134,#63383);
#63024=SHAPE_DEFINITION_REPRESENTATION(#63135,#63384);
#63025=SHAPE_DEFINITION_REPRESENTATION(#63136,#63385);
#63026=SHAPE_DEFINITION_REPRESENTATION(#63137,#63386);
#63027=SHAPE_DEFINITION_REPRESENTATION(#63138,#63387);
#63028=SHAPE_DEFINITION_REPRESENTATION(#63159,#63388);
#63029=SHAPE_DEFINITION_REPRESENTATION(#63160,#63389);
#63030=SHAPE_DEFINITION_REPRESENTATION(#63161,#63390);
#63031=SHAPE_DEFINITION_REPRESENTATION(#63162,#63391);
#63032=SHAPE_DEFINITION_REPRESENTATION(#63163,#63392);
#63033=SHAPE_DEFINITION_REPRESENTATION(#63164,#63393);
#63034=SHAPE_DEFINITION_REPRESENTATION(#63165,#63394);
#63035=SHAPE_DEFINITION_REPRESENTATION(#63166,#63395);
#63036=SHAPE_DEFINITION_REPRESENTATION(#63167,#63396);
#63037=SHAPE_DEFINITION_REPRESENTATION(#63168,#63397);
#63038=SHAPE_DEFINITION_REPRESENTATION(#63169,#63398);
#63039=SHAPE_DEFINITION_REPRESENTATION(#63217,#63399);
#63040=SHAPE_DEFINITION_REPRESENTATION(#63218,#63400);
#63041=SHAPE_DEFINITION_REPRESENTATION(#63219,#63401);
#63042=SHAPE_DEFINITION_REPRESENTATION(#63220,#63402);
#63043=SHAPE_DEFINITION_REPRESENTATION(#63221,#63403);
#63044=SHAPE_DEFINITION_REPRESENTATION(#63222,#63404);
#63045=SHAPE_DEFINITION_REPRESENTATION(#63223,#63405);
#63046=SHAPE_DEFINITION_REPRESENTATION(#63224,#63406);
#63047=SHAPE_DEFINITION_REPRESENTATION(#63225,#63407);
#63048=SHAPE_DEFINITION_REPRESENTATION(#63226,#63408);
#63049=SHAPE_DEFINITION_REPRESENTATION(#63227,#63409);
#63050=SHAPE_DEFINITION_REPRESENTATION(#63228,#63410);
#63051=SHAPE_DEFINITION_REPRESENTATION(#63229,#63411);
#63052=SHAPE_DEFINITION_REPRESENTATION(#63230,#63412);
#63053=SHAPE_DEFINITION_REPRESENTATION(#63231,#63413);
#63054=SHAPE_DEFINITION_REPRESENTATION(#63232,#63414);
#63055=SHAPE_DEFINITION_REPRESENTATION(#63233,#63415);
#63056=SHAPE_DEFINITION_REPRESENTATION(#63239,#63416);
#63057=SHAPE_DEFINITION_REPRESENTATION(#63240,#63417);
#63058=SHAPE_DEFINITION_REPRESENTATION(#63241,#63418);
#63059=SHAPE_DEFINITION_REPRESENTATION(#63242,#63419);
#63060=SHAPE_DEFINITION_REPRESENTATION(#63243,#63420);
#63061=SHAPE_DEFINITION_REPRESENTATION(#63244,#63421);
#63062=SHAPE_DEFINITION_REPRESENTATION(#63250,#63422);
#63063=SHAPE_DEFINITION_REPRESENTATION(#63251,#63423);
#63064=SHAPE_DEFINITION_REPRESENTATION(#63252,#63424);
#63065=SHAPE_DEFINITION_REPRESENTATION(#63253,#63425);
#63066=SHAPE_DEFINITION_REPRESENTATION(#63254,#63426);
#63067=SHAPE_DEFINITION_REPRESENTATION(#63255,#63427);
#63068=SHAPE_DEFINITION_REPRESENTATION(#63256,#63428);
#63069=SHAPE_DEFINITION_REPRESENTATION(#63257,#63429);
#63070=SHAPE_DEFINITION_REPRESENTATION(#63258,#63430);
#63071=SHAPE_DEFINITION_REPRESENTATION(#63262,#63431);
#63072=SHAPE_DEFINITION_REPRESENTATION(#63263,#63432);
#63073=SHAPE_DEFINITION_REPRESENTATION(#63264,#63433);
#63074=SHAPE_DEFINITION_REPRESENTATION(#63265,#63434);
#63075=SHAPE_DEFINITION_REPRESENTATION(#63266,#63435);
#63076=SHAPE_DEFINITION_REPRESENTATION(#63287,#63436);
#63077=SHAPE_DEFINITION_REPRESENTATION(#63288,#63437);
#63078=SHAPE_DEFINITION_REPRESENTATION(#63289,#63438);
#63079=SHAPE_DEFINITION_REPRESENTATION(#63290,#63439);
#63080=SHAPE_DEFINITION_REPRESENTATION(#63291,#63440);
#63081=SHAPE_DEFINITION_REPRESENTATION(#63292,#63441);
#63082=SHAPE_DEFINITION_REPRESENTATION(#63293,#63442);
#63083=SHAPE_DEFINITION_REPRESENTATION(#63294,#63443);
#63084=SHAPE_DEFINITION_REPRESENTATION(#63295,#63444);
#63085=SHAPE_DEFINITION_REPRESENTATION(#63296,#63445);
#63086=SHAPE_DEFINITION_REPRESENTATION(#63297,#63446);
#63087=PRODUCT_DEFINITION_SHAPE('',$,#63448);
#63088=PRODUCT_DEFINITION_SHAPE('',$,#63449);
#63089=PRODUCT_DEFINITION_SHAPE('',$,#63450);
#63090=PRODUCT_DEFINITION_SHAPE('',$,#63451);
#63091=PRODUCT_DEFINITION_SHAPE('',$,#63452);
#63092=PRODUCT_DEFINITION_SHAPE('',$,#63453);
#63093=PRODUCT_DEFINITION_SHAPE('',$,#63454);
#63094=PRODUCT_DEFINITION_SHAPE('',$,#63455);
#63095=PRODUCT_DEFINITION_SHAPE('',$,#63456);
#63096=PRODUCT_DEFINITION_SHAPE('',$,#63457);
#63097=PRODUCT_DEFINITION_SHAPE('',$,#63458);
#63098=PRODUCT_DEFINITION_SHAPE('',$,#63459);
#63099=PRODUCT_DEFINITION_SHAPE('',$,#63460);
#63100=PRODUCT_DEFINITION_SHAPE('',$,#63461);
#63101=PRODUCT_DEFINITION_SHAPE('',$,#63462);
#63102=PRODUCT_DEFINITION_SHAPE('',$,#63463);
#63103=PRODUCT_DEFINITION_SHAPE('',$,#63464);
#63104=PRODUCT_DEFINITION_SHAPE('',$,#63465);
#63105=PRODUCT_DEFINITION_SHAPE('',$,#63466);
#63106=PRODUCT_DEFINITION_SHAPE('',$,#63467);
#63107=PRODUCT_DEFINITION_SHAPE($,$,#529);
#63108=PRODUCT_DEFINITION_SHAPE($,$,#530);
#63109=PRODUCT_DEFINITION_SHAPE($,$,#531);
#63110=PRODUCT_DEFINITION_SHAPE($,$,#532);
#63111=PRODUCT_DEFINITION_SHAPE($,$,#533);
#63112=PRODUCT_DEFINITION_SHAPE('',$,#63468);
#63113=PRODUCT_DEFINITION_SHAPE('',$,#63469);
#63114=PRODUCT_DEFINITION_SHAPE('',$,#63470);
#63115=PRODUCT_DEFINITION_SHAPE('',$,#63471);
#63116=PRODUCT_DEFINITION_SHAPE('',$,#63472);
#63117=PRODUCT_DEFINITION_SHAPE('',$,#63473);
#63118=PRODUCT_DEFINITION_SHAPE($,$,#534);
#63119=PRODUCT_DEFINITION_SHAPE($,$,#535);
#63120=PRODUCT_DEFINITION_SHAPE($,$,#536);
#63121=PRODUCT_DEFINITION_SHAPE($,$,#537);
#63122=PRODUCT_DEFINITION_SHAPE($,$,#538);
#63123=PRODUCT_DEFINITION_SHAPE('',$,#63474);
#63124=PRODUCT_DEFINITION_SHAPE('',$,#63475);
#63125=PRODUCT_DEFINITION_SHAPE('',$,#63476);
#63126=PRODUCT_DEFINITION_SHAPE('',$,#63477);
#63127=PRODUCT_DEFINITION_SHAPE('',$,#63478);
#63128=PRODUCT_DEFINITION_SHAPE('',$,#63479);
#63129=PRODUCT_DEFINITION_SHAPE('',$,#63480);
#63130=PRODUCT_DEFINITION_SHAPE('',$,#63481);
#63131=PRODUCT_DEFINITION_SHAPE($,$,#539);
#63132=PRODUCT_DEFINITION_SHAPE($,$,#540);
#63133=PRODUCT_DEFINITION_SHAPE($,$,#541);
#63134=PRODUCT_DEFINITION_SHAPE('',$,#63482);
#63135=PRODUCT_DEFINITION_SHAPE('',$,#63483);
#63136=PRODUCT_DEFINITION_SHAPE('',$,#63484);
#63137=PRODUCT_DEFINITION_SHAPE('',$,#63485);
#63138=PRODUCT_DEFINITION_SHAPE('',$,#63486);
#63139=PRODUCT_DEFINITION_SHAPE($,$,#542);
#63140=PRODUCT_DEFINITION_SHAPE($,$,#543);
#63141=PRODUCT_DEFINITION_SHAPE($,$,#544);
#63142=PRODUCT_DEFINITION_SHAPE($,$,#545);
#63143=PRODUCT_DEFINITION_SHAPE($,$,#546);
#63144=PRODUCT_DEFINITION_SHAPE($,$,#547);
#63145=PRODUCT_DEFINITION_SHAPE($,$,#548);
#63146=PRODUCT_DEFINITION_SHAPE($,$,#549);
#63147=PRODUCT_DEFINITION_SHAPE($,$,#550);
#63148=PRODUCT_DEFINITION_SHAPE($,$,#551);
#63149=PRODUCT_DEFINITION_SHAPE($,$,#552);
#63150=PRODUCT_DEFINITION_SHAPE($,$,#553);
#63151=PRODUCT_DEFINITION_SHAPE($,$,#554);
#63152=PRODUCT_DEFINITION_SHAPE($,$,#555);
#63153=PRODUCT_DEFINITION_SHAPE($,$,#556);
#63154=PRODUCT_DEFINITION_SHAPE($,$,#557);
#63155=PRODUCT_DEFINITION_SHAPE($,$,#558);
#63156=PRODUCT_DEFINITION_SHAPE($,$,#559);
#63157=PRODUCT_DEFINITION_SHAPE($,$,#560);
#63158=PRODUCT_DEFINITION_SHAPE($,$,#561);
#63159=PRODUCT_DEFINITION_SHAPE('',$,#63487);
#63160=PRODUCT_DEFINITION_SHAPE('',$,#63488);
#63161=PRODUCT_DEFINITION_SHAPE('',$,#63489);
#63162=PRODUCT_DEFINITION_SHAPE('',$,#63490);
#63163=PRODUCT_DEFINITION_SHAPE('',$,#63491);
#63164=PRODUCT_DEFINITION_SHAPE('',$,#63492);
#63165=PRODUCT_DEFINITION_SHAPE('',$,#63493);
#63166=PRODUCT_DEFINITION_SHAPE('',$,#63494);
#63167=PRODUCT_DEFINITION_SHAPE('',$,#63495);
#63168=PRODUCT_DEFINITION_SHAPE('',$,#63496);
#63169=PRODUCT_DEFINITION_SHAPE('',$,#63497);
#63170=PRODUCT_DEFINITION_SHAPE($,$,#562);
#63171=PRODUCT_DEFINITION_SHAPE($,$,#563);
#63172=PRODUCT_DEFINITION_SHAPE($,$,#564);
#63173=PRODUCT_DEFINITION_SHAPE($,$,#565);
#63174=PRODUCT_DEFINITION_SHAPE($,$,#566);
#63175=PRODUCT_DEFINITION_SHAPE($,$,#567);
#63176=PRODUCT_DEFINITION_SHAPE($,$,#568);
#63177=PRODUCT_DEFINITION_SHAPE($,$,#569);
#63178=PRODUCT_DEFINITION_SHAPE($,$,#570);
#63179=PRODUCT_DEFINITION_SHAPE($,$,#571);
#63180=PRODUCT_DEFINITION_SHAPE($,$,#572);
#63181=PRODUCT_DEFINITION_SHAPE($,$,#573);
#63182=PRODUCT_DEFINITION_SHAPE($,$,#574);
#63183=PRODUCT_DEFINITION_SHAPE($,$,#575);
#63184=PRODUCT_DEFINITION_SHAPE($,$,#576);
#63185=PRODUCT_DEFINITION_SHAPE($,$,#577);
#63186=PRODUCT_DEFINITION_SHAPE($,$,#578);
#63187=PRODUCT_DEFINITION_SHAPE($,$,#579);
#63188=PRODUCT_DEFINITION_SHAPE($,$,#580);
#63189=PRODUCT_DEFINITION_SHAPE($,$,#581);
#63190=PRODUCT_DEFINITION_SHAPE($,$,#582);
#63191=PRODUCT_DEFINITION_SHAPE($,$,#583);
#63192=PRODUCT_DEFINITION_SHAPE($,$,#584);
#63193=PRODUCT_DEFINITION_SHAPE($,$,#585);
#63194=PRODUCT_DEFINITION_SHAPE($,$,#586);
#63195=PRODUCT_DEFINITION_SHAPE($,$,#587);
#63196=PRODUCT_DEFINITION_SHAPE($,$,#588);
#63197=PRODUCT_DEFINITION_SHAPE($,$,#589);
#63198=PRODUCT_DEFINITION_SHAPE($,$,#590);
#63199=PRODUCT_DEFINITION_SHAPE($,$,#591);
#63200=PRODUCT_DEFINITION_SHAPE($,$,#592);
#63201=PRODUCT_DEFINITION_SHAPE($,$,#593);
#63202=PRODUCT_DEFINITION_SHAPE($,$,#594);
#63203=PRODUCT_DEFINITION_SHAPE($,$,#595);
#63204=PRODUCT_DEFINITION_SHAPE($,$,#596);
#63205=PRODUCT_DEFINITION_SHAPE($,$,#597);
#63206=PRODUCT_DEFINITION_SHAPE($,$,#598);
#63207=PRODUCT_DEFINITION_SHAPE($,$,#599);
#63208=PRODUCT_DEFINITION_SHAPE($,$,#600);
#63209=PRODUCT_DEFINITION_SHAPE($,$,#601);
#63210=PRODUCT_DEFINITION_SHAPE($,$,#602);
#63211=PRODUCT_DEFINITION_SHAPE($,$,#603);
#63212=PRODUCT_DEFINITION_SHAPE($,$,#604);
#63213=PRODUCT_DEFINITION_SHAPE($,$,#605);
#63214=PRODUCT_DEFINITION_SHAPE($,$,#606);
#63215=PRODUCT_DEFINITION_SHAPE($,$,#607);
#63216=PRODUCT_DEFINITION_SHAPE($,$,#608);
#63217=PRODUCT_DEFINITION_SHAPE('',$,#63498);
#63218=PRODUCT_DEFINITION_SHAPE('',$,#63499);
#63219=PRODUCT_DEFINITION_SHAPE('',$,#63500);
#63220=PRODUCT_DEFINITION_SHAPE('',$,#63501);
#63221=PRODUCT_DEFINITION_SHAPE('',$,#63502);
#63222=PRODUCT_DEFINITION_SHAPE('',$,#63503);
#63223=PRODUCT_DEFINITION_SHAPE('',$,#63504);
#63224=PRODUCT_DEFINITION_SHAPE('',$,#63505);
#63225=PRODUCT_DEFINITION_SHAPE('',$,#63506);
#63226=PRODUCT_DEFINITION_SHAPE('',$,#63507);
#63227=PRODUCT_DEFINITION_SHAPE('',$,#63508);
#63228=PRODUCT_DEFINITION_SHAPE('',$,#63509);
#63229=PRODUCT_DEFINITION_SHAPE('',$,#63510);
#63230=PRODUCT_DEFINITION_SHAPE('',$,#63511);
#63231=PRODUCT_DEFINITION_SHAPE('',$,#63512);
#63232=PRODUCT_DEFINITION_SHAPE('',$,#63513);
#63233=PRODUCT_DEFINITION_SHAPE('',$,#63514);
#63234=PRODUCT_DEFINITION_SHAPE($,$,#609);
#63235=PRODUCT_DEFINITION_SHAPE($,$,#610);
#63236=PRODUCT_DEFINITION_SHAPE($,$,#611);
#63237=PRODUCT_DEFINITION_SHAPE($,$,#612);
#63238=PRODUCT_DEFINITION_SHAPE($,$,#613);
#63239=PRODUCT_DEFINITION_SHAPE('',$,#63515);
#63240=PRODUCT_DEFINITION_SHAPE('',$,#63516);
#63241=PRODUCT_DEFINITION_SHAPE('',$,#63517);
#63242=PRODUCT_DEFINITION_SHAPE('',$,#63518);
#63243=PRODUCT_DEFINITION_SHAPE('',$,#63519);
#63244=PRODUCT_DEFINITION_SHAPE('',$,#63520);
#63245=PRODUCT_DEFINITION_SHAPE($,$,#614);
#63246=PRODUCT_DEFINITION_SHAPE($,$,#615);
#63247=PRODUCT_DEFINITION_SHAPE($,$,#616);
#63248=PRODUCT_DEFINITION_SHAPE($,$,#617);
#63249=PRODUCT_DEFINITION_SHAPE($,$,#618);
#63250=PRODUCT_DEFINITION_SHAPE('',$,#63521);
#63251=PRODUCT_DEFINITION_SHAPE('',$,#63522);
#63252=PRODUCT_DEFINITION_SHAPE('',$,#63523);
#63253=PRODUCT_DEFINITION_SHAPE('',$,#63524);
#63254=PRODUCT_DEFINITION_SHAPE('',$,#63525);
#63255=PRODUCT_DEFINITION_SHAPE('',$,#63526);
#63256=PRODUCT_DEFINITION_SHAPE('',$,#63527);
#63257=PRODUCT_DEFINITION_SHAPE('',$,#63528);
#63258=PRODUCT_DEFINITION_SHAPE('',$,#63529);
#63259=PRODUCT_DEFINITION_SHAPE($,$,#619);
#63260=PRODUCT_DEFINITION_SHAPE($,$,#620);
#63261=PRODUCT_DEFINITION_SHAPE($,$,#621);
#63262=PRODUCT_DEFINITION_SHAPE('',$,#63530);
#63263=PRODUCT_DEFINITION_SHAPE('',$,#63531);
#63264=PRODUCT_DEFINITION_SHAPE('',$,#63532);
#63265=PRODUCT_DEFINITION_SHAPE('',$,#63533);
#63266=PRODUCT_DEFINITION_SHAPE('',$,#63534);
#63267=PRODUCT_DEFINITION_SHAPE($,$,#622);
#63268=PRODUCT_DEFINITION_SHAPE($,$,#623);
#63269=PRODUCT_DEFINITION_SHAPE($,$,#624);
#63270=PRODUCT_DEFINITION_SHAPE($,$,#625);
#63271=PRODUCT_DEFINITION_SHAPE($,$,#626);
#63272=PRODUCT_DEFINITION_SHAPE($,$,#627);
#63273=PRODUCT_DEFINITION_SHAPE($,$,#628);
#63274=PRODUCT_DEFINITION_SHAPE($,$,#629);
#63275=PRODUCT_DEFINITION_SHAPE($,$,#630);
#63276=PRODUCT_DEFINITION_SHAPE($,$,#631);
#63277=PRODUCT_DEFINITION_SHAPE($,$,#632);
#63278=PRODUCT_DEFINITION_SHAPE($,$,#633);
#63279=PRODUCT_DEFINITION_SHAPE($,$,#634);
#63280=PRODUCT_DEFINITION_SHAPE($,$,#635);
#63281=PRODUCT_DEFINITION_SHAPE($,$,#636);
#63282=PRODUCT_DEFINITION_SHAPE($,$,#637);
#63283=PRODUCT_DEFINITION_SHAPE($,$,#638);
#63284=PRODUCT_DEFINITION_SHAPE($,$,#639);
#63285=PRODUCT_DEFINITION_SHAPE($,$,#640);
#63286=PRODUCT_DEFINITION_SHAPE($,$,#641);
#63287=PRODUCT_DEFINITION_SHAPE('',$,#63535);
#63288=PRODUCT_DEFINITION_SHAPE('',$,#63536);
#63289=PRODUCT_DEFINITION_SHAPE('',$,#63537);
#63290=PRODUCT_DEFINITION_SHAPE('',$,#63538);
#63291=PRODUCT_DEFINITION_SHAPE('',$,#63539);
#63292=PRODUCT_DEFINITION_SHAPE('',$,#63540);
#63293=PRODUCT_DEFINITION_SHAPE('',$,#63541);
#63294=PRODUCT_DEFINITION_SHAPE('',$,#63542);
#63295=PRODUCT_DEFINITION_SHAPE('',$,#63543);
#63296=PRODUCT_DEFINITION_SHAPE('',$,#63544);
#63297=PRODUCT_DEFINITION_SHAPE('',$,#63545);
#63298=PRODUCT_DEFINITION_SHAPE($,$,#642);
#63299=PRODUCT_DEFINITION_SHAPE($,$,#643);
#63300=PRODUCT_DEFINITION_SHAPE($,$,#644);
#63301=PRODUCT_DEFINITION_SHAPE($,$,#645);
#63302=PRODUCT_DEFINITION_SHAPE($,$,#646);
#63303=PRODUCT_DEFINITION_SHAPE($,$,#647);
#63304=PRODUCT_DEFINITION_SHAPE($,$,#648);
#63305=PRODUCT_DEFINITION_SHAPE($,$,#649);
#63306=PRODUCT_DEFINITION_SHAPE($,$,#650);
#63307=PRODUCT_DEFINITION_SHAPE($,$,#651);
#63308=PRODUCT_DEFINITION_SHAPE($,$,#652);
#63309=PRODUCT_DEFINITION_SHAPE($,$,#653);
#63310=PRODUCT_DEFINITION_SHAPE($,$,#654);
#63311=PRODUCT_DEFINITION_SHAPE($,$,#655);
#63312=PRODUCT_DEFINITION_SHAPE($,$,#656);
#63313=PRODUCT_DEFINITION_SHAPE($,$,#657);
#63314=PRODUCT_DEFINITION_SHAPE($,$,#658);
#63315=PRODUCT_DEFINITION_SHAPE($,$,#659);
#63316=PRODUCT_DEFINITION_SHAPE($,$,#660);
#63317=PRODUCT_DEFINITION_SHAPE($,$,#661);
#63318=PRODUCT_DEFINITION_SHAPE($,$,#662);
#63319=PRODUCT_DEFINITION_SHAPE($,$,#663);
#63320=PRODUCT_DEFINITION_SHAPE($,$,#664);
#63321=PRODUCT_DEFINITION_SHAPE($,$,#665);
#63322=PRODUCT_DEFINITION_SHAPE($,$,#666);
#63323=PRODUCT_DEFINITION_SHAPE($,$,#667);
#63324=PRODUCT_DEFINITION_SHAPE($,$,#668);
#63325=PRODUCT_DEFINITION_SHAPE($,$,#669);
#63326=PRODUCT_DEFINITION_SHAPE($,$,#670);
#63327=PRODUCT_DEFINITION_SHAPE($,$,#671);
#63328=PRODUCT_DEFINITION_SHAPE($,$,#672);
#63329=PRODUCT_DEFINITION_SHAPE($,$,#673);
#63330=PRODUCT_DEFINITION_SHAPE($,$,#674);
#63331=PRODUCT_DEFINITION_SHAPE($,$,#675);
#63332=PRODUCT_DEFINITION_SHAPE($,$,#676);
#63333=PRODUCT_DEFINITION_SHAPE($,$,#677);
#63334=PRODUCT_DEFINITION_SHAPE($,$,#678);
#63335=PRODUCT_DEFINITION_SHAPE($,$,#679);
#63336=PRODUCT_DEFINITION_SHAPE($,$,#680);
#63337=PRODUCT_DEFINITION_SHAPE($,$,#681);
#63338=PRODUCT_DEFINITION_SHAPE($,$,#682);
#63339=PRODUCT_DEFINITION_SHAPE($,$,#683);
#63340=PRODUCT_DEFINITION_SHAPE($,$,#684);
#63341=PRODUCT_DEFINITION_SHAPE($,$,#685);
#63342=PRODUCT_DEFINITION_SHAPE($,$,#686);
#63343=PRODUCT_DEFINITION_SHAPE($,$,#687);
#63344=PRODUCT_DEFINITION_SHAPE($,$,#688);
#63345=PRODUCT_DEFINITION_SHAPE($,$,#689);
#63346=PRODUCT_DEFINITION_SHAPE($,$,#690);
#63347=PRODUCT_DEFINITION_SHAPE($,$,#691);
#63348=PRODUCT_DEFINITION_SHAPE($,$,#692);
#63349=SHAPE_REPRESENTATION('',(#24000,#26459,#26460),#62886);
#63350=SHAPE_REPRESENTATION('',(#24001,#25197,#25198,#25199),#62887);
#63351=SHAPE_REPRESENTATION('',(#24002,#25153,#25154,#25155,#25156,#25157,
#25158,#25159,#25160,#25161,#25162,#25163,#25164,#25165,#25166,#25167,#25168,
#25169,#25170,#25171,#25172,#25173,#25174,#25175,#25176,#25177,#25178,#25179,
#25180,#25181,#25182,#25183,#25184,#25185),#62888);
#63352=SHAPE_REPRESENTATION('',(#24003),#62889);
#63353=SHAPE_REPRESENTATION('',(#24040),#62890);
#63354=SHAPE_REPRESENTATION('',(#24047),#62891);
#63355=SHAPE_REPRESENTATION('',(#24054),#62892);
#63356=SHAPE_REPRESENTATION('',(#24107),#62893);
#63357=SHAPE_REPRESENTATION('',(#24138),#62894);
#63358=SHAPE_REPRESENTATION('',(#24160),#62895);
#63359=SHAPE_REPRESENTATION('',(#24191),#62896);
#63360=SHAPE_REPRESENTATION('',(#24214),#62897);
#63361=SHAPE_REPRESENTATION('',(#24228),#62898);
#63362=SHAPE_REPRESENTATION('',(#24242),#62899);
#63363=SHAPE_REPRESENTATION('',(#24285,#24408,#24409,#24410,#24411,#24412),
#62900);
#63364=SHAPE_REPRESENTATION('',(#24286),#62901);
#63365=SHAPE_REPRESENTATION('',(#24306),#62902);
#63366=SHAPE_REPRESENTATION('',(#24326),#62903);
#63367=SHAPE_REPRESENTATION('',(#24341),#62904);
#63368=SHAPE_REPRESENTATION('',(#24391),#62905);
#63369=SHAPE_REPRESENTATION('',(#24413,#24542,#24543,#24544,#24545,#24546),
#62906);
#63370=SHAPE_REPRESENTATION('',(#24414),#62907);
#63371=SHAPE_REPRESENTATION('',(#24434),#62908);
#63372=SHAPE_REPRESENTATION('',(#24454),#62909);
#63373=SHAPE_REPRESENTATION('',(#24471),#62910);
#63374=SHAPE_REPRESENTATION('',(#24525),#62911);
#63375=SHAPE_REPRESENTATION('',(#24547,#24849,#24850,#24851,#24852,#24853,
#24854,#24855,#24856,#24857,#24858,#24859,#24860,#24861,#24862,#24863,#24864,
#24865,#24866,#24867,#24868),#62912);
#63376=SHAPE_REPRESENTATION('',(#24548),#62913);
#63377=SHAPE_REPRESENTATION('',(#24567),#62914);
#63378=SHAPE_REPRESENTATION('',(#24610),#62915);
#63379=SHAPE_REPRESENTATION('',(#24648,#24710,#24711,#24712),#62916);
#63380=SHAPE_REPRESENTATION('',(#24649),#62917);
#63381=SHAPE_REPRESENTATION('',(#24688),#62918);
#63382=SHAPE_REPRESENTATION('',(#24699),#62919);
#63383=SHAPE_REPRESENTATION('',(#24713),#62920);
#63384=SHAPE_REPRESENTATION('',(#24724),#62921);
#63385=SHAPE_REPRESENTATION('',(#24752),#62922);
#63386=SHAPE_REPRESENTATION('',(#24797),#62923);
#63387=SHAPE_REPRESENTATION('',(#24823),#62924);
#63388=SHAPE_REPRESENTATION('',(#24869,#25186,#25187,#25188,#25189,#25190,
#25191,#25192,#25193,#25194,#25195,#25196),#62925);
#63389=SHAPE_REPRESENTATION('',(#24870),#62926);
#63390=SHAPE_REPRESENTATION('',(#25025),#62927);
#63391=SHAPE_REPRESENTATION('',(#25034),#62928);
#63392=SHAPE_REPRESENTATION('',(#25048),#62929);
#63393=SHAPE_REPRESENTATION('',(#25072),#62930);
#63394=SHAPE_REPRESENTATION('',(#25081),#62931);
#63395=SHAPE_REPRESENTATION('',(#25090),#62932);
#63396=SHAPE_REPRESENTATION('',(#25101),#62933);
#63397=SHAPE_REPRESENTATION('',(#25118),#62934);
#63398=SHAPE_REPRESENTATION('',(#25127),#62935);
#63399=SHAPE_REPRESENTATION('',(#25200,#26456,#26457,#26458),#62936);
#63400=SHAPE_REPRESENTATION('',(#25201,#26410,#26411,#26412,#26413,#26414,
#26415,#26416,#26417,#26418,#26419,#26420,#26421,#26422,#26423,#26424,#26425,
#26426,#26427,#26428,#26429,#26430,#26431,#26432,#26433,#26434,#26435,#26436,
#26437,#26438,#26439,#26440,#26441,#26442,#26443,#26444),#62937);
#63401=SHAPE_REPRESENTATION('',(#25202),#62938);
#63402=SHAPE_REPRESENTATION('',(#25299),#62939);
#63403=SHAPE_REPRESENTATION('',(#25352),#62940);
#63404=SHAPE_REPRESENTATION('',(#25383),#62941);
#63405=SHAPE_REPRESENTATION('',(#25405),#62942);
#63406=SHAPE_REPRESENTATION('',(#25436),#62943);
#63407=SHAPE_REPRESENTATION('',(#25459),#62944);
#63408=SHAPE_REPRESENTATION('',(#25473),#62945);
#63409=SHAPE_REPRESENTATION('',(#25487),#62946);
#63410=SHAPE_REPRESENTATION('',(#25530,#25653,#25654,#25655,#25656,#25657),
#62947);
#63411=SHAPE_REPRESENTATION('',(#25531),#62948);
#63412=SHAPE_REPRESENTATION('',(#25551),#62949);
#63413=SHAPE_REPRESENTATION('',(#25571),#62950);
#63414=SHAPE_REPRESENTATION('',(#25586),#62951);
#63415=SHAPE_REPRESENTATION('',(#25636),#62952);
#63416=SHAPE_REPRESENTATION('',(#25658,#25787,#25788,#25789,#25790,#25791),
#62953);
#63417=SHAPE_REPRESENTATION('',(#25659),#62954);
#63418=SHAPE_REPRESENTATION('',(#25679),#62955);
#63419=SHAPE_REPRESENTATION('',(#25699),#62956);
#63420=SHAPE_REPRESENTATION('',(#25716),#62957);
#63421=SHAPE_REPRESENTATION('',(#25770),#62958);
#63422=SHAPE_REPRESENTATION('',(#25792),#62959);
#63423=SHAPE_REPRESENTATION('',(#25816,#26106,#26107,#26108,#26109,#26110,
#26111,#26112,#26113,#26114,#26115,#26116,#26117,#26118,#26119,#26120,#26121,
#26122,#26123,#26124,#26125),#62960);
#63424=SHAPE_REPRESENTATION('',(#25817),#62961);
#63425=SHAPE_REPRESENTATION('',(#25836),#62962);
#63426=SHAPE_REPRESENTATION('',(#25867),#62963);
#63427=SHAPE_REPRESENTATION('',(#25905,#25967,#25968,#25969),#62964);
#63428=SHAPE_REPRESENTATION('',(#25906),#62965);
#63429=SHAPE_REPRESENTATION('',(#25945),#62966);
#63430=SHAPE_REPRESENTATION('',(#25956),#62967);
#63431=SHAPE_REPRESENTATION('',(#25970),#62968);
#63432=SHAPE_REPRESENTATION('',(#25981),#62969);
#63433=SHAPE_REPRESENTATION('',(#26009),#62970);
#63434=SHAPE_REPRESENTATION('',(#26054),#62971);
#63435=SHAPE_REPRESENTATION('',(#26080),#62972);
#63436=SHAPE_REPRESENTATION('',(#26126,#26445,#26446,#26447,#26448,#26449,
#26450,#26451,#26452,#26453,#26454,#26455),#62973);
#63437=SHAPE_REPRESENTATION('',(#26127),#62974);
#63438=SHAPE_REPRESENTATION('',(#26282),#62975);
#63439=SHAPE_REPRESENTATION('',(#26291),#62976);
#63440=SHAPE_REPRESENTATION('',(#26305),#62977);
#63441=SHAPE_REPRESENTATION('',(#26329),#62978);
#63442=SHAPE_REPRESENTATION('',(#26338),#62979);
#63443=SHAPE_REPRESENTATION('',(#26347),#62980);
#63444=SHAPE_REPRESENTATION('',(#26358),#62981);
#63445=SHAPE_REPRESENTATION('',(#26375),#62982);
#63446=SHAPE_REPRESENTATION('',(#26384),#62983);
#63447=PRODUCT_DEFINITION_CONTEXT('part definition',#63743,'design');
#63448=PRODUCT_DEFINITION('PAT-124','PAT-124',#63546,#63447);
#63449=PRODUCT_DEFINITION('X feed stage','X feed stage',#63547,#63447);
#63450=PRODUCT_DEFINITION('Rail and screw supports',
'Rail and screw supports',#63548,#63447);
#63451=PRODUCT_DEFINITION('X Stage - 02 Base','X Stage - 02 Base',#63549,
#63447);
#63452=PRODUCT_DEFINITION('X Stage - 03 Bonded skid',
'X Stage - 03 Bonded skid',#63550,#63447);
#63453=PRODUCT_DEFINITION('X Stage - 03 Bonded skid (1)',
'X Stage - 03 Bonded skid (1)',#63551,#63447);
#63454=PRODUCT_DEFINITION('X Stage - 04 Rail adapter',
'X Stage - 04 Rail adapter',#63552,#63447);
#63455=PRODUCT_DEFINITION('X Stage - 08 Floating bearing support',
'X Stage - 08 Floating bearing support',#63553,#63447);
#63456=PRODUCT_DEFINITION('X Stage - 10 Floating cap',
'X Stage - 10 Floating cap',#63554,#63447);
#63457=PRODUCT_DEFINITION('X Stage - 09 Fixed bearing support',
'X Stage - 09 Fixed bearing support',#63555,#63447);
#63458=PRODUCT_DEFINITION('X Stage - 11 Fixed cap',
'X Stage - 11 Fixed cap',#63556,#63447);
#63459=PRODUCT_DEFINITION('X Stage - 12 End stop',
'X Stage - 12 End stop',#63557,#63447);
#63460=PRODUCT_DEFINITION('X Stage - 12 End stop (1)',
'X Stage - 12 End stop (1)',#63558,#63447);
#63461=PRODUCT_DEFINITION('Linear Guide Rail - 15 mm, 220 mm Long',
'Linear Guide Rail - 15 mm, 220 mm Long',#63559,#63447);
#63462=PRODUCT_DEFINITION('Sealed Ball Bearing - 12 x 32 x 10 mm',
'Sealed Ball Bearing - 12 x 32 x 10 mm',#63560,#63447);
#63463=PRODUCT_DEFINITION('Inner ring','Inner ring',#63561,#63447);
#63464=PRODUCT_DEFINITION('Outer ring','Outer ring',#63562,#63447);
#63465=PRODUCT_DEFINITION('Balls','Balls',#63563,#63447);
#63466=PRODUCT_DEFINITION('Cage','Cage',#63564,#63447);
#63467=PRODUCT_DEFINITION('Seals 2RS','Seals 2RS',#63565,#63447);
#63468=PRODUCT_DEFINITION('Sealed Ball Bearing - 20 x 47 x 14 mm',
'Sealed Ball Bearing - 20 x 47 x 14 mm',#63566,#63447);
#63469=PRODUCT_DEFINITION('Inner ring (1)','Inner ring (1)',#63567,#63447);
#63470=PRODUCT_DEFINITION('Outer ring (1)','Outer ring (1)',#63568,#63447);
#63471=PRODUCT_DEFINITION('Balls (1)','Balls (1)',#63569,#63447);
#63472=PRODUCT_DEFINITION('Cage (1)','Cage (1)',#63570,#63447);
#63473=PRODUCT_DEFINITION('Seals 2RS (1)','Seals 2RS (1)',#63571,#63447);
#63474=PRODUCT_DEFINITION('Moving table and nut','Moving table and nut',
#63572,#63447);
#63475=PRODUCT_DEFINITION('X Stage - 05 Carriage spacer',
'X Stage - 05 Carriage spacer',#63573,#63447);
#63476=PRODUCT_DEFINITION('X Stage - 06 Table','X Stage - 06 Table',#63574,
#63447);
#63477=PRODUCT_DEFINITION('X Stage - 07 Nut bracket',
'X Stage - 07 Nut bracket',#63575,#63447);
#63478=PRODUCT_DEFINITION('Flanged Linear Guide Carriage - 15 mm',
'Flanged Linear Guide Carriage - 15 mm',#63576,#63447);
#63479=PRODUCT_DEFINITION('Block','Block',#63577,#63447);
#63480=PRODUCT_DEFINITION('End cap +','End cap +',#63578,#63447);
#63481=PRODUCT_DEFINITION('End cap','End cap',#63579,#63447);
#63482=PRODUCT_DEFINITION('Flat Washer - M5','Flat Washer - M5',#63580,
#63447);
#63483=PRODUCT_DEFINITION('M5x30 frame screw','M5x30 frame screw',#63581,
#63447);
#63484=PRODUCT_DEFINITION('Flanged lead nut','Flanged lead nut',#63582,
#63447);
#63485=PRODUCT_DEFINITION('Cap Screw - M4x16','Cap Screw - M4x16',#63583,
#63447);
#63486=PRODUCT_DEFINITION('Cap Screw - M5x20','Cap Screw - M5x20',#63584,
#63447);
#63487=PRODUCT_DEFINITION('Lead screw and handwheel',
'Lead screw and handwheel',#63585,#63447);
#63488=PRODUCT_DEFINITION('X Stage - 01 Supported TR12x3 screw',
'X Stage - 01 Supported TR12x3 screw',#63586,#63447);
#63489=PRODUCT_DEFINITION('Inner race spacer','Inner race spacer',#63587,
#63447);
#63490=PRODUCT_DEFINITION('Shaft retaining collar',
'Shaft retaining collar',#63588,#63447);
#63491=PRODUCT_DEFINITION('Handwheel','Handwheel',#63589,#63447);
#63492=PRODUCT_DEFINITION('Handle pivot sleeve','Handle pivot sleeve',#63590,
#63447);
#63493=PRODUCT_DEFINITION('Revolving handle','Revolving handle',#63591,
#63447);
#63494=PRODUCT_DEFINITION('Key 6x6x20','Key 6x6x20',#63592,#63447);
#63495=PRODUCT_DEFINITION('Socket Set Screw - M5x8',
'Socket Set Screw - M5x8',#63593,#63447);
#63496=PRODUCT_DEFINITION('Flat Washer - M6','Flat Washer - M6',#63594,
#63447);
#63497=PRODUCT_DEFINITION('Cap Screw - M6x25','Cap Screw - M6x25',#63595,
#63447);
#63498=PRODUCT_DEFINITION('Y feed stage','Y feed stage',#63596,#63447);
#63499=PRODUCT_DEFINITION('Rail and screw supports (1)',
'Rail and screw supports (1)',#63597,#63447);
#63500=PRODUCT_DEFINITION('Y Stage - 02 Base','Y Stage - 02 Base',#63598,
#63447);
#63501=PRODUCT_DEFINITION('Y Stage - 04 Rail adapter',
'Y Stage - 04 Rail adapter',#63599,#63447);
#63502=PRODUCT_DEFINITION('Y Stage - 08 Floating bearing support',
'Y Stage - 08 Floating bearing support',#63600,#63447);
#63503=PRODUCT_DEFINITION('Y Stage - 10 Floating cap',
'Y Stage - 10 Floating cap',#63601,#63447);
#63504=PRODUCT_DEFINITION('Y Stage - 09 Fixed bearing support',
'Y Stage - 09 Fixed bearing support',#63602,#63447);
#63505=PRODUCT_DEFINITION('Y Stage - 11 Fixed cap',
'Y Stage - 11 Fixed cap',#63603,#63447);
#63506=PRODUCT_DEFINITION('Y Stage - 12 End stop',
'Y Stage - 12 End stop',#63604,#63447);
#63507=PRODUCT_DEFINITION('Y Stage - 12 End stop (1)',
'Y Stage - 12 End stop (1)',#63605,#63447);
#63508=PRODUCT_DEFINITION('Linear Guide Rail - 15 mm, 220 mm Long (1)',
'Linear Guide Rail - 15 mm, 220 mm Long (1)',#63606,#63447);
#63509=PRODUCT_DEFINITION('Sealed Ball Bearing - 12 x 32 x 10 mm (1)',
'Sealed Ball Bearing - 12 x 32 x 10 mm (1)',#63607,#63447);
#63510=PRODUCT_DEFINITION('Inner ring (2)','Inner ring (2)',#63608,#63447);
#63511=PRODUCT_DEFINITION('Outer ring (2)','Outer ring (2)',#63609,#63447);
#63512=PRODUCT_DEFINITION('Balls (2)','Balls (2)',#63610,#63447);
#63513=PRODUCT_DEFINITION('Cage (2)','Cage (2)',#63611,#63447);
#63514=PRODUCT_DEFINITION('Seals 2RS (2)','Seals 2RS (2)',#63612,#63447);
#63515=PRODUCT_DEFINITION('Sealed Ball Bearing - 20 x 47 x 14 mm (1)',
'Sealed Ball Bearing - 20 x 47 x 14 mm (1)',#63613,#63447);
#63516=PRODUCT_DEFINITION('Inner ring (1) (1)','Inner ring (1) (1)',#63614,
#63447);
#63517=PRODUCT_DEFINITION('Outer ring (1) (1)','Outer ring (1) (1)',#63615,
#63447);
#63518=PRODUCT_DEFINITION('Balls (1) (1)','Balls (1) (1)',#63616,#63447);
#63519=PRODUCT_DEFINITION('Cage (1) (1)','Cage (1) (1)',#63617,#63447);
#63520=PRODUCT_DEFINITION('Seals 2RS (1) (1)','Seals 2RS (1) (1)',#63618,#63447);
#63521=PRODUCT_DEFINITION('M5x14 Cap Screw','M5x14 Cap Screw',#63619,#63447);
#63522=PRODUCT_DEFINITION('Moving table and nut (1)',
'Moving table and nut (1)',#63620,#63447);
#63523=PRODUCT_DEFINITION('Y Stage - 05 Carriage spacer',
'Y Stage - 05 Carriage spacer',#63621,#63447);
#63524=PRODUCT_DEFINITION('Y Stage - 06 Table','Y Stage - 06 Table',#63622,
#63447);
#63525=PRODUCT_DEFINITION('Y Stage - 07 Nut bracket',
'Y Stage - 07 Nut bracket',#63623,#63447);
#63526=PRODUCT_DEFINITION('Flanged Linear Guide Carriage - 15 mm (1)',
'Flanged Linear Guide Carriage - 15 mm (1)',#63624,#63447);
#63527=PRODUCT_DEFINITION('Block (1)','Block (1)',#63625,#63447);
#63528=PRODUCT_DEFINITION('End cap + (1)','End cap + (1)',#63626,#63447);
#63529=PRODUCT_DEFINITION('End cap (1)','End cap (1)',#63627,#63447);
#63530=PRODUCT_DEFINITION('Flat Washer - M5 (1)','Flat Washer - M5 (1)',#63628,
#63447);
#63531=PRODUCT_DEFINITION('M5x30 frame screw (1)','M5x30 frame screw (1)',
#63629,#63447);
#63532=PRODUCT_DEFINITION('Flanged lead nut (1)','Flanged lead nut (1)',#63630,
#63447);
#63533=PRODUCT_DEFINITION('Cap Screw - M4x16 (1)','Cap Screw - M4x16 (1)',
#63631,#63447);
#63534=PRODUCT_DEFINITION('Cap Screw - M5x20 (1)','Cap Screw - M5x20 (1)',
#63632,#63447);
#63535=PRODUCT_DEFINITION('Lead screw and handwheel (1)',
'Lead screw and handwheel (1)',#63633,#63447);
#63536=PRODUCT_DEFINITION('Y Stage - 01 Supported TR12x3 screw',
'Y Stage - 01 Supported TR12x3 screw',#63634,#63447);
#63537=PRODUCT_DEFINITION('Inner race spacer (1)','Inner race spacer (1)',
#63635,#63447);
#63538=PRODUCT_DEFINITION('Shaft retaining collar (1)',
'Shaft retaining collar (1)',#63636,#63447);
#63539=PRODUCT_DEFINITION('Handwheel (1)','Handwheel (1)',#63637,#63447);
#63540=PRODUCT_DEFINITION('Handle pivot sleeve (1)',
'Handle pivot sleeve (1)',#63638,#63447);
#63541=PRODUCT_DEFINITION('Revolving handle (1)','Revolving handle (1)',#63639,
#63447);
#63542=PRODUCT_DEFINITION('Key 6x6x20 (1)','Key 6x6x20 (1)',#63640,#63447);
#63543=PRODUCT_DEFINITION('Socket Set Screw - M5x8 (1)',
'Socket Set Screw - M5x8 (1)',#63641,#63447);
#63544=PRODUCT_DEFINITION('Flat Washer - M6 (1)','Flat Washer - M6 (1)',#63642,
#63447);
#63545=PRODUCT_DEFINITION('Cap Screw - M6x25 (1)','Cap Screw - M6x25 (1)',
#63643,#63447);
#63546=PRODUCT_DEFINITION_FORMATION('',$,#63745);
#63547=PRODUCT_DEFINITION_FORMATION('',$,#63746);
#63548=PRODUCT_DEFINITION_FORMATION('',$,#63747);
#63549=PRODUCT_DEFINITION_FORMATION('',$,#63748);
#63550=PRODUCT_DEFINITION_FORMATION('',$,#63749);
#63551=PRODUCT_DEFINITION_FORMATION('',$,#63750);
#63552=PRODUCT_DEFINITION_FORMATION('',$,#63751);
#63553=PRODUCT_DEFINITION_FORMATION('',$,#63752);
#63554=PRODUCT_DEFINITION_FORMATION('',$,#63753);
#63555=PRODUCT_DEFINITION_FORMATION('',$,#63754);
#63556=PRODUCT_DEFINITION_FORMATION('',$,#63755);
#63557=PRODUCT_DEFINITION_FORMATION('',$,#63756);
#63558=PRODUCT_DEFINITION_FORMATION('',$,#63757);
#63559=PRODUCT_DEFINITION_FORMATION('',$,#63758);
#63560=PRODUCT_DEFINITION_FORMATION('',$,#63759);
#63561=PRODUCT_DEFINITION_FORMATION('',$,#63760);
#63562=PRODUCT_DEFINITION_FORMATION('',$,#63761);
#63563=PRODUCT_DEFINITION_FORMATION('',$,#63762);
#63564=PRODUCT_DEFINITION_FORMATION('',$,#63763);
#63565=PRODUCT_DEFINITION_FORMATION('',$,#63764);
#63566=PRODUCT_DEFINITION_FORMATION('',$,#63765);
#63567=PRODUCT_DEFINITION_FORMATION('',$,#63766);
#63568=PRODUCT_DEFINITION_FORMATION('',$,#63767);
#63569=PRODUCT_DEFINITION_FORMATION('',$,#63768);
#63570=PRODUCT_DEFINITION_FORMATION('',$,#63769);
#63571=PRODUCT_DEFINITION_FORMATION('',$,#63770);
#63572=PRODUCT_DEFINITION_FORMATION('',$,#63771);
#63573=PRODUCT_DEFINITION_FORMATION('',$,#63772);
#63574=PRODUCT_DEFINITION_FORMATION('',$,#63773);
#63575=PRODUCT_DEFINITION_FORMATION('',$,#63774);
#63576=PRODUCT_DEFINITION_FORMATION('',$,#63775);
#63577=PRODUCT_DEFINITION_FORMATION('',$,#63776);
#63578=PRODUCT_DEFINITION_FORMATION('',$,#63777);
#63579=PRODUCT_DEFINITION_FORMATION('',$,#63778);
#63580=PRODUCT_DEFINITION_FORMATION('',$,#63779);
#63581=PRODUCT_DEFINITION_FORMATION('',$,#63780);
#63582=PRODUCT_DEFINITION_FORMATION('',$,#63781);
#63583=PRODUCT_DEFINITION_FORMATION('',$,#63782);
#63584=PRODUCT_DEFINITION_FORMATION('',$,#63783);
#63585=PRODUCT_DEFINITION_FORMATION('',$,#63784);
#63586=PRODUCT_DEFINITION_FORMATION('',$,#63785);
#63587=PRODUCT_DEFINITION_FORMATION('',$,#63786);
#63588=PRODUCT_DEFINITION_FORMATION('',$,#63787);
#63589=PRODUCT_DEFINITION_FORMATION('',$,#63788);
#63590=PRODUCT_DEFINITION_FORMATION('',$,#63789);
#63591=PRODUCT_DEFINITION_FORMATION('',$,#63790);
#63592=PRODUCT_DEFINITION_FORMATION('',$,#63791);
#63593=PRODUCT_DEFINITION_FORMATION('',$,#63792);
#63594=PRODUCT_DEFINITION_FORMATION('',$,#63793);
#63595=PRODUCT_DEFINITION_FORMATION('',$,#63794);
#63596=PRODUCT_DEFINITION_FORMATION('',$,#63795);
#63597=PRODUCT_DEFINITION_FORMATION('',$,#63796);
#63598=PRODUCT_DEFINITION_FORMATION('',$,#63797);
#63599=PRODUCT_DEFINITION_FORMATION('',$,#63798);
#63600=PRODUCT_DEFINITION_FORMATION('',$,#63799);
#63601=PRODUCT_DEFINITION_FORMATION('',$,#63800);
#63602=PRODUCT_DEFINITION_FORMATION('',$,#63801);
#63603=PRODUCT_DEFINITION_FORMATION('',$,#63802);
#63604=PRODUCT_DEFINITION_FORMATION('',$,#63803);
#63605=PRODUCT_DEFINITION_FORMATION('',$,#63804);
#63606=PRODUCT_DEFINITION_FORMATION('',$,#63805);
#63607=PRODUCT_DEFINITION_FORMATION('',$,#63806);
#63608=PRODUCT_DEFINITION_FORMATION('',$,#63807);
#63609=PRODUCT_DEFINITION_FORMATION('',$,#63808);
#63610=PRODUCT_DEFINITION_FORMATION('',$,#63809);
#63611=PRODUCT_DEFINITION_FORMATION('',$,#63810);
#63612=PRODUCT_DEFINITION_FORMATION('',$,#63811);
#63613=PRODUCT_DEFINITION_FORMATION('',$,#63812);
#63614=PRODUCT_DEFINITION_FORMATION('',$,#63813);
#63615=PRODUCT_DEFINITION_FORMATION('',$,#63814);
#63616=PRODUCT_DEFINITION_FORMATION('',$,#63815);
#63617=PRODUCT_DEFINITION_FORMATION('',$,#63816);
#63618=PRODUCT_DEFINITION_FORMATION('',$,#63817);
#63619=PRODUCT_DEFINITION_FORMATION('',$,#63818);
#63620=PRODUCT_DEFINITION_FORMATION('',$,#63819);
#63621=PRODUCT_DEFINITION_FORMATION('',$,#63820);
#63622=PRODUCT_DEFINITION_FORMATION('',$,#63821);
#63623=PRODUCT_DEFINITION_FORMATION('',$,#63822);
#63624=PRODUCT_DEFINITION_FORMATION('',$,#63823);
#63625=PRODUCT_DEFINITION_FORMATION('',$,#63824);
#63626=PRODUCT_DEFINITION_FORMATION('',$,#63825);
#63627=PRODUCT_DEFINITION_FORMATION('',$,#63826);
#63628=PRODUCT_DEFINITION_FORMATION('',$,#63827);
#63629=PRODUCT_DEFINITION_FORMATION('',$,#63828);
#63630=PRODUCT_DEFINITION_FORMATION('',$,#63829);
#63631=PRODUCT_DEFINITION_FORMATION('',$,#63830);
#63632=PRODUCT_DEFINITION_FORMATION('',$,#63831);
#63633=PRODUCT_DEFINITION_FORMATION('',$,#63832);
#63634=PRODUCT_DEFINITION_FORMATION('',$,#63833);
#63635=PRODUCT_DEFINITION_FORMATION('',$,#63834);
#63636=PRODUCT_DEFINITION_FORMATION('',$,#63835);
#63637=PRODUCT_DEFINITION_FORMATION('',$,#63836);
#63638=PRODUCT_DEFINITION_FORMATION('',$,#63837);
#63639=PRODUCT_DEFINITION_FORMATION('',$,#63838);
#63640=PRODUCT_DEFINITION_FORMATION('',$,#63839);
#63641=PRODUCT_DEFINITION_FORMATION('',$,#63840);
#63642=PRODUCT_DEFINITION_FORMATION('',$,#63841);
#63643=PRODUCT_DEFINITION_FORMATION('',$,#63842);
#63644=PRODUCT_RELATED_PRODUCT_CATEGORY('PAT-124','PAT-124',(#63745));
#63645=PRODUCT_RELATED_PRODUCT_CATEGORY('X feed stage','X feed stage',(#63746));
#63646=PRODUCT_RELATED_PRODUCT_CATEGORY('Rail and screw supports',
'Rail and screw supports',(#63747));
#63647=PRODUCT_RELATED_PRODUCT_CATEGORY('X Stage - 02 Base',
'X Stage - 02 Base',(#63748));
#63648=PRODUCT_RELATED_PRODUCT_CATEGORY('X Stage - 03 Bonded skid',
'X Stage - 03 Bonded skid',(#63749));
#63649=PRODUCT_RELATED_PRODUCT_CATEGORY('X Stage - 03 Bonded skid (1)',
'X Stage - 03 Bonded skid (1)',(#63750));
#63650=PRODUCT_RELATED_PRODUCT_CATEGORY('X Stage - 04 Rail adapter',
'X Stage - 04 Rail adapter',(#63751));
#63651=PRODUCT_RELATED_PRODUCT_CATEGORY(
'X Stage - 08 Floating bearing support',
'X Stage - 08 Floating bearing support',(#63752));
#63652=PRODUCT_RELATED_PRODUCT_CATEGORY('X Stage - 10 Floating cap',
'X Stage - 10 Floating cap',(#63753));
#63653=PRODUCT_RELATED_PRODUCT_CATEGORY(
'X Stage - 09 Fixed bearing support',
'X Stage - 09 Fixed bearing support',(#63754));
#63654=PRODUCT_RELATED_PRODUCT_CATEGORY('X Stage - 11 Fixed cap',
'X Stage - 11 Fixed cap',(#63755));
#63655=PRODUCT_RELATED_PRODUCT_CATEGORY('X Stage - 12 End stop',
'X Stage - 12 End stop',(#63756));
#63656=PRODUCT_RELATED_PRODUCT_CATEGORY('X Stage - 12 End stop (1)',
'X Stage - 12 End stop (1)',(#63757));
#63657=PRODUCT_RELATED_PRODUCT_CATEGORY(
'Linear Guide Rail - 15 mm, 220 mm Long',
'Linear Guide Rail - 15 mm, 220 mm Long',(#63758));
#63658=PRODUCT_RELATED_PRODUCT_CATEGORY(
'Sealed Ball Bearing - 12 x 32 x 10 mm',
'Sealed Ball Bearing - 12 x 32 x 10 mm',(#63759));
#63659=PRODUCT_RELATED_PRODUCT_CATEGORY('Inner ring','Inner ring',(#63760));
#63660=PRODUCT_RELATED_PRODUCT_CATEGORY('Outer ring','Outer ring',(#63761));
#63661=PRODUCT_RELATED_PRODUCT_CATEGORY('Balls','Balls',(#63762));
#63662=PRODUCT_RELATED_PRODUCT_CATEGORY('Cage','Cage',(#63763));
#63663=PRODUCT_RELATED_PRODUCT_CATEGORY('Seals 2RS','Seals 2RS',(#63764));
#63664=PRODUCT_RELATED_PRODUCT_CATEGORY(
'Sealed Ball Bearing - 20 x 47 x 14 mm',
'Sealed Ball Bearing - 20 x 47 x 14 mm',(#63765));
#63665=PRODUCT_RELATED_PRODUCT_CATEGORY('Inner ring (1)',
'Inner ring (1)',(#63766));
#63666=PRODUCT_RELATED_PRODUCT_CATEGORY('Outer ring (1)',
'Outer ring (1)',(#63767));
#63667=PRODUCT_RELATED_PRODUCT_CATEGORY('Balls (1)','Balls (1)',(#63768));
#63668=PRODUCT_RELATED_PRODUCT_CATEGORY('Cage (1)','Cage (1)',(#63769));
#63669=PRODUCT_RELATED_PRODUCT_CATEGORY('Seals 2RS (1)','Seals 2RS (1)',
(#63770));
#63670=PRODUCT_RELATED_PRODUCT_CATEGORY('Moving table and nut',
'Moving table and nut',(#63771));
#63671=PRODUCT_RELATED_PRODUCT_CATEGORY('X Stage - 05 Carriage spacer',
'X Stage - 05 Carriage spacer',(#63772));
#63672=PRODUCT_RELATED_PRODUCT_CATEGORY('X Stage - 06 Table',
'X Stage - 06 Table',(#63773));
#63673=PRODUCT_RELATED_PRODUCT_CATEGORY('X Stage - 07 Nut bracket',
'X Stage - 07 Nut bracket',(#63774));
#63674=PRODUCT_RELATED_PRODUCT_CATEGORY(
'Flanged Linear Guide Carriage - 15 mm',
'Flanged Linear Guide Carriage - 15 mm',(#63775));
#63675=PRODUCT_RELATED_PRODUCT_CATEGORY('Block','Block',(#63776));
#63676=PRODUCT_RELATED_PRODUCT_CATEGORY('End cap +','End cap +',(#63777));
#63677=PRODUCT_RELATED_PRODUCT_CATEGORY('End cap','End cap',(#63778));
#63678=PRODUCT_RELATED_PRODUCT_CATEGORY('Flat Washer - M5',
'Flat Washer - M5',(#63779));
#63679=PRODUCT_RELATED_PRODUCT_CATEGORY('M5x30 frame screw',
'M5x30 frame screw',(#63780));
#63680=PRODUCT_RELATED_PRODUCT_CATEGORY('Flanged lead nut',
'Flanged lead nut',(#63781));
#63681=PRODUCT_RELATED_PRODUCT_CATEGORY('Cap Screw - M4x16',
'Cap Screw - M4x16',(#63782));
#63682=PRODUCT_RELATED_PRODUCT_CATEGORY('Cap Screw - M5x20',
'Cap Screw - M5x20',(#63783));
#63683=PRODUCT_RELATED_PRODUCT_CATEGORY('Lead screw and handwheel',
'Lead screw and handwheel',(#63784));
#63684=PRODUCT_RELATED_PRODUCT_CATEGORY(
'X Stage - 01 Supported TR12x3 screw',
'X Stage - 01 Supported TR12x3 screw',(#63785));
#63685=PRODUCT_RELATED_PRODUCT_CATEGORY('Inner race spacer',
'Inner race spacer',(#63786));
#63686=PRODUCT_RELATED_PRODUCT_CATEGORY('Shaft retaining collar',
'Shaft retaining collar',(#63787));
#63687=PRODUCT_RELATED_PRODUCT_CATEGORY('Handwheel','Handwheel',(#63788));
#63688=PRODUCT_RELATED_PRODUCT_CATEGORY('Handle pivot sleeve',
'Handle pivot sleeve',(#63789));
#63689=PRODUCT_RELATED_PRODUCT_CATEGORY('Revolving handle',
'Revolving handle',(#63790));
#63690=PRODUCT_RELATED_PRODUCT_CATEGORY('Key 6x6x20','Key 6x6x20',(#63791));
#63691=PRODUCT_RELATED_PRODUCT_CATEGORY('Socket Set Screw - M5x8',
'Socket Set Screw - M5x8',(#63792));
#63692=PRODUCT_RELATED_PRODUCT_CATEGORY('Flat Washer - M6',
'Flat Washer - M6',(#63793));
#63693=PRODUCT_RELATED_PRODUCT_CATEGORY('Cap Screw - M6x25',
'Cap Screw - M6x25',(#63794));
#63694=PRODUCT_RELATED_PRODUCT_CATEGORY('Y feed stage','Y feed stage',(#63795));
#63695=PRODUCT_RELATED_PRODUCT_CATEGORY('Rail and screw supports (1)',
'Rail and screw supports (1)',(#63796));
#63696=PRODUCT_RELATED_PRODUCT_CATEGORY('Y Stage - 02 Base',
'Y Stage - 02 Base',(#63797));
#63697=PRODUCT_RELATED_PRODUCT_CATEGORY('Y Stage - 04 Rail adapter',
'Y Stage - 04 Rail adapter',(#63798));
#63698=PRODUCT_RELATED_PRODUCT_CATEGORY(
'Y Stage - 08 Floating bearing support',
'Y Stage - 08 Floating bearing support',(#63799));
#63699=PRODUCT_RELATED_PRODUCT_CATEGORY('Y Stage - 10 Floating cap',
'Y Stage - 10 Floating cap',(#63800));
#63700=PRODUCT_RELATED_PRODUCT_CATEGORY(
'Y Stage - 09 Fixed bearing support',
'Y Stage - 09 Fixed bearing support',(#63801));
#63701=PRODUCT_RELATED_PRODUCT_CATEGORY('Y Stage - 11 Fixed cap',
'Y Stage - 11 Fixed cap',(#63802));
#63702=PRODUCT_RELATED_PRODUCT_CATEGORY('Y Stage - 12 End stop',
'Y Stage - 12 End stop',(#63803));
#63703=PRODUCT_RELATED_PRODUCT_CATEGORY('Y Stage - 12 End stop (1)',
'Y Stage - 12 End stop (1)',(#63804));
#63704=PRODUCT_RELATED_PRODUCT_CATEGORY(
'Linear Guide Rail - 15 mm, 220 mm Long (1)',
'Linear Guide Rail - 15 mm, 220 mm Long (1)',(#63805));
#63705=PRODUCT_RELATED_PRODUCT_CATEGORY(
'Sealed Ball Bearing - 12 x 32 x 10 mm (1)',
'Sealed Ball Bearing - 12 x 32 x 10 mm (1)',(#63806));
#63706=PRODUCT_RELATED_PRODUCT_CATEGORY('Inner ring (2)',
'Inner ring (2)',(#63807));
#63707=PRODUCT_RELATED_PRODUCT_CATEGORY('Outer ring (2)',
'Outer ring (2)',(#63808));
#63708=PRODUCT_RELATED_PRODUCT_CATEGORY('Balls (2)','Balls (2)',(#63809));
#63709=PRODUCT_RELATED_PRODUCT_CATEGORY('Cage (2)','Cage (2)',(#63810));
#63710=PRODUCT_RELATED_PRODUCT_CATEGORY('Seals 2RS (2)','Seals 2RS (2)',
(#63811));
#63711=PRODUCT_RELATED_PRODUCT_CATEGORY(
'Sealed Ball Bearing - 20 x 47 x 14 mm (1)',
'Sealed Ball Bearing - 20 x 47 x 14 mm (1)',(#63812));
#63712=PRODUCT_RELATED_PRODUCT_CATEGORY('Inner ring (1) (1)',
'Inner ring (1) (1)',(#63813));
#63713=PRODUCT_RELATED_PRODUCT_CATEGORY('Outer ring (1) (1)',
'Outer ring (1) (1)',(#63814));
#63714=PRODUCT_RELATED_PRODUCT_CATEGORY('Balls (1) (1)','Balls (1) (1)',
(#63815));
#63715=PRODUCT_RELATED_PRODUCT_CATEGORY('Cage (1) (1)','Cage (1) (1)',(#63816));
#63716=PRODUCT_RELATED_PRODUCT_CATEGORY('Seals 2RS (1) (1)',
'Seals 2RS (1) (1)',(#63817));
#63717=PRODUCT_RELATED_PRODUCT_CATEGORY('M5x14 Cap Screw',
'M5x14 Cap Screw',(#63818));
#63718=PRODUCT_RELATED_PRODUCT_CATEGORY('Moving table and nut (1)',
'Moving table and nut (1)',(#63819));
#63719=PRODUCT_RELATED_PRODUCT_CATEGORY('Y Stage - 05 Carriage spacer',
'Y Stage - 05 Carriage spacer',(#63820));
#63720=PRODUCT_RELATED_PRODUCT_CATEGORY('Y Stage - 06 Table',
'Y Stage - 06 Table',(#63821));
#63721=PRODUCT_RELATED_PRODUCT_CATEGORY('Y Stage - 07 Nut bracket',
'Y Stage - 07 Nut bracket',(#63822));
#63722=PRODUCT_RELATED_PRODUCT_CATEGORY(
'Flanged Linear Guide Carriage - 15 mm (1)',
'Flanged Linear Guide Carriage - 15 mm (1)',(#63823));
#63723=PRODUCT_RELATED_PRODUCT_CATEGORY('Block (1)','Block (1)',(#63824));
#63724=PRODUCT_RELATED_PRODUCT_CATEGORY('End cap + (1)','End cap + (1)',
(#63825));
#63725=PRODUCT_RELATED_PRODUCT_CATEGORY('End cap (1)','End cap (1)',(#63826));
#63726=PRODUCT_RELATED_PRODUCT_CATEGORY('Flat Washer - M5 (1)',
'Flat Washer - M5 (1)',(#63827));
#63727=PRODUCT_RELATED_PRODUCT_CATEGORY('M5x30 frame screw (1)',
'M5x30 frame screw (1)',(#63828));
#63728=PRODUCT_RELATED_PRODUCT_CATEGORY('Flanged lead nut (1)',
'Flanged lead nut (1)',(#63829));
#63729=PRODUCT_RELATED_PRODUCT_CATEGORY('Cap Screw - M4x16 (1)',
'Cap Screw - M4x16 (1)',(#63830));
#63730=PRODUCT_RELATED_PRODUCT_CATEGORY('Cap Screw - M5x20 (1)',
'Cap Screw - M5x20 (1)',(#63831));
#63731=PRODUCT_RELATED_PRODUCT_CATEGORY('Lead screw and handwheel (1)',
'Lead screw and handwheel (1)',(#63832));
#63732=PRODUCT_RELATED_PRODUCT_CATEGORY(
'Y Stage - 01 Supported TR12x3 screw',
'Y Stage - 01 Supported TR12x3 screw',(#63833));
#63733=PRODUCT_RELATED_PRODUCT_CATEGORY('Inner race spacer (1)',
'Inner race spacer (1)',(#63834));
#63734=PRODUCT_RELATED_PRODUCT_CATEGORY('Shaft retaining collar (1)',
'Shaft retaining collar (1)',(#63835));
#63735=PRODUCT_RELATED_PRODUCT_CATEGORY('Handwheel (1)','Handwheel (1)',
(#63836));
#63736=PRODUCT_RELATED_PRODUCT_CATEGORY('Handle pivot sleeve (1)',
'Handle pivot sleeve (1)',(#63837));
#63737=PRODUCT_RELATED_PRODUCT_CATEGORY('Revolving handle (1)',
'Revolving handle (1)',(#63838));
#63738=PRODUCT_RELATED_PRODUCT_CATEGORY('Key 6x6x20 (1)',
'Key 6x6x20 (1)',(#63839));
#63739=PRODUCT_RELATED_PRODUCT_CATEGORY('Socket Set Screw - M5x8 (1)',
'Socket Set Screw - M5x8 (1)',(#63840));
#63740=PRODUCT_RELATED_PRODUCT_CATEGORY('Flat Washer - M6 (1)',
'Flat Washer - M6 (1)',(#63841));
#63741=PRODUCT_RELATED_PRODUCT_CATEGORY('Cap Screw - M6x25 (1)',
'Cap Screw - M6x25 (1)',(#63842));
#63742=APPLICATION_PROTOCOL_DEFINITION('international standard',
'automotive_design',2009,#63743);
#63743=APPLICATION_CONTEXT(
'Core Data for Automotive Mechanical Design Process');
#63744=PRODUCT_CONTEXT('part definition',#63743,'mechanical');
#63745=PRODUCT('PAT-124','PAT-124','PAT-124',
(#63744));
#63746=PRODUCT('X feed stage','X feed stage','X feed stage',(#63744));
#63747=PRODUCT('Rail and screw supports','Rail and screw supports',
'Rail and screw supports',(#63744));
#63748=PRODUCT('X Stage - 02 Base','X Stage - 02 Base',
'X Stage - 02 Base',(#63744));
#63749=PRODUCT('X Stage - 03 Bonded skid','X Stage - 03 Bonded skid',
'X Stage - 03 Bonded skid',(#63744));
#63750=PRODUCT('X Stage - 03 Bonded skid (1)',
'X Stage - 03 Bonded skid (1)','X Stage - 03 Bonded skid (1)',(#63744));
#63751=PRODUCT('X Stage - 04 Rail adapter','X Stage - 04 Rail adapter',
'X Stage - 04 Rail adapter',(#63744));
#63752=PRODUCT('X Stage - 08 Floating bearing support',
'X Stage - 08 Floating bearing support',
'X Stage - 08 Floating bearing support',(#63744));
#63753=PRODUCT('X Stage - 10 Floating cap','X Stage - 10 Floating cap',
'X Stage - 10 Floating cap',(#63744));
#63754=PRODUCT('X Stage - 09 Fixed bearing support',
'X Stage - 09 Fixed bearing support',
'X Stage - 09 Fixed bearing support',(#63744));
#63755=PRODUCT('X Stage - 11 Fixed cap','X Stage - 11 Fixed cap',
'X Stage - 11 Fixed cap',(#63744));
#63756=PRODUCT('X Stage - 12 End stop','X Stage - 12 End stop',
'X Stage - 12 End stop',(#63744));
#63757=PRODUCT('X Stage - 12 End stop (1)','X Stage - 12 End stop (1)',
'X Stage - 12 End stop (1)',(#63744));
#63758=PRODUCT('Linear Guide Rail - 15 mm, 220 mm Long',
'Linear Guide Rail - 15 mm, 220 mm Long',
'Linear Guide Rail - 15 mm, 220 mm Long',(#63744));
#63759=PRODUCT('Sealed Ball Bearing - 12 x 32 x 10 mm',
'Sealed Ball Bearing - 12 x 32 x 10 mm',
'Sealed Ball Bearing - 12 x 32 x 10 mm',(#63744));
#63760=PRODUCT('Inner ring','Inner ring','Inner ring',(#63744));
#63761=PRODUCT('Outer ring','Outer ring','Outer ring',(#63744));
#63762=PRODUCT('Balls','Balls','Balls',(#63744));
#63763=PRODUCT('Cage','Cage','Cage',(#63744));
#63764=PRODUCT('Seals 2RS','Seals 2RS','Seals 2RS',(#63744));
#63765=PRODUCT('Sealed Ball Bearing - 20 x 47 x 14 mm',
'Sealed Ball Bearing - 20 x 47 x 14 mm',
'Sealed Ball Bearing - 20 x 47 x 14 mm',(#63744));
#63766=PRODUCT('Inner ring (1)','Inner ring (1)','Inner ring (1)',(#63744));
#63767=PRODUCT('Outer ring (1)','Outer ring (1)','Outer ring (1)',(#63744));
#63768=PRODUCT('Balls (1)','Balls (1)','Balls (1)',(#63744));
#63769=PRODUCT('Cage (1)','Cage (1)','Cage (1)',(#63744));
#63770=PRODUCT('Seals 2RS (1)','Seals 2RS (1)','Seals 2RS (1)',(#63744));
#63771=PRODUCT('Moving table and nut','Moving table and nut',
'Moving table and nut',(#63744));
#63772=PRODUCT('X Stage - 05 Carriage spacer',
'X Stage - 05 Carriage spacer','X Stage - 05 Carriage spacer',(#63744));
#63773=PRODUCT('X Stage - 06 Table','X Stage - 06 Table',
'X Stage - 06 Table',(#63744));
#63774=PRODUCT('X Stage - 07 Nut bracket','X Stage - 07 Nut bracket',
'X Stage - 07 Nut bracket',(#63744));
#63775=PRODUCT('Flanged Linear Guide Carriage - 15 mm',
'Flanged Linear Guide Carriage - 15 mm',
'Flanged Linear Guide Carriage - 15 mm',(#63744));
#63776=PRODUCT('Block','Block','Block',(#63744));
#63777=PRODUCT('End cap +','End cap +','End cap +',(#63744));
#63778=PRODUCT('End cap','End cap','End cap',(#63744));
#63779=PRODUCT('Flat Washer - M5','Flat Washer - M5','Flat Washer - M5',
(#63744));
#63780=PRODUCT('M5x30 frame screw','M5x30 frame screw',
'M5x30 frame screw',(#63744));
#63781=PRODUCT('Flanged lead nut','Flanged lead nut','Flanged lead nut',
(#63744));
#63782=PRODUCT('Cap Screw - M4x16','Cap Screw - M4x16',
'Cap Screw - M4x16',(#63744));
#63783=PRODUCT('Cap Screw - M5x20','Cap Screw - M5x20',
'Cap Screw - M5x20',(#63744));
#63784=PRODUCT('Lead screw and handwheel','Lead screw and handwheel',
'Lead screw and handwheel',(#63744));
#63785=PRODUCT('X Stage - 01 Supported TR12x3 screw',
'X Stage - 01 Supported TR12x3 screw',
'X Stage - 01 Supported TR12x3 screw',(#63744));
#63786=PRODUCT('Inner race spacer','Inner race spacer',
'Inner race spacer',(#63744));
#63787=PRODUCT('Shaft retaining collar','Shaft retaining collar',
'Shaft retaining collar',(#63744));
#63788=PRODUCT('Handwheel','Handwheel','Handwheel',(#63744));
#63789=PRODUCT('Handle pivot sleeve','Handle pivot sleeve',
'Handle pivot sleeve',(#63744));
#63790=PRODUCT('Revolving handle','Revolving handle','Revolving handle',
(#63744));
#63791=PRODUCT('Key 6x6x20','Key 6x6x20','Key 6x6x20',(#63744));
#63792=PRODUCT('Socket Set Screw - M5x8','Socket Set Screw - M5x8',
'Socket Set Screw - M5x8',(#63744));
#63793=PRODUCT('Flat Washer - M6','Flat Washer - M6','Flat Washer - M6',
(#63744));
#63794=PRODUCT('Cap Screw - M6x25','Cap Screw - M6x25',
'Cap Screw - M6x25',(#63744));
#63795=PRODUCT('Y feed stage','Y feed stage','Y feed stage',(#63744));
#63796=PRODUCT('Rail and screw supports (1)',
'Rail and screw supports (1)','Rail and screw supports (1)',(#63744));
#63797=PRODUCT('Y Stage - 02 Base','Y Stage - 02 Base',
'Y Stage - 02 Base',(#63744));
#63798=PRODUCT('Y Stage - 04 Rail adapter','Y Stage - 04 Rail adapter',
'Y Stage - 04 Rail adapter',(#63744));
#63799=PRODUCT('Y Stage - 08 Floating bearing support',
'Y Stage - 08 Floating bearing support',
'Y Stage - 08 Floating bearing support',(#63744));
#63800=PRODUCT('Y Stage - 10 Floating cap','Y Stage - 10 Floating cap',
'Y Stage - 10 Floating cap',(#63744));
#63801=PRODUCT('Y Stage - 09 Fixed bearing support',
'Y Stage - 09 Fixed bearing support',
'Y Stage - 09 Fixed bearing support',(#63744));
#63802=PRODUCT('Y Stage - 11 Fixed cap','Y Stage - 11 Fixed cap',
'Y Stage - 11 Fixed cap',(#63744));
#63803=PRODUCT('Y Stage - 12 End stop','Y Stage - 12 End stop',
'Y Stage - 12 End stop',(#63744));
#63804=PRODUCT('Y Stage - 12 End stop (1)','Y Stage - 12 End stop (1)',
'Y Stage - 12 End stop (1)',(#63744));
#63805=PRODUCT('Linear Guide Rail - 15 mm, 220 mm Long (1)',
'Linear Guide Rail - 15 mm, 220 mm Long (1)',
'Linear Guide Rail - 15 mm, 220 mm Long (1)',(#63744));
#63806=PRODUCT('Sealed Ball Bearing - 12 x 32 x 10 mm (1)',
'Sealed Ball Bearing - 12 x 32 x 10 mm (1)',
'Sealed Ball Bearing - 12 x 32 x 10 mm (1)',(#63744));
#63807=PRODUCT('Inner ring (2)','Inner ring (2)','Inner ring (2)',(#63744));
#63808=PRODUCT('Outer ring (2)','Outer ring (2)','Outer ring (2)',(#63744));
#63809=PRODUCT('Balls (2)','Balls (2)','Balls (2)',(#63744));
#63810=PRODUCT('Cage (2)','Cage (2)','Cage (2)',(#63744));
#63811=PRODUCT('Seals 2RS (2)','Seals 2RS (2)','Seals 2RS (2)',(#63744));
#63812=PRODUCT('Sealed Ball Bearing - 20 x 47 x 14 mm (1)',
'Sealed Ball Bearing - 20 x 47 x 14 mm (1)',
'Sealed Ball Bearing - 20 x 47 x 14 mm (1)',(#63744));
#63813=PRODUCT('Inner ring (1) (1)','Inner ring (1) (1)','Inner ring (1) (1)',(#63744));
#63814=PRODUCT('Outer ring (1) (1)','Outer ring (1) (1)','Outer ring (1) (1)',(#63744));
#63815=PRODUCT('Balls (1) (1)','Balls (1) (1)','Balls (1) (1)',(#63744));
#63816=PRODUCT('Cage (1) (1)','Cage (1) (1)','Cage (1) (1)',(#63744));
#63817=PRODUCT('Seals 2RS (1) (1)','Seals 2RS (1) (1)','Seals 2RS (1) (1)',(#63744));
#63818=PRODUCT('M5x14 Cap Screw','M5x14 Cap Screw','M5x14 Cap Screw',(#63744));
#63819=PRODUCT('Moving table and nut (1)','Moving table and nut (1)',
'Moving table and nut (1)',(#63744));
#63820=PRODUCT('Y Stage - 05 Carriage spacer',
'Y Stage - 05 Carriage spacer','Y Stage - 05 Carriage spacer',(#63744));
#63821=PRODUCT('Y Stage - 06 Table','Y Stage - 06 Table',
'Y Stage - 06 Table',(#63744));
#63822=PRODUCT('Y Stage - 07 Nut bracket','Y Stage - 07 Nut bracket',
'Y Stage - 07 Nut bracket',(#63744));
#63823=PRODUCT('Flanged Linear Guide Carriage - 15 mm (1)',
'Flanged Linear Guide Carriage - 15 mm (1)',
'Flanged Linear Guide Carriage - 15 mm (1)',(#63744));
#63824=PRODUCT('Block (1)','Block (1)','Block (1)',(#63744));
#63825=PRODUCT('End cap + (1)','End cap + (1)','End cap + (1)',(#63744));
#63826=PRODUCT('End cap (1)','End cap (1)','End cap (1)',(#63744));
#63827=PRODUCT('Flat Washer - M5 (1)','Flat Washer - M5 (1)',
'Flat Washer - M5 (1)',(#63744));
#63828=PRODUCT('M5x30 frame screw (1)','M5x30 frame screw (1)',
'M5x30 frame screw (1)',(#63744));
#63829=PRODUCT('Flanged lead nut (1)','Flanged lead nut (1)',
'Flanged lead nut (1)',(#63744));
#63830=PRODUCT('Cap Screw - M4x16 (1)','Cap Screw - M4x16 (1)',
'Cap Screw - M4x16 (1)',(#63744));
#63831=PRODUCT('Cap Screw - M5x20 (1)','Cap Screw - M5x20 (1)',
'Cap Screw - M5x20 (1)',(#63744));
#63832=PRODUCT('Lead screw and handwheel (1)',
'Lead screw and handwheel (1)','Lead screw and handwheel (1)',(#63744));
#63833=PRODUCT('Y Stage - 01 Supported TR12x3 screw',
'Y Stage - 01 Supported TR12x3 screw',
'Y Stage - 01 Supported TR12x3 screw',(#63744));
#63834=PRODUCT('Inner race spacer (1)','Inner race spacer (1)',
'Inner race spacer (1)',(#63744));
#63835=PRODUCT('Shaft retaining collar (1)','Shaft retaining collar (1)',
'Shaft retaining collar (1)',(#63744));
#63836=PRODUCT('Handwheel (1)','Handwheel (1)','Handwheel (1)',(#63744));
#63837=PRODUCT('Handle pivot sleeve (1)','Handle pivot sleeve (1)',
'Handle pivot sleeve (1)',(#63744));
#63838=PRODUCT('Revolving handle (1)','Revolving handle (1)',
'Revolving handle (1)',(#63744));
#63839=PRODUCT('Key 6x6x20 (1)','Key 6x6x20 (1)','Key 6x6x20 (1)',(#63744));
#63840=PRODUCT('Socket Set Screw - M5x8 (1)',
'Socket Set Screw - M5x8 (1)','Socket Set Screw - M5x8 (1)',(#63744));
#63841=PRODUCT('Flat Washer - M6 (1)','Flat Washer - M6 (1)',
'Flat Washer - M6 (1)',(#63744));
#63842=PRODUCT('Cap Screw - M6x25 (1)','Cap Screw - M6x25 (1)',
'Cap Screw - M6x25 (1)',(#63744));
#63843=PRESENTATION_STYLE_ASSIGNMENT((#63849));
#63844=PRESENTATION_STYLE_ASSIGNMENT((#63850));
#63845=PRESENTATION_STYLE_ASSIGNMENT((#63851));
#63846=PRESENTATION_STYLE_ASSIGNMENT((#63852));
#63847=PRESENTATION_STYLE_ASSIGNMENT((#63853));
#63848=PRESENTATION_STYLE_ASSIGNMENT((#63854));
#63849=SURFACE_STYLE_USAGE(.BOTH.,#63855);
#63850=SURFACE_STYLE_USAGE(.BOTH.,#63856);
#63851=SURFACE_STYLE_USAGE(.BOTH.,#63857);
#63852=SURFACE_STYLE_USAGE(.BOTH.,#63858);
#63853=SURFACE_STYLE_USAGE(.BOTH.,#63859);
#63854=SURFACE_STYLE_USAGE(.BOTH.,#63860);
#63855=SURFACE_SIDE_STYLE('',(#63861));
#63856=SURFACE_SIDE_STYLE('',(#63862));
#63857=SURFACE_SIDE_STYLE('',(#63863));
#63858=SURFACE_SIDE_STYLE('',(#63864));
#63859=SURFACE_SIDE_STYLE('',(#63865));
#63860=SURFACE_SIDE_STYLE('',(#63866));
#63861=SURFACE_STYLE_FILL_AREA(#63867);
#63862=SURFACE_STYLE_FILL_AREA(#63868);
#63863=SURFACE_STYLE_FILL_AREA(#63869);
#63864=SURFACE_STYLE_FILL_AREA(#63870);
#63865=SURFACE_STYLE_FILL_AREA(#63871);
#63866=SURFACE_STYLE_FILL_AREA(#63872);
#63867=FILL_AREA_STYLE('Steel - Satin',(#63873));
#63868=FILL_AREA_STYLE('CAD Library Painted - Deep blue',(#63874));
#63869=FILL_AREA_STYLE('CAD Library Painted - Engineering blue',(#63875));
#63870=FILL_AREA_STYLE('CAD Library Painted - Steel gray',(#63876));
#63871=FILL_AREA_STYLE('CAD Library Painted - Light blue',(#63877));
#63872=FILL_AREA_STYLE('CAD Library Painted - Graphite',(#63878));
#63873=FILL_AREA_STYLE_COLOUR('Steel - Satin',#63879);
#63874=FILL_AREA_STYLE_COLOUR('CAD Library Painted - Deep blue',#63880);
#63875=FILL_AREA_STYLE_COLOUR('CAD Library Painted - Engineering blue',
#63881);
#63876=FILL_AREA_STYLE_COLOUR('CAD Library Painted - Steel gray',#63882);
#63877=FILL_AREA_STYLE_COLOUR('CAD Library Painted - Light blue',#63883);
#63878=FILL_AREA_STYLE_COLOUR('CAD Library Painted - Graphite',#63884);
#63879=COLOUR_RGB('Steel - Satin',0.627450980392157,0.627450980392157,0.627450980392157);
#63880=COLOUR_RGB('CAD Library Painted - Deep blue',0.0784313725490196,
0.203921568627451,0.349019607843137);
#63881=COLOUR_RGB('CAD Library Painted - Engineering blue',0.12156862745098,
0.356862745098039,0.6);
#63882=COLOUR_RGB('CAD Library Painted - Steel gray',0.592156862745098,
0.631372549019608,0.67843137254902);
#63883=COLOUR_RGB('CAD Library Painted - Light blue',0.286274509803922,
0.552941176470588,0.780392156862745);
#63884=COLOUR_RGB('CAD Library Painted - Graphite',0.168627450980392,0.192156862745098,
0.231372549019608);
#63885=COLOUR_RGB('Dark Blue',0.08,0.2,0.34);
#63886=FILL_AREA_STYLE_COLOUR('',#63885);
#63887=FILL_AREA_STYLE('',(#63886));
#63888=SURFACE_STYLE_FILL_AREA(#63887);
#63889=SURFACE_SIDE_STYLE('',(#63888));
#63890=SURFACE_STYLE_USAGE(.BOTH.,#63889);
#63891=PRESENTATION_STYLE_ASSIGNMENT((#63890));
#63892=COLOUR_RGB('Light Blue',0.38,0.62,0.78);
#63893=FILL_AREA_STYLE_COLOUR('',#63892);
#63894=FILL_AREA_STYLE('',(#63893));
#63895=SURFACE_STYLE_FILL_AREA(#63894);
#63896=SURFACE_SIDE_STYLE('',(#63895));
#63897=SURFACE_STYLE_USAGE(.BOTH.,#63896);
#63898=PRESENTATION_STYLE_ASSIGNMENT((#63897));
#63899=COLOUR_RGB('Sky Blue',0.24,0.69,0.87);
#63900=FILL_AREA_STYLE_COLOUR('',#63899);
#63901=FILL_AREA_STYLE('',(#63900));
#63902=SURFACE_STYLE_FILL_AREA(#63901);
#63903=SURFACE_SIDE_STYLE('',(#63902));
#63904=SURFACE_STYLE_USAGE(.BOTH.,#63903);
#63905=PRESENTATION_STYLE_ASSIGNMENT((#63904));
#63906=COLOUR_RGB('Grey',0.48,0.52,0.57);
#63907=FILL_AREA_STYLE_COLOUR('',#63906);
#63908=FILL_AREA_STYLE('',(#63907));
#63909=SURFACE_STYLE_FILL_AREA(#63908);
#63910=SURFACE_SIDE_STYLE('',(#63909));
#63911=SURFACE_STYLE_USAGE(.BOTH.,#63910);
#63912=PRESENTATION_STYLE_ASSIGNMENT((#63911));
#63913=COLOUR_RGB('Black',0.12,0.14,0.17);
#63914=FILL_AREA_STYLE_COLOUR('',#63913);
#63915=FILL_AREA_STYLE('',(#63914));
#63916=SURFACE_STYLE_FILL_AREA(#63915);
#63917=SURFACE_SIDE_STYLE('',(#63916));
#63918=SURFACE_STYLE_USAGE(.BOTH.,#63917);
#63919=PRESENTATION_STYLE_ASSIGNMENT((#63918));
#63920=COLOUR_RGB('Off White',0.89,0.88,0.83);
#63921=FILL_AREA_STYLE_COLOUR('',#63920);
#63922=FILL_AREA_STYLE('',(#63921));
#63923=SURFACE_STYLE_FILL_AREA(#63922);
#63924=SURFACE_SIDE_STYLE('',(#63923));
#63925=SURFACE_STYLE_USAGE(.BOTH.,#63924);
#63926=PRESENTATION_STYLE_ASSIGNMENT((#63925));
ENDSEC;
END-ISO-10303-21;
